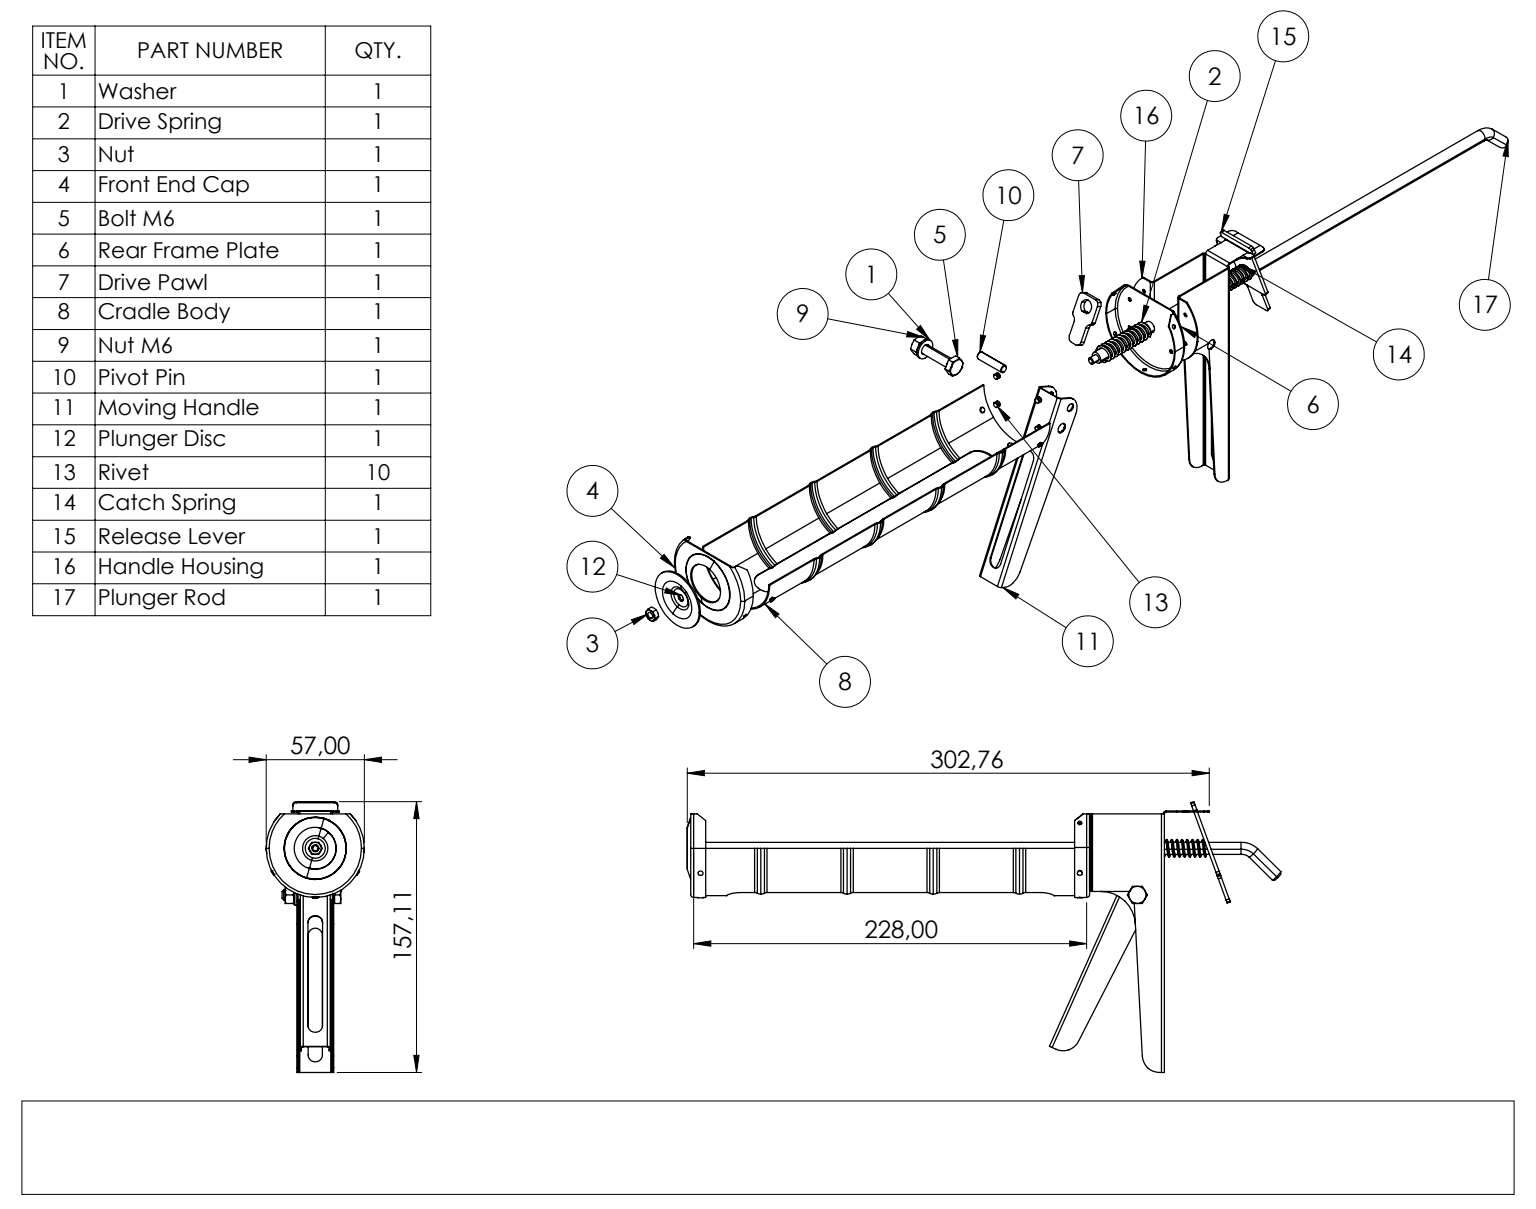
ISO-10303-21;
HEADER;
FILE_DESCRIPTION (('STEP AP214'),
    '1' );
FILE_NAME ('MAS-156',
    '2026-10-06T09:00:30',
    ( '' ),
    ( '' ),
    'SwSTEP 2.0',
    'SolidWorks 2020',
    '' );
FILE_SCHEMA (( 'AUTOMOTIVE_DESIGN' ));
ENDSEC;

DATA;
#1 = CARTESIAN_POINT ( 'NONE',  ( 7.707106781468556100, -5.692566302608600637, -27.29492475672613594 ) ) ;
#2 = DIRECTION ( 'NONE',  ( 0.000000000000000000, 0.9128796883888953273, -0.4082287037029530552 ) ) ;
#3 = CARTESIAN_POINT ( 'NONE',  ( 27.50000000000000000, -6.735334946019999940E-15, 115.0000000000000000 ) ) ;
#4 = EDGE_CURVE ( 'NONE', #19777, #16714, #24382, .T. ) ;
#5 = EDGE_CURVE ( 'NONE', #10372, #13996, #4280, .T. ) ;
#6 = DIRECTION ( 'NONE',  ( -1.000000000000000000, 1.167320209990000089E-13, -2.253435535809999718E-12 ) ) ;
#7 = B_SPLINE_CURVE_WITH_KNOTS ( 'NONE', 5,
 ( #8666, #18262, #27873, #6319, #23164, #13557 ),
 .UNSPECIFIED., .F., .F.,
 ( 6, 6 ),
 ( -2.319814965009999952, 0.000000000000000000 ),
 .UNSPECIFIED. ) ;
#8 = ORIENTED_EDGE ( 'NONE', *, *, #13852, .T. ) ;
#9 = DIRECTION ( 'NONE',  ( -0.7071067811865475727, 0.7071067811865475727, 0.000000000000000000 ) ) ;
#10 = CARTESIAN_POINT ( 'NONE',  ( -15.86372219731129896, -9.538245303637634009, -0.6999999999999785283 ) ) ;
#11 = CARTESIAN_POINT ( 'NONE',  ( 9.499999999614264112, -13.84939817494163350, -36.47165854346829406 ) ) ;
#12 = ORIENTED_EDGE ( 'NONE', *, *, #12651, .T. ) ;
#13 = CARTESIAN_POINT ( 'NONE',  ( 25.25401215818320821, -13.21081861402980273, 4.098596794000014754 ) ) ;
#14 = CARTESIAN_POINT ( 'NONE',  ( 3.314820598666778917, -5.455691467570147779, -47.04669147682499641 ) ) ;
#15 = ORIENTED_EDGE ( 'NONE', *, *, #21844, .F. ) ;
#16 = VERTEX_POINT ( 'NONE', #10421 ) ;
#17 = PRODUCT_DEFINITION ( 'UNKNOWN', '', #18877, #12195 ) ;
#18 = CARTESIAN_POINT ( 'NONE',  ( 0.000000000000000000, 0.000000000000000000, 0.000000000000000000 ) ) ;
#19 = EDGE_LOOP ( 'NONE', ( #14713, #16983, #4133, #2279 ) ) ;
#20 = CARTESIAN_POINT ( 'NONE',  ( -0.8259893079150000261, -28.48844349870000059, 224.2403608809999866 ) ) ;
#21 = ORIENTED_EDGE ( 'NONE', *, *, #30426, .T. ) ;
#22 = CARTESIAN_POINT ( 'NONE',  ( 24.25874038310000103, -14.95904359230000047, 225.7601370010000039 ) ) ;
#23 = CARTESIAN_POINT ( 'NONE',  ( -4.903324624900923467, -10.51181958078580259, -35.69001801787404560 ) ) ;
#24 = FACE_OUTER_BOUND ( 'NONE', #15323, .T. ) ;
#25 = CARTESIAN_POINT ( 'NONE',  ( 0.2753640861538455553, 4.598480474408660257, -35.69999999999998863 ) ) ;
#26 = CARTESIAN_POINT ( 'NONE',  ( 18.18796211431769549, 19.99998853575082336, -0.6839386825886580867 ) ) ;
#27 = EDGE_CURVE ( 'NONE', #20783, #1709, #15444, .T. ) ;
#28 = CARTESIAN_POINT ( 'NONE',  ( -3.876926306394398836, -0.3768009765330506133, -0.6999999999999992895 ) ) ;
#29 = CARTESIAN_POINT ( 'NONE',  ( -6.645959583264284376, -7.251031249533246736, -33.94260493001564782 ) ) ;
#30 = CARTESIAN_POINT ( 'NONE',  ( 1.834951415319072465, -1.057599859260872410, 226.6412452697799438 ) ) ;
#31 = ORIENTED_EDGE ( 'NONE', *, *, #12379, .F. ) ;
#32 = CARTESIAN_POINT ( 'NONE',  ( -5.299969906037439671, -1.662641516789540086, -11.02323088900000769 ) ) ;
#33 = CARTESIAN_POINT ( 'NONE',  ( -4.266767049786682087, -2.157590496602210806, -27.02722909260000961 ) ) ;
#34 = DIRECTION ( 'NONE',  ( 1.000000000000000000, 3.839471067133294241E-11, -1.287095525146219562E-11 ) ) ;
#35 = AXIS2_PLACEMENT_3D ( 'NONE', #27512, #5959, #1254 ) ;
#36 = B_SPLINE_CURVE_WITH_KNOTS ( 'NONE', 3,
 ( #5890, #1034, #22739, #5586, #10623, #27300 ),
 .UNSPECIFIED., .F., .F.,
 ( 4, 2, 4 ),
 ( 0.000000000000000000, 0.5000000000000000000, 1.000000000000000000 ),
 .UNSPECIFIED. ) ;
#37 = CARTESIAN_POINT ( 'NONE',  ( 24.70074545475921823, -14.21822122957610368, 6.002806299999996043 ) ) ;
#38 = CARTESIAN_POINT ( 'NONE',  ( 19.56389002122311638, 19.56882009050699622, 0.5006759800000037952 ) ) ;
#39 = CARTESIAN_POINT ( 'NONE',  ( 5.746322866173966482, -30.90925660337144265, -80.12837891589188644 ) ) ;
#40 = CARTESIAN_POINT ( 'NONE',  ( 3.800013225884302237, -1.579422177728474708, -17.87122516810000405 ) ) ;
#41 = ADVANCED_FACE ( 'NONE', ( #13225 ), #5997, .F. ) ;
#42 = CARTESIAN_POINT ( 'NONE',  ( 17.19192930164915722, 9.890905752024515607, -1.400000000000002132 ) ) ;
#43 = CARTESIAN_POINT ( 'NONE',  ( -24.83401023410189623, -13.98326748962921329, 4.239871886000001311 ) ) ;
#44 = CARTESIAN_POINT ( 'NONE',  ( 1.346291201779999946, -4.118494162357343669, -70.37733883405731206 ) ) ;
#45 = ORIENTED_EDGE ( 'NONE', *, *, #3237, .T. ) ;
#46 = AXIS2_PLACEMENT_3D ( 'NONE', #29369, #26557, #19627 ) ;
#47 = CARTESIAN_POINT ( 'NONE',  ( 0.5184513693225318853, -28.49550581263314086, 3.899998581000013509 ) ) ;
#48 = CARTESIAN_POINT ( 'NONE',  ( -12.32027642597168260, -32.00000000000000711, -27.84664838113162233 ) ) ;
#49 = VERTEX_POINT ( 'NONE', #5842 ) ;
#50 = EDGE_CURVE ( 'NONE', #6418, #21281, #18108, .T. ) ;
#51 = CARTESIAN_POINT ( 'NONE',  ( -20.30403093128963476, 20.00000000003735323, 3.000000106999994642 ) ) ;
#52 = CARTESIAN_POINT ( 'NONE',  ( 1.057488903014505443E-10, -106.9648224075757952, 18.31364292107395642 ) ) ;
#53 = VERTEX_POINT ( 'NONE', #11043 ) ;
#54 = PRODUCT_DEFINITION ( 'UNKNOWN', '', #25430, #25414 ) ;
#55 = VERTEX_POINT ( 'NONE', #6316 ) ;
#56 = ORIENTED_EDGE ( 'NONE', *, *, #13467, .F. ) ;
#57 = EDGE_LOOP ( 'NONE', ( #4561, #8496, #21991, #5977, #22039 ) ) ;
#58 = DIRECTION ( 'NONE',  ( 1.000000000000000000, 0.000000000000000000, 0.000000000000000000 ) ) ;
#59 = DIRECTION ( 'NONE',  ( 0.7071067811865475727, -0.7071067811865475727, 0.000000000000000000 ) ) ;
#60 = CARTESIAN_POINT ( 'NONE',  ( -1.682270644565667439, 2.346032993262427091, -68.02444337080407877 ) ) ;
#61 = VERTEX_POINT ( 'NONE', #24738 ) ;
#62 = CARTESIAN_POINT ( 'NONE',  ( 7.707106781302665688, -60.46534760594231983, -2.801202534548945966 ) ) ;
#63 = CARTESIAN_POINT ( 'NONE',  ( 24.57933163011563238, -12.98840299560160538, 225.3593307347778136 ) ) ;
#64 = EDGE_CURVE ( 'NONE', #9917, #25371, #9300, .T. ) ;
#65 = CARTESIAN_POINT ( 'NONE',  ( 17.83929014045347827, 20.00000000006149392, -1.000005633855494125E-09 ) ) ;
#66 = DIRECTION ( 'NONE',  ( 0.000000000000000000, -0.3420201433259318913, 0.9396926207858126157 ) ) ;
#67 = CARTESIAN_POINT ( 'NONE',  ( 1.127732790480000080, -28.47784299079999926, 225.0000014190000002 ) ) ;
#68 = VERTEX_POINT ( 'NONE', #12776 ) ;
#69 = CARTESIAN_POINT ( 'NONE',  ( -18.27629205756926822, 19.99998488772503080, -0.6746503638753708065 ) ) ;
#70 = EDGE_CURVE ( 'NONE', #662, #13739, #1640, .T. ) ;
#71 = VECTOR ( 'NONE', #9226, 1000.000000000000000 ) ;
#72 = MANIFOLD_SOLID_BREP ( 'PartBody', #5507 ) ;
#73 = CARTESIAN_POINT ( 'NONE',  ( -3.057389860650357338, 5.459897439232808125, -16.07761783620000173 ) ) ;
#74 = CARTESIAN_POINT ( 'NONE',  ( 15.69372571266449512, 10.97998838177520931, -1.972246272986471594 ) ) ;
#75 = CARTESIAN_POINT ( 'NONE',  ( 0.09701118263791908003, -27.50000000070000894, 6.100000000000011191 ) ) ;
#76 = ORIENTED_EDGE ( 'NONE', *, *, #19659, .F. ) ;
#77 = CARTESIAN_POINT ( 'NONE',  ( 16.21564467631812789, 10.42862492216662318, -0.6999999999999785283 ) ) ;
#78 = CARTESIAN_POINT ( 'NONE',  ( 11.39453140432736511, 21.69999999994131912, -70.10000000020002631 ) ) ;
#79 = DIRECTION ( 'NONE',  ( -1.000000000000000000, 0.000000000000000000, -2.253435535809999718E-12 ) ) ;
#80 = EDGE_CURVE ( 'NONE', #20682, #22430, #3324, .T. ) ;
#81 = DIRECTION ( 'NONE',  ( 0.000000000000000000, 0.000000000000000000, 1.000000000000000000 ) ) ;
#82 = CARTESIAN_POINT ( 'NONE',  ( 7.105427357599999217E-15, 3.552713678799999608E-15, 43.21714158840000408 ) ) ;
#83 = CARTESIAN_POINT ( 'NONE',  ( 27.71720220739999974, -1.975806291350000238E-11, 229.4485730569999760 ) ) ;
#84 = CARTESIAN_POINT ( 'NONE',  ( -11.57541201399999942, -14.20905793120000027, 230.6999999999999886 ) ) ;
#85 = EDGE_LOOP ( 'NONE', ( #21526, #26943, #30310, #22481 ) ) ;
#86 = CARTESIAN_POINT ( 'NONE',  ( 25.26810488179999936, 12.77004255139999955, 229.0000000000000000 ) ) ;
#87 = CARTESIAN_POINT ( 'NONE',  ( 27.69999999930000101, -3.392159599989999961E-15, 90.00000000000000000 ) ) ;
#88 = CARTESIAN_POINT ( 'NONE',  ( -27.88265104574380260, 4.289521473631270787, 0.8585786439999909536 ) ) ;
#89 = CARTESIAN_POINT ( 'NONE',  ( -4.778993077004805912, -1.464489131705188019, -68.10000000002500542 ) ) ;
#90 = VERTEX_POINT ( 'NONE', #28021 ) ;
#91 = CARTESIAN_POINT ( 'NONE',  ( 20.67177784749999958, 17.22892977999999786, 230.6999999999999886 ) ) ;
#92 = AXIS2_PLACEMENT_3D ( 'NONE', #8995, #11519, #1614 ) ;
#93 =( LENGTH_UNIT ( ) NAMED_UNIT ( * ) SI_UNIT ( .MILLI., .METRE. ) );
#94 = ORIENTED_EDGE ( 'NONE', *, *, #1377, .F. ) ;
#95 = DIRECTION ( 'NONE',  ( 2.764840495839172918E-12, 0.9128796883888953273, -0.4082287037029530552 ) ) ;
#96 = CARTESIAN_POINT ( 'NONE',  ( 0.2945360517547964130, 4.690762039826936736, -70.15875473022499875 ) ) ;
#97 = VERTEX_POINT ( 'NONE', #25833 ) ;
#98 = CARTESIAN_POINT ( 'NONE',  ( -4.913246905806704312, -2.484498147601009510, -28.96472909259999895 ) ) ;
#99 = CARTESIAN_POINT ( 'NONE',  ( 7.000000000111516130, -60.34578018690756807, -2.533826264242911908 ) ) ;
#100 = CARTESIAN_POINT ( 'NONE',  ( 2.776548632478545553, -3.583402058917904753, -52.50430438132499233 ) ) ;
#101 = ADVANCED_FACE ( 'NONE', ( #28332 ), #9497, .F. ) ;
#102 = CARTESIAN_POINT ( 'NONE',  ( -10.00000000000000000, 21.72305290929948640, -60.97178489257708378 ) ) ;
#103 = CARTESIAN_POINT ( 'NONE',  ( 17.95841148951064525, -9.763538383420391042, -0.6999999999999784173 ) ) ;
#104 = CARTESIAN_POINT ( 'NONE',  ( 24.55806919409999978, -14.46257963250000067, 223.9201486480000085 ) ) ;
#105 = DIRECTION ( 'NONE',  ( -1.000000000000000000, 5.687697937797165957E-16, -6.771501495045624776E-12 ) ) ;
#106 = EDGE_CURVE ( 'NONE', #11838, #4649, #28678, .T. ) ;
#107 = EDGE_CURVE ( 'NONE', #7680, #17625, #27535, .T. ) ;
#108 = CARTESIAN_POINT ( 'NONE',  ( 0.000000000000000000, 0.000000000000000000, 229.2412452700000074 ) ) ;
#109 = ORIENTED_EDGE ( 'NONE', *, *, #22749, .F. ) ;
#110 = CARTESIAN_POINT ( 'NONE',  ( -10.99999999969999998, 20.99999999999999645, -58.51619611000000276 ) ) ;
#111 = CARTESIAN_POINT ( 'NONE',  ( 24.34123158960000310, -14.82477075290000101, 225.9012998019999827 ) ) ;
#112 = CARTESIAN_POINT ( 'NONE',  ( -12.01652311039999965, 1.520041121179999788, 231.9999989789999972 ) ) ;
#113 = CARTESIAN_POINT ( 'NONE',  ( -9.000000000000000000, -130.0000000000000000, -44.10000000000000142 ) ) ;
#114 = AXIS2_PLACEMENT_3D ( 'NONE', #11940, #28625, #12094 ) ;
#115 = CARTESIAN_POINT ( 'NONE',  ( -3.552713678799999608E-15, 0.000000000000000000, 193.2171415880000040 ) ) ;
#116 = CARTESIAN_POINT ( 'NONE',  ( -6.000000000000000000, -30.08462078616447499, -79.82823602431849963 ) ) ;
#117 = CARTESIAN_POINT ( 'NONE',  ( 24.40260331739102639, -13.31784478726558163, 224.1134674150510477 ) ) ;
#118 = CARTESIAN_POINT ( 'NONE',  ( -8.261799387992772026, -15.86465192213916353, -74.65259062561661096 ) ) ;
#119 = CARTESIAN_POINT ( 'NONE',  ( -24.32472894358752313, 13.45989150749028873, 3.899998581000013509 ) ) ;
#120 = CARTESIAN_POINT ( 'NONE',  ( 1.007237960741799165, 1.747572776708515185, 227.6412452700616598 ) ) ;
#121 = MANIFOLD_SOLID_BREP ( 'Stock-MAS-156-1', #21607 ) ;
#122 = CARTESIAN_POINT ( 'NONE',  ( 8.999999999800001760, 21.69999999998272244, -51.75615994398976483 ) ) ;
#123 = CARTESIAN_POINT ( 'NONE',  ( 17.93011078765611543, -8.208160914697428368, -0.6999999999999784173 ) ) ;
#124 = CARTESIAN_POINT ( 'NONE',  ( 7.291979204365766520, -115.1332600680515981, 21.92702704693240179 ) ) ;
#125 = VERTEX_POINT ( 'NONE', #7091 ) ;
#126 = CARTESIAN_POINT ( 'NONE',  ( 19.80526555972147307, 19.50877392102524155, 1.800000000000023803 ) ) ;
#127 = ORIENTED_EDGE ( 'NONE', *, *, #8933, .T. ) ;
#128 = DIRECTION ( 'NONE',  ( -0.000000000000000000, -0.000000000000000000, -1.000000000000000000 ) ) ;
#129 = AXIS2_PLACEMENT_3D ( 'NONE', #21311, #28843, #21003 ) ;
#130 = EDGE_CURVE ( 'NONE', #97, #8033, #30399, .T. ) ;
#131 = CARTESIAN_POINT ( 'NONE',  ( -5.110483438867316153, -2.062468175234513534, -60.18491726642499628 ) ) ;
#132 = ORIENTED_EDGE ( 'NONE', *, *, #23382, .F. ) ;
#133 = EDGE_CURVE ( 'NONE', #7914, #29606, #10076, .T. ) ;
#134 = CONTEXT_DEPENDENT_SHAPE_REPRESENTATION ( #24876, #24989 ) ;
#135 = ORIENTED_EDGE ( 'NONE', *, *, #1841, .T. ) ;
#136 = CARTESIAN_POINT ( 'NONE',  ( -7.000000000050451199, -115.5267901941139144, 21.04701626956108029 ) ) ;
#137 = ORIENTED_EDGE ( 'NONE', *, *, #11511, .F. ) ;
#138 = CARTESIAN_POINT ( 'NONE',  ( 28.49999999979999998, 4.443028818220000176, 229.0000000000000000 ) ) ;
#139 = CARTESIAN_POINT ( 'NONE',  ( 0.000000000000000000, 5.495185456771864096, -69.00660115587162124 ) ) ;
#140 = CARTESIAN_POINT ( 'NONE',  ( 5.010073463369999480, 11.17224087250000153, 232.6627648150000027 ) ) ;
#141 = CYLINDRICAL_SURFACE ( 'NONE', #31028, 3.749999999999999556 ) ;
#142 = CARTESIAN_POINT ( 'NONE',  ( -3.010188847181571870, -5.300177381000955812, -6.685065142700001850 ) ) ;
#143 = CIRCLE ( 'NONE', #28760, 2.000000000000000000 ) ;
#144 = DIRECTION ( 'NONE',  ( -0.6941258031311203780, -0.7198537139083029945, 0.000000000000000000 ) ) ;
#145 = VERTEX_POINT ( 'NONE', #2379 ) ;
#146 = CARTESIAN_POINT ( 'NONE',  ( -0.9130200810698786418, -4.996423850591022564, -44.10000000002499121 ) ) ;
#147 = CARTESIAN_POINT ( 'NONE',  ( -3.665401116828205463, 4.874126016103034864, -20.23064294440001021 ) ) ;
#148 = CARTESIAN_POINT ( 'NONE',  ( 4.000000000000000000, -31.49740633216590524, -81.40662568294101220 ) ) ;
#149 = CARTESIAN_POINT ( 'NONE',  ( 0.4908581387334869928, -27.49541710664063032, 225.9948832293035537 ) ) ;
#150 = AXIS2_PLACEMENT_3D ( 'NONE', #9380, #9854, #2162 ) ;
#151 = CARTESIAN_POINT ( 'NONE',  ( 4.000000000000000000, -29.96004123392021157, -79.78289277550334191 ) ) ;
#152 = DIRECTION ( 'NONE',  ( 0.000000000000000000, 1.000000000000000000, 0.000000000000000000 ) ) ;
#153 = CARTESIAN_POINT ( 'NONE',  ( -18.31085446006445494, 19.88197403644849004, 0.02160863700001458554 ) ) ;
#154 = CARTESIAN_POINT ( 'NONE',  ( 4.638687372181960811, -19.47448025771016233, -31.31863632548023801 ) ) ;
#155 = DIRECTION ( 'NONE',  ( 0.000000000000000000, 0.000000000000000000, -1.000000000000000000 ) ) ;
#156 = DIRECTION ( 'NONE',  ( 1.000000000000000000, -0.000000000000000000, -2.257150022439999944E-12 ) ) ;
#157 = EDGE_CURVE ( 'NONE', #11921, #14079, #9072, .T. ) ;
#158 = CARTESIAN_POINT ( 'NONE',  ( 8.999999999770000869, 20.92262005359999577, -43.64010329495499718 ) ) ;
#159 = B_SPLINE_CURVE_WITH_KNOTS ( 'NONE', 3,
 ( #30867, #2535, #9297, #23951 ),
 .UNSPECIFIED., .F., .F.,
 ( 4, 4 ),
 ( 0.000000000000000000, 1.000000000000000000 ),
 .UNSPECIFIED. ) ;
#160 = ORIENTED_EDGE ( 'NONE', *, *, #26147, .F. ) ;
#161 = CARTESIAN_POINT ( 'NONE',  ( 0.6138679561251692007, 4.311712124478117580, -29.00600711720001357 ) ) ;
#162 = FACE_BOUND ( 'NONE', #6310, .T. ) ;
#163 = ORIENTED_EDGE ( 'NONE', *, *, #204, .F. ) ;
#164 = FACE_OUTER_BOUND ( 'NONE', #30752, .T. ) ;
#165 = CARTESIAN_POINT ( 'NONE',  ( 3.314820598666778917, -5.455691467570147779, -46.56669147682499954 ) ) ;
#166 = ORIENTED_EDGE ( 'NONE', *, *, #29617, .T. ) ;
#167 = EDGE_CURVE ( 'NONE', #31001, #29368, #18432, .T. ) ;
#168 = ORIENTED_EDGE ( 'NONE', *, *, #10296, .F. ) ;
#169 = CARTESIAN_POINT ( 'NONE',  ( 0.000000000000000000, 0.000000000000000000, 0.000000000000000000 ) ) ;
#170 = VERTEX_POINT ( 'NONE', #24397 ) ;
#171 = CARTESIAN_POINT ( 'NONE',  ( -17.59696554489119080, -9.791838634853515799, 0.000000000000000000 ) ) ;
#172 = ADVANCED_BREP_SHAPE_REPRESENTATION ( '', ( #20871, #17722 ), #24361 ) ;
#173 = ORIENTED_EDGE ( 'NONE', *, *, #3047, .T. ) ;
#174 = CARTESIAN_POINT ( 'NONE',  ( 23.47715715134837211, -20.00370206646827498, 1.000000000000000888 ) ) ;
#175 = CARTESIAN_POINT ( 'NONE',  ( -6.661312627754256255, -8.560122214784900763, -36.64192442629084212 ) ) ;
#176 = CARTESIAN_POINT ( 'NONE',  ( 19.80526555972147307, 19.50877392102524155, 8.000000000000007105 ) ) ;
#177 = CARTESIAN_POINT ( 'NONE',  ( 0.4017848704880546684, 4.295537307870551658, -35.69999999999999574 ) ) ;
#178 = CARTESIAN_POINT ( 'NONE',  ( 19.37011161855012986, 20.00004249230521935, -0.3429596948707999693 ) ) ;
#179 = CARTESIAN_POINT ( 'NONE',  ( -24.00289803497245700, 14.02635913871703011, 5.901399683999997592 ) ) ;
#180 = CARTESIAN_POINT ( 'NONE',  ( -4.861312627776431583, -9.716283825163692711, -32.74022090983473987 ) ) ;
#181 = CARTESIAN_POINT ( 'NONE',  ( -10.69999999996051798, -35.47467438098505710, -24.90706660654935689 ) ) ;
#182 = ORIENTED_EDGE ( 'NONE', *, *, #19559, .F. ) ;
#183 = CARTESIAN_POINT ( 'NONE',  ( 3.834994720502944876, -2.823021758520125601, -9.910276792900003073 ) ) ;
#184 = CARTESIAN_POINT ( 'NONE',  ( -5.505691776210679400, -0.009179722898969058451, -27.16856466009999238 ) ) ;
#185 = DIRECTION ( 'NONE',  ( 0.000000000000000000, -2.257145581549999994E-12, -1.000000000000000000 ) ) ;
#186 = EDGE_CURVE ( 'NONE', #24695, #19740, #19204, .T. ) ;
#187 = LINE ( 'NONE', #21734, #27735 ) ;
#188 = LINE ( 'NONE', #19684, #28372 ) ;
#189 = LINE ( 'NONE', #19380, #24692 ) ;
#190 = CARTESIAN_POINT ( 'NONE',  ( 8.566424601805415762, -26.13212873426111216, 23.30748548239859019 ) ) ;
#191 = CARTESIAN_POINT ( 'NONE',  ( 3.486358836775539594, -2.566383416802844319, -8.972776792899997744 ) ) ;
#192 = AXIS2_PLACEMENT_3D ( 'NONE', #23801, #30571, #26003 ) ;
#193 = CIRCLE ( 'NONE', #5696, 0.9999999999999991118 ) ;
#194 = CARTESIAN_POINT ( 'NONE',  ( 9.999999999959999997, -24.87868334570000073, -26.27868334529999927 ) ) ;
#195 = CARTESIAN_POINT ( 'NONE',  ( -0.6197578587862698773, -3.499936541734924411, 230.8124538892490136 ) ) ;
#196 = ORIENTED_EDGE ( 'NONE', *, *, #30807, .F. ) ;
#197 = PLANE ( 'NONE',  #19813 ) ;
#198 = CARTESIAN_POINT ( 'NONE',  ( 16.37473331889771089, 11.76353838340827984, 0.000000000000000000 ) ) ;
#199 = ORIENTED_EDGE ( 'NONE', *, *, #6289, .F. ) ;
#200 = CARTESIAN_POINT ( 'NONE',  ( 25.11738521000000190, -13.46751580659999981, 225.6806823370000075 ) ) ;
#201 = DIRECTION ( 'NONE',  ( 0.000000000000000000, 0.3420201433259318913, -0.9396926207858126157 ) ) ;
#202 = EDGE_LOOP ( 'NONE', ( #3283, #15747, #28522, #14669, #12113 ) ) ;
#203 = ORIENTED_EDGE ( 'NONE', *, *, #5628, .T. ) ;
#204 = EDGE_CURVE ( 'NONE', #15790, #12797, #14647, .T. ) ;
#205 = ORIENTED_EDGE ( 'NONE', *, *, #16530, .T. ) ;
#206 = ORIENTED_EDGE ( 'NONE', *, *, #14101, .F. ) ;
#207 = CARTESIAN_POINT ( 'NONE',  ( 7.099269075060530731, -8.189196033044112255, -36.82283721307814517 ) ) ;
#208 = VECTOR ( 'NONE', #27934, 1000.000000000000114 ) ;
#209 = CARTESIAN_POINT ( 'NONE',  ( -5.361385120510000490, 31.61859227569999931, 222.0000000000000000 ) ) ;
#211 = CARTESIAN_POINT ( 'NONE',  ( -19.29999999990000248, -25.07317073083999759, -28.39999999989999324 ) ) ;
#210 = CIRCLE ( 'NONE', #706, 27.69999999999999929 ) ;
#212 = CIRCLE ( 'NONE', #1212, 2.299999999999999822 ) ;
#213 = ORIENTED_EDGE ( 'NONE', *, *, #13656, .T. ) ;
#214 = CARTESIAN_POINT ( 'NONE',  ( -24.82162973577514364, 12.51998933611906573, 5.310645680000003921 ) ) ;
#215 = CIRCLE ( 'NONE', #4748, 1.500000000000000222 ) ;
#216 = CIRCLE ( 'NONE', #11262, 3.491271820589999741 ) ;
#217 = CARTESIAN_POINT ( 'NONE',  ( 24.50095082274352265, -13.13603084652294051, 225.6822660555842219 ) ) ;
#218 = LINE ( 'NONE', #7132, #8498 ) ;
#219 = CARTESIAN_POINT ( 'NONE',  ( 3.040504021322313122, 1.733590290792417887, 0.000000000000000000 ) ) ;
#220 = ADVANCED_FACE ( 'NONE', ( #19519 ), #21819, .T. ) ;
#221 = CARTESIAN_POINT ( 'NONE',  ( 2.051456227667985299, -4.656424856567735304, -0.7000710907721876541 ) ) ;
#222 = ORIENTED_EDGE ( 'NONE', *, *, #2639, .F. ) ;
#223 = DIRECTION ( 'NONE',  ( 1.000000000000000000, -1.843431230200084908E-12, 2.650498504963248473E-12 ) ) ;
#224 = EDGE_CURVE ( 'NONE', #17932, #4565, #12425, .T. ) ;
#225 = B_SPLINE_CURVE_WITH_KNOTS ( 'NONE', 3,
 ( #19407, #7594, #2874, #4928, #17039, #25916 ),
 .UNSPECIFIED., .F., .F.,
 ( 4, 2, 4 ),
 ( 0.000000000000000000, 0.5000000000000000000, 1.000000000000000000 ),
 .UNSPECIFIED. ) ;
#226 = CARTESIAN_POINT ( 'NONE',  ( -5.990533020055879732, -1.129328118392731950, -16.09949426530000238 ) ) ;
#227 = DIRECTION ( 'NONE',  ( 1.000000000000000000, -1.843431230200084908E-12, 2.650498504963248473E-12 ) ) ;
#228 = CARTESIAN_POINT ( 'NONE',  ( 26.93395403039999891, -3.298349123909999533E-15, 87.75675929330000713 ) ) ;
#229 = DIRECTION ( 'NONE',  ( -0.1090476345695678556, -0.6986477033489640887, -0.7071067811865474617 ) ) ;
#230 = CARTESIAN_POINT ( 'NONE',  ( -10.69999999930000101, -30.00000000000000000, -28.40000000000000213 ) ) ;
#231 = CARTESIAN_POINT ( 'NONE',  ( 22.70032920257776254, -14.24644155109503885, 5.491373161944450132 ) ) ;
#232 = EDGE_CURVE ( 'NONE', #14788, #6922, #2831, .T. ) ;
#233 = LINE ( 'NONE', #19574, #18492 ) ;
#234 = DIRECTION ( 'NONE',  ( -1.000000000000000000, 0.000000000000000000, 0.000000000000000000 ) ) ;
#235 = CARTESIAN_POINT ( 'NONE',  ( 21.99374050320000151, 17.63454380109999775, 229.1414208810000162 ) ) ;
#236 = CARTESIAN_POINT ( 'NONE',  ( -8.000000000474178918, -29.73863906514523947, -27.17531388891475075 ) ) ;
#237 = AXIS2_PLACEMENT_3D ( 'NONE', #28809, #7419, #7570 ) ;
#238 = EDGE_LOOP ( 'NONE', ( #5235, #17859 ) ) ;
#239 = CARTESIAN_POINT ( 'NONE',  ( 22.83443070970000122, 16.43389729289999934, 229.0000000010000178 ) ) ;
#240 = AXIS2_PLACEMENT_3D ( 'NONE', #28736, #7186, #4980 ) ;
#241 = AXIS2_PLACEMENT_3D ( 'NONE', #12449, #26774, #973 ) ;
#242 = AXIS2_PLACEMENT_3D ( 'NONE', #1141, #8056, #25215 ) ;
#243 = AXIS2_PLACEMENT_3D ( 'NONE', #30286, #20689, #17993 ) ;
#244 = DIRECTION ( 'NONE',  ( 0.9880370573969197157, -0.1542166437529880196, 2.958228394580000263E-31 ) ) ;
#245 = ADVANCED_FACE ( 'NONE', ( #491 ), #28838, .T. ) ;
#246 = CARTESIAN_POINT ( 'NONE',  ( -4.889194147463507001, -0.6752612934842897596, -68.10000000002499121 ) ) ;
#247 = ORIENTED_EDGE ( 'NONE', *, *, #6735, .T. ) ;
#248 = CARTESIAN_POINT ( 'NONE',  ( 2.914123423709013228, 2.127246859543532764, -88.52261276242110455 ) ) ;
#249 = ORIENTED_EDGE ( 'NONE', *, *, #27861, .T. ) ;
#250 = LINE ( 'NONE', #26663, #23008 ) ;
#251 = CARTESIAN_POINT ( 'NONE',  ( -4.287590041606510916, 1.413705153860731034, -68.74019511502500279 ) ) ;
#252 = ORIENTED_EDGE ( 'NONE', *, *, #15221, .F. ) ;
#253 = CARTESIAN_POINT ( 'NONE',  ( 4.370697773661016861, 1.580342671372844787, -26.51249766020000109 ) ) ;
#254 = CARTESIAN_POINT ( 'NONE',  ( -18.80686365405603055, 19.99999823163966184, -0.5856999480000069092 ) ) ;
#255 = EDGE_CURVE ( 'NONE', #7386, #15620, #13185, .T. ) ;
#256 = DIRECTION ( 'NONE',  ( -2.764840495839172918E-12, -0.9128796883888953273, 0.4082287037029531107 ) ) ;
#257 = B_SPLINE_SURFACE_WITH_KNOTS ( 'NONE', 5, 1, ( 
 ( #21157, #21469 ),
 ( #23836, #30754 ),
 ( #16430, #9183 ),
 ( #14231, #2282 ),
 ( #11866, #28394 ),
 ( #6831, #11711 ),
 ( #21312, #7144 ),
 ( #26039, #4479 ),
 ( #11245, #28076 ),
 ( #9342, #20853 ),
 ( #18943, #26346 ),
 ( #4794, #7602 ),
 ( #19727, #10128 ),
 ( #21937, #19414 ),
 ( #26800, #17195 ) ),
 .UNSPECIFIED., .F., .F., .F.,
 ( 6, 3, 3, 3, 6 ),
 ( 2, 2 ),
 ( 0.000000000000000000, 0.5239015562240000312, 1.047803112450000018, 1.571704668670000027, 1.746338520749999956 ),
 ( -0.7000000000009999335, 2.556819966299999618E-06 ),
 .UNSPECIFIED. ) ;
#258 = CARTESIAN_POINT ( 'NONE',  ( 4.545032752014871669, -0.3361547907463971474, -49.12442242802499237 ) ) ;
#259 = CARTESIAN_POINT ( 'NONE',  ( 8.000000000495651520, -23.99023929168359714, -28.09088344023833983 ) ) ;
#260 = VECTOR ( 'NONE', #12799, 1000.000000000000000 ) ;
#261 =( LENGTH_UNIT ( ) NAMED_UNIT ( * ) SI_UNIT ( .MILLI., .METRE. ) );
#262 = DIRECTION ( 'NONE',  ( -0.9595496299847263710, 0.2815395311429191305, 0.000000000000000000 ) ) ;
#263 = PRODUCT_DEFINITION_CONTEXT ( 'detailed design', #6356, 'design' ) ;
#264 = DIRECTION ( 'NONE',  ( 0.000000000000000000, 0.000000000000000000, -1.000000000000000000 ) ) ;
#265 = CARTESIAN_POINT ( 'NONE',  ( -17.49268987146206555, -21.99976866032092460, -27.95151664070907316 ) ) ;
#266 = ORIENTED_EDGE ( 'NONE', *, *, #25247, .T. ) ;
#267 = DIRECTION ( 'NONE',  ( -1.000000000000000000, 0.000000000000000000, 0.000000000000000000 ) ) ;
#268 = CARTESIAN_POINT ( 'NONE',  ( 8.700000000289421109, -16.34566964816854195, -38.02266470773063389 ) ) ;
#269 = CARTESIAN_POINT ( 'NONE',  ( -23.23277126416379801, -15.26692729116844482, 5.104183903000020450 ) ) ;
#270 = CARTESIAN_POINT ( 'NONE',  ( -26.95773186790000153, 8.656139628340000058, 223.3999999999999773 ) ) ;
#271 = DIRECTION ( 'NONE',  ( 0.000000000000000000, 0.000000000000000000, 1.000000000000000000 ) ) ;
#272 = STYLED_ITEM ( 'NONE', ( #2224 ), #72 ) ;
#273 = CARTESIAN_POINT ( 'NONE',  ( -8.699999999730765765, -25.41515418226572365, -25.82241997913822473 ) ) ;
#274 = LINE ( 'NONE', #1578, #23781 ) ;
#275 = CARTESIAN_POINT ( 'NONE',  ( -4.583497702006505747, -30.37373325290905868, -0.6577119969999878357 ) ) ;
#276 = CARTESIAN_POINT ( 'NONE',  ( 0.9565336475350260104, -27.48338672371320612, 4.451904520592202097 ) ) ;
#277 = CONICAL_SURFACE ( 'NONE', #23882, 4.987531172069999741, 1.047197551199999799 ) ;
#278 = STYLED_ITEM ( 'NONE', ( #27092 ), #24185 ) ;
#279 = CARTESIAN_POINT ( 'NONE',  ( 28.49528339128749366, 0.5184828350247753237, 8.000000000000007105 ) ) ;
#280 = CARTESIAN_POINT ( 'NONE',  ( 23.65332633301680687, -14.60697862033088512, 225.7326966119605061 ) ) ;
#281 = CARTESIAN_POINT ( 'NONE',  ( 8.903108651239925564, -22.82508830966962421, 140.0000000000000000 ) ) ;
#282 = CARTESIAN_POINT ( 'NONE',  ( -16.81618662976075740, -7.899504219251200610, 0.000000000000000000 ) ) ;
#283 = CARTESIAN_POINT ( 'NONE',  ( 24.86822223037987456, 13.92223202030449691, 5.680679506000013923 ) ) ;
#284 = EDGE_CURVE ( 'NONE', #12548, #25224, #27851, .T. ) ;
#285 = ORIENTED_EDGE ( 'NONE', *, *, #4802, .T. ) ;
#286 = CARTESIAN_POINT ( 'NONE',  ( 20.30396079662882158, 20.00000000004802203, 2.200000000000007283 ) ) ;
#287 = ADVANCED_FACE ( 'NONE', ( #20132 ), #22799, .T. ) ;
#288 = B_SPLINE_CURVE_WITH_KNOTS ( 'NONE', 3,
 ( #27666, #1871, #22960, #8785, #25480, #25320 ),
 .UNSPECIFIED., .F., .F.,
 ( 4, 2, 4 ),
 ( 0.000000000000000000, 0.5000000000000000000, 1.000000000000000000 ),
 .UNSPECIFIED. ) ;
#289 = CARTESIAN_POINT ( 'NONE',  ( -24.87138426050000106, -13.91768300640000078, 223.9574921340000060 ) ) ;
#290 = ORIENTED_EDGE ( 'NONE', *, *, #7961, .T. ) ;
#291 = EDGE_CURVE ( 'NONE', #28488, #24538, #21849, .T. ) ;
#292 = CARTESIAN_POINT ( 'NONE',  ( 24.30716200859999887, -13.49132717699999873, 226.0027513979999867 ) ) ;
#293 = CARTESIAN_POINT ( 'NONE',  ( -0.06606756225350368661, 5.646037861211643083, -57.79818518972499675 ) ) ;
#294 = ORIENTED_EDGE ( 'NONE', *, *, #26070, .F. ) ;
#295 = ORIENTED_EDGE ( 'NONE', *, *, #24858, .F. ) ;
#296 = CARTESIAN_POINT ( 'NONE',  ( -17.49199711315135986, -24.60220466956999985, -24.01086508779000184 ) ) ;
#297 = ORIENTED_EDGE ( 'NONE', *, *, #4833, .F. ) ;
#298 = PRESENTATION_LAYER_ASSIGNMENT (  '', '', ( #23411 ) ) ;
#299 = ORIENTED_EDGE ( 'NONE', *, *, #13486, .T. ) ;
#300 = DIRECTION ( 'NONE',  ( -1.224606353819999829E-16, -1.000000000000000000, 0.000000000000000000 ) ) ;
#301 = CARTESIAN_POINT ( 'NONE',  ( -27.79539923781684507, -0.5057481689249115897, 6.600000000000022737 ) ) ;
#302 = CARTESIAN_POINT ( 'NONE',  ( 8.575788938069999645, 8.809323376420000073, 232.6627648150000027 ) ) ;
#303 = B_SPLINE_CURVE_WITH_KNOTS ( 'NONE', 3,
 ( #7112, #10096, #12136, #9624, #26931, #23962, #26313, #16696, #28976, #19692, #29276, #195, #19386, #5366, #24571, #11984, #24252, #21910, #9939, #19542, #7719, #4759, #14973, #3006, #12599, #31031 ),
 .UNSPECIFIED., .F., .F.,
 ( 4, 2, 2, 1, 1, 2, 2, 2, 2, 2, 1, 1, 2, 2, 4 ),
 ( 0.000000000000000000, 0.1250000000000129896, 0.1875000000000214828, 0.2187500000000258127, 0.2343750000000295874, 0.2421875000000298650, 0.2500000000000301426, 0.5000000000000094369, 0.6249999999999991118, 0.6874999999999938938, 0.7187499999999913403, 0.7343749999999900080, 0.7421874999999908962, 0.7499999999999916733, 1.000000000000000000 ),
 .UNSPECIFIED. ) ;
#304 = DIRECTION ( 'NONE',  ( 0.000000000000000000, 0.000000000000000000, 1.000000000000000000 ) ) ;
#305 = CARTESIAN_POINT ( 'NONE',  ( -0.8919388126321509125, 6.008950160842678301, -10.86772091660000150 ) ) ;
#306 = CARTESIAN_POINT ( 'NONE',  ( 28.49999999970000175, -7.466149220240000162, 229.2404163060000144 ) ) ;
#307 = ORIENTED_EDGE ( 'NONE', *, *, #28551, .T. ) ;
#308 = CARTESIAN_POINT ( 'NONE',  ( 0.7512103448916097603, -4.944508214582001848, -44.10000000002501253 ) ) ;
#309 = CARTESIAN_POINT ( 'NONE',  ( -24.96253706803760153, -13.75225324404262572, 4.689458291000009105 ) ) ;
#310 = CARTESIAN_POINT ( 'NONE',  ( -2.227024806490494946, -3.476280271252722542, -19.20544088820001249 ) ) ;
#311 = CARTESIAN_POINT ( 'NONE',  ( -0.9568679087069641431, 3.499999999999999556, 230.7624477058865295 ) ) ;
#312 = CARTESIAN_POINT ( 'NONE',  ( 1.087768546295719840, -27.47890868157812605, 225.2179249496743978 ) ) ;
#313 = CARTESIAN_POINT ( 'NONE',  ( -9.502613819449999610, 7.533418146720000763, 230.6412452697800006 ) ) ;
#314 = CARTESIAN_POINT ( 'NONE',  ( 8.903108651239925564, -22.82508830966962421, 40.00000000000000000 ) ) ;
#315 = CARTESIAN_POINT ( 'NONE',  ( 2.295476649252899293, -3.592865671589305698, -43.56966640442499994 ) ) ;
#316 = CARTESIAN_POINT ( 'NONE',  ( -10.69999999999999929, -120.5233595621999996, -31.26042064940000387 ) ) ;
#317 = DIRECTION ( 'NONE',  ( 0.9316362575375356503, 0.3633921898465274913, 0.000000000000000000 ) ) ;
#318 = CARTESIAN_POINT ( 'NONE',  ( 10.99289321870000080, -2.500000000000002220, -1.692893218799999877 ) ) ;
#319 = CARTESIAN_POINT ( 'NONE',  ( -24.34385441500000269, 13.50419739129999996, 229.9172023120000006 ) ) ;
#320 = CARTESIAN_POINT ( 'NONE',  ( 8.999999999770000869, 20.38323484520000051, -43.42699808786800020 ) ) ;
#321 = EDGE_LOOP ( 'NONE', ( #8069, #252, #28865, #19891 ) ) ;
#322 = CARTESIAN_POINT ( 'NONE',  ( 3.499930668453409055, 4.992711500635231836, -29.81106724380000372 ) ) ;
#323 = ADVANCED_FACE ( 'NONE', ( #27664 ), #10999, .T. ) ;
#324 = FACE_OUTER_BOUND ( 'NONE', #14055, .T. ) ;
#325 = ORIENTED_EDGE ( 'NONE', *, *, #21114, .F. ) ;
#326 = CARTESIAN_POINT ( 'NONE',  ( 25.05552768372066907, -13.58331698798256504, 3.920132093000017193 ) ) ;
#327 = CARTESIAN_POINT ( 'NONE',  ( -3.250950776947242993, -3.159825117472811140, -47.60083066912499561 ) ) ;
#328 = EDGE_LOOP ( 'NONE', ( #29249, #19391, #9540, #3873 ) ) ;
#329 = EDGE_LOOP ( 'NONE', ( #30586, #15478, #7122, #23473 ) ) ;
#330 = DIRECTION ( 'NONE',  ( 0.000000000000000000, 0.000000000000000000, 1.000000000000000000 ) ) ;
#331 = B_SPLINE_CURVE_WITH_KNOTS ( 'NONE', 4,
 ( #20135, #6279, #8153, #24861, #17748 ),
 .UNSPECIFIED., .F., .F.,
 ( 5, 5 ),
 ( -0.9817477042469999748, 0.9817477042469999748 ),
 .UNSPECIFIED. ) ;
#332 = ORIENTED_EDGE ( 'NONE', *, *, #29953, .F. ) ;
#333 = CARTESIAN_POINT ( 'NONE',  ( -0.07056952541350000607, -28.50017087330000010, 223.9013489249999793 ) ) ;
#334 = EDGE_LOOP ( 'NONE', ( #15122, #20536, #2916, #30946, #21769, #8369 ) ) ;
#335 = CARTESIAN_POINT ( 'NONE',  ( 17.14656078599760392, 12.09981795542235439, -0.6999999999999784173 ) ) ;
#336 =( NAMED_UNIT ( * ) PLANE_ANGLE_UNIT ( ) SI_UNIT ( $, .RADIAN. ) );
#337 = DIRECTION ( 'NONE',  ( -1.000000000000000000, 5.687697913155423197E-16, -6.771501495041734442E-12 ) ) ;
#338 = CARTESIAN_POINT ( 'NONE',  ( 0.6569784070868507353, 4.711013504487742587, -35.69999999999999574 ) ) ;
#339 = SHAPE_REPRESENTATION ( 'Nut', ( #17722 ), #14741 ) ;
#340 = CARTESIAN_POINT ( 'NONE',  ( -12.38103409318611270, -30.48833240864483685, -24.64074601757454630 ) ) ;
#341 = CARTESIAN_POINT ( 'NONE',  ( 9.499999999713729437, -18.10015590263875396, -36.47860036342770229 ) ) ;
#342 = CARTESIAN_POINT ( 'NONE',  ( -23.20948082139999968, -13.40000000000000036, 6.099999999630000502 ) ) ;
#343 = FACE_OUTER_BOUND ( 'NONE', #7511, .T. ) ;
#344 = ORIENTED_EDGE ( 'NONE', *, *, #5154, .T. ) ;
#345 = CARTESIAN_POINT ( 'NONE',  ( -3.630162863991666988, -2.403661707492382060, -7.389929326000004295 ) ) ;
#346 = CARTESIAN_POINT ( 'NONE',  ( 0.8594151385421661127, 6.036396974313712249, -29.00600711719999936 ) ) ;
#347 = CARTESIAN_POINT ( 'NONE',  ( -1.108738578190967550, -3.350312884103880950, 0.000000000000000000 ) ) ;
#348 = LINE ( 'NONE', #2999, #25253 ) ;
#349 = CARTESIAN_POINT ( 'NONE',  ( 23.83639842146205368, 14.30623132797946084, 6.099998581000020792 ) ) ;
#350 = PRESENTATION_STYLE_ASSIGNMENT (( #5052 ) ) ;
#351 = CARTESIAN_POINT ( 'NONE',  ( 8.414407093329970166, -26.18160851622837981, 23.09437632025412412 ) ) ;
#352 = CARTESIAN_POINT ( 'NONE',  ( 3.619519562537643065, 2.908736503316577959, -8.354586408000006514 ) ) ;
#353 = EDGE_CURVE ( 'NONE', #27389, #17896, #14711, .T. ) ;
#354 = B_SPLINE_SURFACE_WITH_KNOTS ( 'NONE', 5, 1, ( 
 ( #10886, #5534 ),
 ( #25047, #15138 ),
 ( #29454, #22387 ),
 ( #22540, #832 ),
 ( #10575, #22684 ),
 ( #7887, #24739 ) ),
 .UNSPECIFIED., .F., .F., .F.,
 ( 6, 6 ),
 ( 2, 2 ),
 ( 0.000000000000000000, 2.000000000000000000 ),
 ( 4.440892098500000003E-16, 0.7000000000030000002 ),
 .UNSPECIFIED. ) ;
#355 = CARTESIAN_POINT ( 'NONE',  ( 12.80098767942999771, -22.00000000000000000, -31.28675134584999640 ) ) ;
#356 =( REPRESENTATION_RELATIONSHIP ('NONE','NONE', #2712, #527 ) REPRESENTATION_RELATIONSHIP_WITH_TRANSFORMATION ( #7357 )SHAPE_REPRESENTATION_RELATIONSHIP( ) );
#357 = LINE ( 'NONE', #17016, #5202 ) ;
#358 = DIRECTION ( 'NONE',  ( 1.000000000000000000, 0.000000000000000000, 0.000000000000000000 ) ) ;
#359 = VERTEX_POINT ( 'NONE', #2030 ) ;
#360 = LINE ( 'NONE', #2855, #2718 ) ;
#361 = CARTESIAN_POINT ( 'NONE',  ( -12.41750254862020952, -32.00000000000000711, -29.79893583387511669 ) ) ;
#362 = ORIENTED_EDGE ( 'NONE', *, *, #25331, .T. ) ;
#363 = FACE_OUTER_BOUND ( 'NONE', #1822, .T. ) ;
#364 = FACE_OUTER_BOUND ( 'NONE', #13195, .T. ) ;
#365 = ORIENTED_EDGE ( 'NONE', *, *, #11993, .F. ) ;
#366 = CARTESIAN_POINT ( 'NONE',  ( -3.642744778375347270, -3.605832648298818111, -44.10000000002499121 ) ) ;
#367 = ORIENTED_EDGE ( 'NONE', *, *, #29552, .F. ) ;
#368 = VERTEX_POINT ( 'NONE', #1564 ) ;
#369 = ORIENTED_EDGE ( 'NONE', *, *, #12352, .F. ) ;
#370 = CARTESIAN_POINT ( 'NONE',  ( 6.438687372225744276, -8.560122214837054599, -36.64192442626541890 ) ) ;
#371 = ADVANCED_FACE ( 'NONE', ( #30354 ), #16338, .F. ) ;
#372 = DIRECTION ( 'NONE',  ( 0.000000000000000000, 0.000000000000000000, -1.000000000000000000 ) ) ;
#373 = FACE_OUTER_BOUND ( 'NONE', #7279, .T. ) ;
#374 = ORIENTED_EDGE ( 'NONE', *, *, #19213, .T. ) ;
#375 = PLANE ( 'NONE',  #27480 ) ;
#376 = LINE ( 'NONE', #19562, #18555 ) ;
#377 = CARTESIAN_POINT ( 'NONE',  ( -17.39952085737849075, -31.99978942475004118, -27.11779176627238641 ) ) ;
#378 = CARTESIAN_POINT ( 'NONE',  ( 10.69999999996367102, -29.15111427914373721, -26.30567555911243360 ) ) ;
#379 = ORIENTED_EDGE ( 'NONE', *, *, #13979, .T. ) ;
#380 = EDGE_CURVE ( 'NONE', #18294, #17040, #28347, .T. ) ;
#381 = AXIS2_PLACEMENT_3D ( 'NONE', #29649, #27284, #22722 ) ;
#382 = CARTESIAN_POINT ( 'NONE',  ( -4.278952157217899455, -0.8066629416743122949, -15.59949426530000238 ) ) ;
#383 = LINE ( 'NONE', #6989, #23905 ) ;
#384 = AXIS2_PLACEMENT_3D ( 'NONE', #23871, #9212, #21346 ) ;
#385 = DIRECTION ( 'NONE',  ( 0.000000000000000000, 0.000000000000000000, 1.000000000000000000 ) ) ;
#386 = CARTESIAN_POINT ( 'NONE',  ( -12.34929264641464464, -28.75102117903383458, -33.16229187319683547 ) ) ;
#387 = CARTESIAN_POINT ( 'NONE',  ( 7.105427357599999217E-15, 3.552713678799999608E-15, 143.6055512749999821 ) ) ;
#388 = LINE ( 'NONE', #26960, #26358 ) ;
#389 = ADVANCED_FACE ( 'NONE', ( #25945 ), #10756, .T. ) ;
#390 = CARTESIAN_POINT ( 'NONE',  ( 10.35667741062603397, -26.55163333981976592, 190.0000000000000000 ) ) ;
#391 = CARTESIAN_POINT ( 'NONE',  ( -10.69999999999999929, -25.99080750769999781, -31.25597987799999444 ) ) ;
#392 = CARTESIAN_POINT ( 'NONE',  ( 25.84472112319999937, 9.051226241580000220, 230.0000000000000000 ) ) ;
#393 = DIRECTION ( 'NONE',  ( -1.000000000000000000, 0.000000000000000000, 0.000000000000000000 ) ) ;
#394 = ORIENTED_EDGE ( 'NONE', *, *, #19312, .F. ) ;
#395 = CARTESIAN_POINT ( 'NONE',  ( -3.985743628842677300, -2.180176701716181942, -52.94982952342499516 ) ) ;
#396 = CARTESIAN_POINT ( 'NONE',  ( -12.32161713220065735, -24.97215432380749434, -23.79754533132837935 ) ) ;
#397 = AXIS2_PLACEMENT_3D ( 'NONE', #28615, #21537, #4694 ) ;
#398 = CARTESIAN_POINT ( 'NONE',  ( 1.060425485998340633, -4.855416528021975431, -68.10000000002500542 ) ) ;
#399 = DIRECTION ( 'NONE',  ( 0.000000000000000000, 0.000000000000000000, 1.000000000000000000 ) ) ;
#400 = ORIENTED_EDGE ( 'NONE', *, *, #20390, .F. ) ;
#401 = VECTOR ( 'NONE', #6112, 1000.000000000000000 ) ;
#402 = EDGE_CURVE ( 'NONE', #3946, #1905, #1953, .T. ) ;
#403 = CARTESIAN_POINT ( 'NONE',  ( 0.5564057544863512117, 3.564787113782302619, -88.52261276243972077 ) ) ;
#404 = SURFACE_SIDE_STYLE ('',( #26510 ) ) ;
#405 = CIRCLE ( 'NONE', #17950, 27.23548387080000310 ) ;
#406 = ORIENTED_EDGE ( 'NONE', *, *, #23149, .F. ) ;
#407 = FACE_OUTER_BOUND ( 'NONE', #9123, .T. ) ;
#408 = CARTESIAN_POINT ( 'NONE',  ( -0.8929276208064895748, -4.785132802852544387, -68.65745670422501234 ) ) ;
#409 = VERTEX_POINT ( 'NONE', #30514 ) ;
#410 = CARTESIAN_POINT ( 'NONE',  ( 2.193772516446764076, 5.694542648089183423, -26.09462237480000724 ) ) ;
#411 = CARTESIAN_POINT ( 'NONE',  ( 17.16657240420000008, -9.000000000000001776, -0.8000000000000020428 ) ) ;
#412 = EDGE_CURVE ( 'NONE', #27661, #8534, #216, .T. ) ;
#413 = CARTESIAN_POINT ( 'NONE',  ( -4.543473910928012671, 0.02303893552233621245, -62.57122063472500884 ) ) ;
#414 = CARTESIAN_POINT ( 'NONE',  ( 17.16657240490000191, 11.00000000029999825, -0.6999999999999992895 ) ) ;
#415 = CARTESIAN_POINT ( 'NONE',  ( -23.47637529058820860, -14.89020704899713365, 4.098700198000015504 ) ) ;
#416 = B_SPLINE_SURFACE_WITH_KNOTS ( 'NONE', 5, 1, ( 
 ( #8599, #18199 ),
 ( #6254, #14591 ),
 ( #24030, #21979 ),
 ( #14278, #7033 ),
 ( #4834, #16622 ),
 ( #17088, #24179 ),
 ( #30954, #26082 ),
 ( #19146, #23884 ),
 ( #18832, #2323 ),
 ( #2471, #16469 ),
 ( #21669, #26392 ),
 ( #16775, #28434 ),
 ( #9549, #14431 ),
 ( #2781, #4521 ),
 ( #14119, #119 ) ),
 .UNSPECIFIED., .F., .F., .F.,
 ( 6, 3, 3, 3, 6 ),
 ( 2, 2 ),
 ( 0.000000000000000000, 0.5239049113340000785, 1.047809822670000113, 1.571714733999999947, 1.746349704450000040 ),
 ( -0.7000000000009999335, 2.557518061549999935E-06 ),
 .UNSPECIFIED. ) ;
#417 = CARTESIAN_POINT ( 'NONE',  ( -19.80535397421925481, 19.50875616500616871, 0.9999999989999952543 ) ) ;
#418 = VECTOR ( 'NONE', #18881, 1000.000000000000000 ) ;
#419 = CARTESIAN_POINT ( 'NONE',  ( 8.700000000293144353, -9.427296937348389250, -35.64651715365807405 ) ) ;
#420 = AXIS2_PLACEMENT_3D ( 'NONE', #11851, #7126, #19088 ) ;
#421 = EDGE_CURVE ( 'NONE', #12111, #14873, #20589, .T. ) ;
#422 = CARTESIAN_POINT ( 'NONE',  ( -27.92857142909999979, 3.420150602519999655E-15, 92.06031501479999690 ) ) ;
#423 = ORIENTED_EDGE ( 'NONE', *, *, #232, .T. ) ;
#424 = CARTESIAN_POINT ( 'NONE',  ( 3.370970677400644266, 1.161062029669245321, 227.6835602974635719 ) ) ;
#425 = DIRECTION ( 'NONE',  ( -1.000000000000000000, 0.000000000000000000, 0.000000000000000000 ) ) ;
#426 = CARTESIAN_POINT ( 'NONE',  ( -7.523368333400000552, -9.723541495030000092, 232.6627643349999914 ) ) ;
#427 = CIRCLE ( 'NONE', #27022, 27.23548387080000310 ) ;
#428 = DIRECTION ( 'NONE',  ( 0.3633921898465272138, -0.9316362575375356503, 0.000000000000000000 ) ) ;
#429 = CARTESIAN_POINT ( 'NONE',  ( -6.304462755850305911, -10.33059293845434645, 232.0000000000046043 ) ) ;
#430 = CARTESIAN_POINT ( 'NONE',  ( -6.000000000000000000, -29.96004123392021157, -79.78289277550334191 ) ) ;
#431 = CARTESIAN_POINT ( 'NONE',  ( 2.919161196683367709, -2.910013007151718956, -0.6999999999999992895 ) ) ;
#432 = AXIS2_PLACEMENT_3D ( 'NONE', #11352, #25679, #6931 ) ;
#433 = B_SPLINE_CURVE_WITH_KNOTS ( 'NONE', 5,
 ( #4051, #25135, #25459, #5930, #17879, #25619 ),
 .UNSPECIFIED., .F., .F.,
 ( 6, 6 ),
 ( -7.000000000120000010, -4.999999893120000038 ),
 .UNSPECIFIED. ) ;
#434 = CARTESIAN_POINT ( 'NONE',  ( -28.35945636591989683, -7.983396444576476902, 0.7595836940000044724 ) ) ;
#435 = LINE ( 'NONE', #22127, #18791 ) ;
#436 = CARTESIAN_POINT ( 'NONE',  ( -7.999999999681902452, -14.92844969907143771, -33.25053330396754347 ) ) ;
#437 = EDGE_CURVE ( 'NONE', #12797, #28640, #22954, .T. ) ;
#438 = MANIFOLD_SOLID_BREP ( 'Stock-MAS-156-1', #10548 ) ;
#439 = CARTESIAN_POINT ( 'NONE',  ( -24.33346004068414459, -12.81155130651161045, 5.286751411345756324 ) ) ;
#440 = CARTESIAN_POINT ( 'NONE',  ( 7.665314379936610578, -115.2210683807244038, 21.73067038611315382 ) ) ;
#441 = ORIENTED_EDGE ( 'NONE', *, *, #29887, .F. ) ;
#442 = VECTOR ( 'NONE', #12389, 1000.000000000000000 ) ;
#443 = CARTESIAN_POINT ( 'NONE',  ( 19.80526555962148549, 19.50877392102342256, 1.000000000000000888 ) ) ;
#444 = CARTESIAN_POINT ( 'NONE',  ( -24.26052213770000066, -13.57583965319999919, 223.9574921340000060 ) ) ;
#445 = DIRECTION ( 'NONE',  ( -3.924189347185962345E-12, 0.4082287037029531107, 0.9128796883888953273 ) ) ;
#446 = EDGE_CURVE ( 'NONE', #1677, #8641, #13828, .T. ) ;
#447 = CARTESIAN_POINT ( 'NONE',  ( 4.569612387855602087, -0.08076758077263379576, -58.09793411332499602 ) ) ;
#448 = ORIENTED_EDGE ( 'NONE', *, *, #167, .T. ) ;
#449 = ORIENTED_EDGE ( 'NONE', *, *, #3492, .F. ) ;
#451 = CARTESIAN_POINT ( 'NONE',  ( 18.13191322229999969, 10.47263190749999495, -1.399999999599998990 ) ) ;
#450 = AXIS2_PLACEMENT_3D ( 'NONE', #30643, #26222, #11742 ) ;
#452 = ORIENTED_EDGE ( 'NONE', *, *, #845, .F. ) ;
#453 = VERTEX_POINT ( 'NONE', #9877 ) ;
#454 = SURFACE_STYLE_FILL_AREA ( #9717 ) ;
#455 = CARTESIAN_POINT ( 'NONE',  ( -16.66884554142874464, -10.09718743908464234, -0.6999999999999783062 ) ) ;
#456 = CARTESIAN_POINT ( 'NONE',  ( -24.82465127917437542, -14.00098045660550916, 223.9261769685532784 ) ) ;
#457 = CARTESIAN_POINT ( 'NONE',  ( 10.59650700230000098, -5.774382186429999564, 231.9999991140000191 ) ) ;
#458 = EDGE_CURVE ( 'NONE', #11841, #9298, #9464, .T. ) ;
#459 = CARTESIAN_POINT ( 'NONE',  ( 9.799999999872998302, 8.682826176889994585, 14.90608581632256424 ) ) ;
#460 = CARTESIAN_POINT ( 'NONE',  ( 3.619519562537647062, 2.908736503316577515, -7.854586408000003850 ) ) ;
#461 = PLANE ( 'NONE',  #25084 ) ;
#462 = ORIENTED_EDGE ( 'NONE', *, *, #21169, .F. ) ;
#463 = CARTESIAN_POINT ( 'NONE',  ( 2.806119477842475618, -3.711775362531495759, -44.10000000002499121 ) ) ;
#464 = DIRECTION ( 'NONE',  ( -1.667070188605962886E-12, 0.4082287037029531107, 0.9128796883888953273 ) ) ;
#465 = VECTOR ( 'NONE', #12974, 1000.000000000000000 ) ;
#466 = ADVANCED_FACE ( 'NONE', ( #21379 ), #11165, .F. ) ;
#467 = CARTESIAN_POINT ( 'NONE',  ( 4.354753084053718304, 0.1085053810021633369, -21.17661200059999871 ) ) ;
#468 = CARTESIAN_POINT ( 'NONE',  ( 12.63351996701598878, 21.70000000000023377, -55.99837678453474865 ) ) ;
#469 = DIRECTION ( 'NONE',  ( 2.764840495839172918E-12, 0.9128796883888953273, -0.4082287037029531107 ) ) ;
#470 = CARTESIAN_POINT ( 'NONE',  ( -3.907985046680000082E-14, -26.80000000000000071, 6.099999999630000502 ) ) ;
#471 = DIRECTION ( 'NONE',  ( 1.000000000000000000, 0.000000000000000000, 0.000000000000000000 ) ) ;
#472 = CARTESIAN_POINT ( 'NONE',  ( -4.848570193085772750, 0.4842359979205512754, -47.22737393802500350 ) ) ;
#473 = CARTESIAN_POINT ( 'NONE',  ( -27.50000000000000000, 3.367667473009999970E-15, 36.39444872359999295 ) ) ;
#474 = CARTESIAN_POINT ( 'NONE',  ( 0.6479069288420113981, -26.79235980062891542, 224.0901877813894032 ) ) ;
#475 = CARTESIAN_POINT ( 'NONE',  ( 8.699999999949442397, -116.5561065468441626, 18.74526241745003574 ) ) ;
#476 = AXIS2_PLACEMENT_3D ( 'NONE', #10659, #13016, #25296 ) ;
#477 = CARTESIAN_POINT ( 'NONE',  ( -26.13021838950000131, 9.136631768579999147, 229.9751247030000059 ) ) ;
#478 = CARTESIAN_POINT ( 'NONE',  ( 8.999999999770000869, 21.34659487689999935, -44.03581336912210276 ) ) ;
#479 = ORIENTED_EDGE ( 'NONE', *, *, #10437, .F. ) ;
#480 = CARTESIAN_POINT ( 'NONE',  ( 3.166603938121563377, 4.517215167231739770, -30.21106724380000941 ) ) ;
#481 = ORIENTED_EDGE ( 'NONE', *, *, #2473, .T. ) ;
#482 = CARTESIAN_POINT ( 'NONE',  ( -10.00000000039044856, -37.77593666279831552, -25.96758248505484801 ) ) ;
#483 = CARTESIAN_POINT ( 'NONE',  ( 2.137930486642451555, 6.059703978454344941, -45.49079303332499791 ) ) ;
#484 = ORIENTED_EDGE ( 'NONE', *, *, #3647, .F. ) ;
#485 = ORIENTED_EDGE ( 'NONE', *, *, #26372, .T. ) ;
#486 = AXIS2_PLACEMENT_3D ( 'NONE', #21935, #385, #9970 ) ;
#487 = ORIENTED_EDGE ( 'NONE', *, *, #22114, .T. ) ;
#488 = CARTESIAN_POINT ( 'NONE',  ( 18.64708650441101767, 19.99999271436163539, 230.6104614892431073 ) ) ;
#489 = ORIENTED_EDGE ( 'NONE', *, *, #26242, .T. ) ;
#490 = CARTESIAN_POINT ( 'NONE',  ( -16.83342759575507586, 10.99999999997565503, -0.6999999999999784173 ) ) ;
#491 = FACE_OUTER_BOUND ( 'NONE', #749, .T. ) ;
#492 = DIRECTION ( 'NONE',  ( 6.325958275728752229E-12, 0.3568421334038983650, -0.9341647027306021478 ) ) ;
#493 = CARTESIAN_POINT ( 'NONE',  ( 0.5558345775367062869, 4.217921792658845703, -35.70000000000000284 ) ) ;
#494 = AXIS2_PLACEMENT_3D ( 'NONE', #24933, #10926, #20518 ) ;
#495 = CARTESIAN_POINT ( 'NONE',  ( -20.30396347049999761, 20.00000000670000233, 227.0000000000000000 ) ) ;
#496 = EDGE_CURVE ( 'NONE', #28185, #6097, #18826, .T. ) ;
#497 = CARTESIAN_POINT ( 'NONE',  ( -3.505585908281066754, -1.519096937744677245, -0.6999999999999995115 ) ) ;
#498 = DIRECTION ( 'NONE',  ( -0.7071067811865475727, -0.7071067811865475727, 0.000000000000000000 ) ) ;
#499 = CYLINDRICAL_SURFACE ( 'NONE', #6959, 3.000000000000003997 ) ;
#500 = CARTESIAN_POINT ( 'NONE',  ( 0.5074138422395748638, -6.503547975687064664, -9.393384211799999051 ) ) ;
#501 = CARTESIAN_POINT ( 'NONE',  ( -4.702124758411583727, -0.9170245833456597273, -30.15902066320000685 ) ) ;
#502 = CARTESIAN_POINT ( 'NONE',  ( 1.630907767950000142, 5.558498091389999729, 226.6412452697800006 ) ) ;
#503 = EDGE_CURVE ( 'NONE', #26528, #20466, #26706, .T. ) ;
#504 = ADVANCED_FACE ( 'NONE', ( #24355, #2797 ), #16952, .T. ) ;
#505 = CARTESIAN_POINT ( 'NONE',  ( 10.14902473058287491, -26.01926976374856082, 187.9396849849999853 ) ) ;
#506 = CARTESIAN_POINT ( 'NONE',  ( 9.229093439197374238, -15.48814874288954613, -74.51555467526300447 ) ) ;
#507 = CARTESIAN_POINT ( 'NONE',  ( 5.601646981916513113, -31.11278470850464473, -80.20245708799704687 ) ) ;
#508 = CARTESIAN_POINT ( 'NONE',  ( 1.015231355570000105, -28.48218680760000154, 225.5064715119999903 ) ) ;
#509 = CARTESIAN_POINT ( 'NONE',  ( 1.213582369797461258, 4.521795443253901148, -2.053410702900000828 ) ) ;
#510 = CARTESIAN_POINT ( 'NONE',  ( 0.5057536231481192246, -27.79562098839016571, 6.099998581000020792 ) ) ;
#511 = CARTESIAN_POINT ( 'NONE',  ( -23.81866173682177390, -14.33570044646243247, 3.899998581000013509 ) ) ;
#512 = CARTESIAN_POINT ( 'NONE',  ( 16.27478637877570833, 11.65988689034672809, -4.336808689942018722E-16 ) ) ;
#513 = ORIENTED_EDGE ( 'NONE', *, *, #26739, .T. ) ;
#514 = DIRECTION ( 'NONE',  ( -0.7071067811834159667, 0.6355433650310505778, -0.3099752105724544737 ) ) ;
#515 = CARTESIAN_POINT ( 'NONE',  ( -10.35667741062608371, -26.55163333981974816, 190.0000000000000000 ) ) ;
#516 = AXIS2_PLACEMENT_3D ( 'NONE', #27552, #8502, #8343 ) ;
#517 = ORIENTED_EDGE ( 'NONE', *, *, #14756, .F. ) ;
#518 = B_SPLINE_CURVE_WITH_KNOTS ( 'NONE', 3,
 ( #27708, #6155, #1766, #15753, #13874, #1917, #25838, #4277, #13558, #25368, #23481, #21112, #6786, #30708, #3806, #28337, #13394, #9135, #23165, #23005 ),
 .UNSPECIFIED., .F., .F.,
 ( 4, 1, 1, 1, 2, 2, 2, 1, 1, 1, 2, 2, 4 ),
 ( 0.000000000000000000, 0.1249999999999770739, 0.1874999999999654166, 0.2187499999999614197, 0.2343749999999610867, 0.2499999999999607536, 0.4999999999999691358, 0.6249999999999732436, 0.6874999999999761302, 0.7187499999999775735, 0.7343749999999796829, 0.7499999999999819034, 1.000000000000000000 ),
 .UNSPECIFIED. ) ;
#519 = B_SPLINE_CURVE_WITH_KNOTS ( 'NONE', 5,
 ( #763, #19799, #26878, #10508, #7824, #14617, #22156, #5319, #27336, #14923, #24519, #22311, #2956, #20108, #29696 ),
 .UNSPECIFIED., .F., .F.,
 ( 6, 3, 3, 3, 6 ),
 ( 0.000000000000000000, 0.3000000000005726419, 0.6000000000000000888, 0.9000000000028631764, 1.000000000000000000 ),
 .UNSPECIFIED. ) ;
#520 = DIRECTION ( 'NONE',  ( 1.000000000000000000, -0.000000000000000000, -2.257150022439999944E-12 ) ) ;
#521 = DIRECTION ( 'NONE',  ( 1.000000000000000000, 0.000000000000000000, 0.000000000000000000 ) ) ;
#522 = ORIENTED_EDGE ( 'NONE', *, *, #12199, .T. ) ;
#523 = CARTESIAN_POINT ( 'NONE',  ( -2.744417411265728912, -4.298957096598221561, -44.10000000002499121 ) ) ;
#524 = ORIENTED_EDGE ( 'NONE', *, *, #26123, .T. ) ;
#525 = ORIENTED_EDGE ( 'NONE', *, *, #2715, .F. ) ;
#526 = FILL_AREA_STYLE_COLOUR ( '', #18851 ) ;
#527 = SHAPE_REPRESENTATION ( 'Rivet', ( #17722 ), #2272 ) ;
#528 = VERTEX_POINT ( 'NONE', #14451 ) ;
#529 = FACE_OUTER_BOUND ( 'NONE', #18862, .T. ) ;
#530 = FACE_OUTER_BOUND ( 'NONE', #26990, .T. ) ;
#531 = CARTESIAN_POINT ( 'NONE',  ( -7.999999999670753148, -18.01685129643773564, -34.09892490238275542 ) ) ;
#532 = EDGE_CURVE ( 'NONE', #10448, #2003, #10192, .T. ) ;
#533 = ORIENTED_EDGE ( 'NONE', *, *, #12374, .F. ) ;
#534 = CARTESIAN_POINT ( 'NONE',  ( -24.78870452935070290, 12.58522324297991268, 5.507123707999994622 ) ) ;
#535 = FACE_BOUND ( 'NONE', #29200, .T. ) ;
#536 = CARTESIAN_POINT ( 'NONE',  ( -17.19097361925006595, -31.99975500943657281, -30.75789318072767742 ) ) ;
#537 = CARTESIAN_POINT ( 'NONE',  ( 10.69999999989999928, -25.00000000000000000, -7.274962170899998526 ) ) ;
#538 = ORIENTED_EDGE ( 'NONE', *, *, #20624, .T. ) ;
#539 = AXIS2_PLACEMENT_3D ( 'NONE', #23049, #13598, #18623 ) ;
#540 = MANIFOLD_SOLID_BREP ( 'PartBody', #13552 ) ;
#541 = CARTESIAN_POINT ( 'NONE',  ( 1.776356839399999804E-15, -5.329070518200000398E-15, 224.6412452697800290 ) ) ;
#542 = CARTESIAN_POINT ( 'NONE',  ( -2.820898088245517688, -4.403288343584588205, -17.70544088820000539 ) ) ;
#543 = CARTESIAN_POINT ( 'NONE',  ( -0.9721910944845530977, -28.48371442619422567, 224.4394323450521540 ) ) ;
#544 = APPLICATION_CONTEXT ( 'automotive_design' ) ;
#545 = CARTESIAN_POINT ( 'NONE',  ( -8.699999999716542476, -29.98791884354844939, -27.92359244214648228 ) ) ;
#546 = LINE ( 'NONE', #17194, #5634 ) ;
#547 = DIRECTION ( 'NONE',  ( 0.000000000000000000, 0.000000000000000000, -1.000000000000000000 ) ) ;
#548 = FACE_OUTER_BOUND ( 'NONE', #11882, .T. ) ;
#549 = CYLINDRICAL_SURFACE ( 'NONE', #29045, 20.00000000000000355 ) ;
#550 = DIRECTION ( 'NONE',  ( -1.000000000000000000, 5.063197467948052462E-16, -2.257212216284997029E-12 ) ) ;
#551 = CARTESIAN_POINT ( 'NONE',  ( 26.78508784419999955, 9.380747199480000020, 229.2930777859999978 ) ) ;
#552 = CARTESIAN_POINT ( 'NONE',  ( -10.87631678760000042, 14.78838196149999895, 230.6999999999999886 ) ) ;
#553 = VERTEX_POINT ( 'NONE', #15670 ) ;
#554 = CARTESIAN_POINT ( 'NONE',  ( 4.692739937114380311, 0.5303478879429834869, -55.01771407622499765 ) ) ;
#555 = CARTESIAN_POINT ( 'NONE',  ( -8.699999999672870743, -17.90468864316765973, -33.94136269864641520 ) ) ;
#556 = CARTESIAN_POINT ( 'NONE',  ( -26.39324905318550307, 9.701294701415816846, 8.000000000000007105 ) ) ;
#557 = CARTESIAN_POINT ( 'NONE',  ( -4.646218698937943259, 0.8004880362142797745, -68.10000000002497700 ) ) ;
#558 = ADVANCED_FACE ( 'NONE', ( #1056 ), #28917, .F. ) ;
#559 = ORIENTED_EDGE ( 'NONE', *, *, #5058, .T. ) ;
#560 = ADVANCED_FACE ( 'NONE', ( #602, #27628 ), #17709, .F. ) ;
#561 = CARTESIAN_POINT ( 'NONE',  ( 3.371793442757397230, -0.3929169320064240245, -94.29636648343951322 ) ) ;
#562 = ORIENTED_EDGE ( 'NONE', *, *, #8040, .F. ) ;
#563 = CARTESIAN_POINT ( 'NONE',  ( -10.99289321870000080, 19.99999999999999645, -1.692893218799999877 ) ) ;
#564 = DIRECTION ( 'NONE',  ( 1.000000000000000000, 0.000000000000000000, 0.000000000000000000 ) ) ;
#565 = VERTEX_POINT ( 'NONE', #8271 ) ;
#566 = CARTESIAN_POINT ( 'NONE',  ( 2.695668638436317543, -3.937035225248731951, -28.07042313650000409 ) ) ;
#567 = EDGE_CURVE ( 'NONE', #6895, #23236, #6073, .T. ) ;
#568 = DIRECTION ( 'NONE',  ( 1.000000000000000000, -1.224606353819999582E-16, 0.000000000000000000 ) ) ;
#569 = AXIS2_PLACEMENT_3D ( 'NONE', #17547, #27158, #15193 ) ;
#570 = CARTESIAN_POINT ( 'NONE',  ( -3.552713678799999608E-15, -26.80000000000000071, 0.000000000000000000 ) ) ;
#571 = CARTESIAN_POINT ( 'NONE',  ( -23.92402432625451070, -13.56054118811422882, 3.912293197164086855 ) ) ;
#572 =( LENGTH_UNIT ( ) NAMED_UNIT ( * ) SI_UNIT ( .MILLI., .METRE. ) );
#573 = CARTESIAN_POINT ( 'NONE',  ( -25.38146355678814814, 12.59839640969361696, 1.000000000000000888 ) ) ;
#574 = UNCERTAINTY_MEASURE_WITH_UNIT (LENGTH_MEASURE( 1.000000000000000082E-05 ), #26475, 'distance_accuracy_value', 'NONE');
#575 = CARTESIAN_POINT ( 'NONE',  ( -7.999999999684056284, -16.63651352361650382, -33.12749869627004529 ) ) ;
#576 = LINE ( 'NONE', #10157, #14540 ) ;
#577 = ORIENTED_EDGE ( 'NONE', *, *, #30008, .F. ) ;
#578 = CARTESIAN_POINT ( 'NONE',  ( 1.850829058368554492, -3.930924299794261056, -38.89973510835294235 ) ) ;
#579 = EDGE_CURVE ( 'NONE', #21911, #7653, #7180, .T. ) ;
#580 = CARTESIAN_POINT ( 'NONE',  ( 24.49999999589999788, -3.000285566359999846E-15, 90.00000000000000000 ) ) ;
#581 = CARTESIAN_POINT ( 'NONE',  ( -23.25311087912443853, -15.23597700045676895, 5.310552105000033052 ) ) ;
#582 = DIRECTION ( 'NONE',  ( 0.000000000000000000, 0.000000000000000000, 1.000000000000000000 ) ) ;
#583 = CARTESIAN_POINT ( 'NONE',  ( 26.93395386830000149, -3.298349104060000254E-15, 142.2432411360000231 ) ) ;
#584 = CARTESIAN_POINT ( 'NONE',  ( 2.423529086371690511, -21.74707102514618740, -30.21021974772776986 ) ) ;
#585 = CARTESIAN_POINT ( 'NONE',  ( 3.633532083198900864, -2.434228036718701027, -0.6999999999999992895 ) ) ;
#586 = CARTESIAN_POINT ( 'NONE',  ( -4.785279987089964493, -31.71089578132167119, 1.000000000000000888 ) ) ;
#587 = LINE ( 'NONE', #26687, #5223 ) ;
#588 = DIRECTION ( 'NONE',  ( 0.000000000000000000, 0.000000000000000000, 1.000000000000000000 ) ) ;
#589 = FACE_OUTER_BOUND ( 'NONE', #26163, .T. ) ;
#590 = COLOUR_RGB ( '', 0.09019608, 0.27058824, 0.51372549) ;
#591 = CARTESIAN_POINT ( 'NONE',  ( -22.29514036694591184, -14.89751301532327155, 93.21714158846667431 ) ) ;
#592 = CARTESIAN_POINT ( 'NONE',  ( 1.128437890537931976, -3.898078178863690901, -68.10000000002501963 ) ) ;
#593 = ORIENTED_EDGE ( 'NONE', *, *, #25979, .T. ) ;
#594 = CARTESIAN_POINT ( 'NONE',  ( 11.59065746419999954, -24.20066399999999973, -1.404983722799999057 ) ) ;
#595 = CARTESIAN_POINT ( 'NONE',  ( 24.19477113890000197, -13.69187437440000110, 226.0798554400000171 ) ) ;
#596 = CARTESIAN_POINT ( 'NONE',  ( -0.8249440165340218289, 4.504533947698903695, -60.65324387862499833 ) ) ;
#597 = ORIENTED_EDGE ( 'NONE', *, *, #20203, .T. ) ;
#598 = EDGE_CURVE ( 'NONE', #11580, #19721, #22614, .T. ) ;
#599 = ORIENTED_EDGE ( 'NONE', *, *, #18165, .T. ) ;
#600 = DIRECTION ( 'NONE',  ( -4.656612873080000265E-10, 2.255973186040000320E-12, 1.000000000000000000 ) ) ;
#601 = ORIENTED_EDGE ( 'NONE', *, *, #21982, .T. ) ;
#602 = FACE_BOUND ( 'NONE', #30223, .T. ) ;
#603 = CARTESIAN_POINT ( 'NONE',  ( -24.29138540600951046, 13.52003710149997140, 3.901342110999989288 ) ) ;
#604 = DIRECTION ( 'NONE',  ( 0.2815395311429191860, 0.9595496299847263710, 0.000000000000000000 ) ) ;
#605 = VECTOR ( 'NONE', #18518, 1000.000000000000000 ) ;
#606 = CARTESIAN_POINT ( 'NONE',  ( 11.05434102880000147, 5.380509146490000560, 232.6627648150000027 ) ) ;
#607 = DIRECTION ( 'NONE',  ( 1.224606353819999829E-16, 1.000000000000000000, 0.000000000000000000 ) ) ;
#608 = CARTESIAN_POINT ( 'NONE',  ( 0.3624384587677549341, -4.645391411234346180, -8.893384211800004380 ) ) ;
#609 = AXIS2_PLACEMENT_3D ( 'NONE', #4921, #21294, #28527 ) ;
#610 = CARTESIAN_POINT ( 'NONE',  ( 14.40197535836999876, -27.00000000000014566, -22.62649730800000114 ) ) ;
#611 = EDGE_LOOP ( 'NONE', ( #22896, #7545, #4645, #11032, #905, #16835, #7239, #10300 ) ) ;
#612 = CARTESIAN_POINT ( 'NONE',  ( 2.873326072151168642, -3.563018121669343063, -44.10000000002499831 ) ) ;
#613 = ADVANCED_FACE ( 'NONE', ( #29527 ), #24814, .T. ) ;
#614 = CARTESIAN_POINT ( 'NONE',  ( -7.861312627709999390, 2.450513428968473129, -42.01217025057427179 ) ) ;
#615 = ADVANCED_FACE ( 'NONE', ( #10188, #8422, #29835 ), #7814, .F. ) ;
#616 = CARTESIAN_POINT ( 'NONE',  ( 5.403695180783418373, -1.168003237233325553, -24.79036215650000585 ) ) ;
#617 = CARTESIAN_POINT ( 'NONE',  ( 8.349999999579441834, -116.5561065468438215, 18.74526241744838373 ) ) ;
#618 = FACE_OUTER_BOUND ( 'NONE', #29092, .T. ) ;
#619 = EDGE_CURVE ( 'NONE', #11656, #7142, #9529, .T. ) ;
#620 =( LENGTH_UNIT ( ) NAMED_UNIT ( * ) SI_UNIT ( .MILLI., .METRE. ) );
#621 = DIRECTION ( 'NONE',  ( -1.000000000000000000, -0.000000000000000000, -6.771000000000000128E-12 ) ) ;
#622 = CARTESIAN_POINT ( 'NONE',  ( -0.5163256777700186984, 4.538631023554793309, -47.86410749632499773 ) ) ;
#623 = EDGE_CURVE ( 'NONE', #12633, #11464, #6060, .T. ) ;
#624 = CARTESIAN_POINT ( 'NONE',  ( -7.999999999945726081, -112.1477080532550445, 5.846459785100098117 ) ) ;
#625 = CARTESIAN_POINT ( 'NONE',  ( -26.84464183999999776, 3.287411896330000120E-15, 142.5624961750000068 ) ) ;
#626 = FACE_BOUND ( 'NONE', #15131, .T. ) ;
#627 = CARTESIAN_POINT ( 'NONE',  ( -18.03440174900000059, 20.21871556809999859, 229.9751246760000072 ) ) ;
#628 = CARTESIAN_POINT ( 'NONE',  ( 8.999999999770000869, 20.56980753179999510, -43.48101130890499633 ) ) ;
#629 = ORIENTED_EDGE ( 'NONE', *, *, #30807, .T. ) ;
#630 = B_SPLINE_CURVE_WITH_KNOTS ( 'NONE', 1,
 ( #19801, #8283 ),
 .UNSPECIFIED., .F., .F.,
 ( 2, 2 ),
 ( -2.557291473029999731E-06, 0.7000000000009999335 ),
 .UNSPECIFIED. ) ;
#631 = B_SPLINE_CURVE_WITH_KNOTS ( 'NONE', 5,
 ( #31112, #6871, #7037, #18836, #26396, #16473, #11758, #23732, #2168 ),
 .UNSPECIFIED., .F., .F.,
 ( 6, 3, 6 ),
 ( 8.011061266649999624, 8.811732102769999742, 9.612402938880000747 ),
 .UNSPECIFIED. ) ;
#632 = CARTESIAN_POINT ( 'NONE',  ( -2.539202180960155264, -4.449342792696782567, -31.61392233980000199 ) ) ;
#633 = EDGE_CURVE ( 'NONE', #28095, #17368, #24462, .T. ) ;
#634 = ORIENTED_EDGE ( 'NONE', *, *, #28989, .F. ) ;
#635 = CARTESIAN_POINT ( 'NONE',  ( 9.999999999971985076, -26.60730091853679369, -31.40000000000158664 ) ) ;
#636 = CARTESIAN_POINT ( 'NONE',  ( -2.393684743089937061, 3.904820337558664978, -45.05531229042499319 ) ) ;
#637 = ORIENTED_EDGE ( 'NONE', *, *, #4986, .T. ) ;
#638 = ORIENTED_EDGE ( 'NONE', *, *, #24063, .F. ) ;
#639 = PRODUCT_CONTEXT ( 'NONE', #19223, 'mechanical' ) ;
#640 = ORIENTED_EDGE ( 'NONE', *, *, #8309, .F. ) ;
#641 = ORIENTED_EDGE ( 'NONE', *, *, #7365, .F. ) ;
#642 = DIRECTION ( 'NONE',  ( -1.181300906760215537E-13, 0.9986295347541825906, 0.05233595625040957794 ) ) ;
#643 = EDGE_CURVE ( 'NONE', #22250, #22666, #3841, .T. ) ;
#644 = LINE ( 'NONE', #10231, #6918 ) ;
#645 = CARTESIAN_POINT ( 'NONE',  ( -6.585786437629999490, -15.73107082825028336, -76.73232662853232000 ) ) ;
#646 = CARTESIAN_POINT ( 'NONE',  ( -12.39443769393950845, -30.57364707460137510, -24.68998539662501557 ) ) ;
#647 = CARTESIAN_POINT ( 'NONE',  ( -3.745818880286417851, 2.145659048795447443, -0.6999999999999994005 ) ) ;
#648 = DIRECTION ( 'NONE',  ( 1.000000000000000000, 0.000000000000000000, 0.000000000000000000 ) ) ;
#649 = CIRCLE ( 'NONE', #8157, 1.472846691535505848 ) ;
#650 = DIRECTION ( 'NONE',  ( 0.000000000000000000, -1.000000000000000000, 2.257145581549999994E-12 ) ) ;
#651 = CARTESIAN_POINT ( 'NONE',  ( -0.8919388126321509125, 6.008950160842678301, -11.46772091660000470 ) ) ;
#652 = CARTESIAN_POINT ( 'NONE',  ( 6.379535387291454640, -1.442012952481606991, -32.78377053309999667 ) ) ;
#653 = CARTESIAN_POINT ( 'NONE',  ( 3.686970300939999667, -0.1862064327014488485, -68.94610314789109395 ) ) ;
#654 = CARTESIAN_POINT ( 'NONE',  ( 24.92013865993870425, -13.82966158318416738, 6.099998581000020792 ) ) ;
#655 = CARTESIAN_POINT ( 'NONE',  ( 24.66346747934004568, 14.28208995973567141, 6.002748562000004284 ) ) ;
#656 =( NAMED_UNIT ( * ) PLANE_ANGLE_UNIT ( ) SI_UNIT ( $, .RADIAN. ) );
#657 = CARTESIAN_POINT ( 'NONE',  ( 8.000000000883357387, -67.40749995174687115, -17.04319545456667484 ) ) ;
#658 = CARTESIAN_POINT ( 'NONE',  ( -2.308365619037855421, -4.044857084274065429, -30.67642233980000199 ) ) ;
#659 = CARTESIAN_POINT ( 'NONE',  ( 9.999999999969999109, -24.00000000000000000, -28.40000000000000213 ) ) ;
#660 = CARTESIAN_POINT ( 'NONE',  ( 24.34663841809999951, -12.78636765230000094, 5.000000000000000000 ) ) ;
#661 = LINE ( 'NONE', #3612, #30395 ) ;
#662 = VERTEX_POINT ( 'NONE', #3400 ) ;
#663 = DIRECTION ( 'NONE',  ( 4.901511854548699870E-24, -1.000000000000000000, 2.257145581550420047E-12 ) ) ;
#664 = CARTESIAN_POINT ( 'NONE',  ( -12.44217317844253756, -31.99999999999999289, -29.95172824868416583 ) ) ;
#665 = EDGE_LOOP ( 'NONE', ( #12496, #18069, #19743, #15909 ) ) ;
#666 = CARTESIAN_POINT ( 'NONE',  ( -14.89999999969999855, -27.00000000000000000, -28.40000000020000215 ) ) ;
#667 = DIRECTION ( 'NONE',  ( 0.3090169943750400994, -0.9510565162951234441, 0.000000000000000000 ) ) ;
#668 = EDGE_CURVE ( 'NONE', #10071, #13694, #28108, .T. ) ;
#669 = VERTEX_POINT ( 'NONE', #6546 ) ;
#670 = CARTESIAN_POINT ( 'NONE',  ( 9.947945353310727157, -14.47719179179285476, -74.14759643693901126 ) ) ;
#671 = ORIENTED_EDGE ( 'NONE', *, *, #17096, .T. ) ;
#672 = ORIENTED_EDGE ( 'NONE', *, *, #1632, .F. ) ;
#673 = EDGE_CURVE ( 'NONE', #7295, #15790, #18185, .T. ) ;
#674 = ORIENTED_EDGE ( 'NONE', *, *, #8406, .F. ) ;
#675 = CARTESIAN_POINT ( 'NONE',  ( 27.50000000000000000, -1.044349611129999949E-13, 0.000000000000000000 ) ) ;
#676 = ADVANCED_FACE ( 'NONE', ( #8584 ), #13788, .T. ) ;
#677 = EDGE_CURVE ( 'NONE', #10071, #14251, #16593, .T. ) ;
#678 = CARTESIAN_POINT ( 'NONE',  ( -16.06988921231594603, 11.79183908526949054, -0.6999999999999784173 ) ) ;
#679 = DIRECTION ( 'NONE',  ( 0.9316362575375356503, 0.3633921898465274913, 0.000000000000000000 ) ) ;
#680 = ORIENTED_EDGE ( 'NONE', *, *, #23014, .F. ) ;
#681 = CARTESIAN_POINT ( 'NONE',  ( -24.83827471527357744, 12.48687850854618198, 4.999998581000003384 ) ) ;
#682 = DIRECTION ( 'NONE',  ( 0.9316362575375356503, 0.3633921898465274913, 0.000000000000000000 ) ) ;
#683 = CARTESIAN_POINT ( 'NONE',  ( -17.12355120911804462, -32.00000000000027001, -31.01886516981582886 ) ) ;
#684 = CARTESIAN_POINT ( 'NONE',  ( 0.000000000000000000, 0.000000000000000000, 92.06031501460000754 ) ) ;
#685 = CIRCLE ( 'NONE', #15728, 3.200000000000000178 ) ;
#686 = ORIENTED_EDGE ( 'NONE', *, *, #13583, .T. ) ;
#687 = TOROIDAL_SURFACE ( 'NONE', #1239, 12.03781779390000040, 5.000000000000000000 ) ;
#688 = MANIFOLD_SOLID_BREP ( 'Stock-MAS-156-1', #17562 ) ;
#689 = CARTESIAN_POINT ( 'NONE',  ( 16.20123158609999692, -8.472631907500000281, -1.399999999599998990 ) ) ;
#690 = CARTESIAN_POINT ( 'NONE',  ( -5.151963982244392781, -3.152247574024123811, -21.30799200640000279 ) ) ;
#691 = TOROIDAL_SURFACE ( 'NONE', #8176, 29.80000000000000071, 3.000000000000000000 ) ;
#692 = CARTESIAN_POINT ( 'NONE',  ( -0.8418772534729759283, -28.48787735128006560, 224.2649303555695326 ) ) ;
#693 = B_SPLINE_CURVE_WITH_KNOTS ( 'NONE', 1,
 ( #19992, #29587 ),
 .UNSPECIFIED., .F., .F.,
 ( 2, 2 ),
 ( -3.500000000000000000, -1.499999893000000029 ),
 .UNSPECIFIED. ) ;
#694 = CARTESIAN_POINT ( 'NONE',  ( -0.2897532859572976571, -27.49881094958763939, 6.071390044457605661 ) ) ;
#695 = CARTESIAN_POINT ( 'NONE',  ( 23.26185891380331583, -14.66761890373620503, 225.2867514118632357 ) ) ;
#696 = DIRECTION ( 'NONE',  ( -0.8660254037843290176, 0.5000000000001900702, 0.000000000000000000 ) ) ;
#697 = CARTESIAN_POINT ( 'NONE',  ( 8.999999999770000869, 20.70710678120000381, -44.39289321881399530 ) ) ;
#698 = CARTESIAN_POINT ( 'NONE',  ( -3.415131430766694010, -0.8926240818011570433, -0.6999999999999785283 ) ) ;
#699 = CARTESIAN_POINT ( 'NONE',  ( 18.26639035964474900, 11.02001161816309072, -0.6999999989999727834 ) ) ;
#700 = FACE_OUTER_BOUND ( 'NONE', #10031, .T. ) ;
#701 = ORIENTED_EDGE ( 'NONE', *, *, #14521, .F. ) ;
#702 = CARTESIAN_POINT ( 'NONE',  ( 3.599561039400463347, 4.779710538180673041, -54.62619010302499589 ) ) ;
#703 = DIRECTION ( 'NONE',  ( -1.000000000000000000, 0.000000000000000000, 0.000000000000000000 ) ) ;
#704 = CARTESIAN_POINT ( 'NONE',  ( -18.48840142452550594, 20.72769736509012262, 0.7069223289999926330 ) ) ;
#705 = CARTESIAN_POINT ( 'NONE',  ( -4.145494824737311568, 0.03818007883295551630, -68.10000000002501963 ) ) ;
#706 = AXIS2_PLACEMENT_3D ( 'NONE', #14476, #7537, #17129 ) ;
#707 = ORIENTED_EDGE ( 'NONE', *, *, #25056, .T. ) ;
#708 = CIRCLE ( 'NONE', #23295, 3.000000000000001332 ) ;
#709 = CARTESIAN_POINT ( 'NONE',  ( 23.81569860410000317, -13.75000000000000000, 6.099999999630000502 ) ) ;
#710 = VECTOR ( 'NONE', #27940, 1000.000000000000000 ) ;
#711 = ORIENTED_EDGE ( 'NONE', *, *, #9275, .F. ) ;
#712 = FACE_OUTER_BOUND ( 'NONE', #24045, .T. ) ;
#713 = EDGE_CURVE ( 'NONE', #20972, #5752, #15843, .T. ) ;
#714 = CARTESIAN_POINT ( 'NONE',  ( -8.000000000001699973, -117.5009442568067755, 14.55791348096084192 ) ) ;
#715 = ORIENTED_EDGE ( 'NONE', *, *, #21453, .F. ) ;
#716 = CARTESIAN_POINT ( 'NONE',  ( 1.415268835064556363, -5.780081730213937341, -64.22397119102500085 ) ) ;
#717 = LINE ( 'NONE', #17373, #10923 ) ;
#718 = CARTESIAN_POINT ( 'NONE',  ( -28.49528339128749366, -0.5184828350247461248, 0.7595836940000044724 ) ) ;
#719 = DIRECTION ( 'NONE',  ( 0.000000000000000000, -1.000000000000000000, 0.000000000000000000 ) ) ;
#720 = SURFACE_STYLE_USAGE ( .BOTH. , #26983 ) ;
#721 = CARTESIAN_POINT ( 'NONE',  ( -15.88645657644312337, 11.57790908595850965, -1.400000000000001910 ) ) ;
#722 = ORIENTED_EDGE ( 'NONE', *, *, #2189, .T. ) ;
#723 = CARTESIAN_POINT ( 'NONE',  ( 13.99999999979999821, 21.69999999929999390, -58.51619795559999915 ) ) ;
#724 = DIRECTION ( 'NONE',  ( 0.000000000000000000, -0.3420201433259318358, 0.9396926207858125046 ) ) ;
#725 = VERTEX_POINT ( 'NONE', #10962 ) ;
#726 = CARTESIAN_POINT ( 'NONE',  ( 3.221703195401058650, 1.419518900322475741, 227.6563758784883191 ) ) ;
#727 = ADVANCED_FACE ( 'NONE', ( #13470 ), #28257, .F. ) ;
#728 = DIRECTION ( 'NONE',  ( 0.000000000000000000, -2.256683728769999802E-12, -1.000000000000000000 ) ) ;
#729 = CIRCLE ( 'NONE', #20825, 27.50000000000000000 ) ;
#730 = CARTESIAN_POINT ( 'NONE',  ( 7.000000000276031642, -5.430118837459354530, -26.70804059584096635 ) ) ;
#731 = VECTOR ( 'NONE', #13088, 1000.000000000000114 ) ;
#732 = CARTESIAN_POINT ( 'NONE',  ( 28.49528339128749366, 0.5184828350247212558, 1.000000000000000888 ) ) ;
#733 = CARTESIAN_POINT ( 'NONE',  ( 26.80000000069999899, -3.281945028320000125E-15, 142.8898184869999852 ) ) ;
#734 = CARTESIAN_POINT ( 'NONE',  ( -5.851800771450323957, -26.15706768910720825, 208.9785434308453489 ) ) ;
#735 = CARTESIAN_POINT ( 'NONE',  ( 2.380832905875084116, -3.235963252731846485, -0.6999999999999991784 ) ) ;
#736 = CARTESIAN_POINT ( 'NONE',  ( -27.29371452669260734, -0.4966198192113812637, -0.6577119969999878357 ) ) ;
#737 = DIRECTION ( 'NONE',  ( 0.000000000000000000, -0.9624904629342537765, 0.2713155151490711514 ) ) ;
#738 = SURFACE_STYLE_USAGE ( .BOTH. , #10017 ) ;
#739 = CARTESIAN_POINT ( 'NONE',  ( -7.999999999681398855, -14.76903124974032977, -33.32608274503188994 ) ) ;
#740 = EDGE_CURVE ( 'NONE', #4043, #4187, #12790, .T. ) ;
#741 = CARTESIAN_POINT ( 'NONE',  ( -7.833397470852288436, -25.63019328476619307, 22.68384840406914549 ) ) ;
#742 = LINE ( 'NONE', #24800, #23892 ) ;
#743 = ORIENTED_EDGE ( 'NONE', *, *, #1777, .T. ) ;
#744 = CYLINDRICAL_SURFACE ( 'NONE', #29818, 3.000000000000002220 ) ;
#745 = CARTESIAN_POINT ( 'NONE',  ( 13.99999999979999821, 21.34999999960000139, -58.51619795559999915 ) ) ;
#746 = VECTOR ( 'NONE', #11944, 1000.000000000000114 ) ;
#747 = CARTESIAN_POINT ( 'NONE',  ( 1.008954696561116027, 5.412080152108726949, -64.22744533512499743 ) ) ;
#748 = EDGE_LOOP ( 'NONE', ( #15033, #19487, #856, #4347 ) ) ;
#749 = EDGE_LOOP ( 'NONE', ( #24404, #672, #17249, #8267 ) ) ;
#750 = CARTESIAN_POINT ( 'NONE',  ( -20.06986697712849121, -20.94709743681733727, 0.2686753820000109538 ) ) ;
#751 = EDGE_LOOP ( 'NONE', ( #2180, #29405, #19550, #13095 ) ) ;
#752 = EDGE_CURVE ( 'NONE', #26248, #11846, #25282, .T. ) ;
#753 = ORIENTED_EDGE ( 'NONE', *, *, #18876, .T. ) ;
#754 = CARTESIAN_POINT ( 'NONE',  ( -7.999999999888485647, -60.34578018689373380, -2.533826264313577603 ) ) ;
#755 = CARTESIAN_POINT ( 'NONE',  ( -23.69119896560000171, -20.94188573509999785, 229.0000000000000000 ) ) ;
#756 = CARTESIAN_POINT ( 'NONE',  ( -19.80535357367646654, 19.50875577052770993, 5.200000000000009948 ) ) ;
#757 = CARTESIAN_POINT ( 'NONE',  ( 8.700000000279958456, -18.28438020625039329, -36.42481760783426381 ) ) ;
#758 = DIRECTION ( 'NONE',  ( 1.224606353819999829E-16, 1.000000000000000000, 0.000000000000000000 ) ) ;
#759 = AXIS2_PLACEMENT_3D ( 'NONE', #15036, #8234, #5426 ) ;
#760 = CARTESIAN_POINT ( 'NONE',  ( 26.57440914490000239, -3.469982507400000582, -0.6999999999999992895 ) ) ;
#761 = ORIENTED_EDGE ( 'NONE', *, *, #22188, .T. ) ;
#762 = CARTESIAN_POINT ( 'NONE',  ( 2.591254417889934825, -3.476099799987327987, -44.10000000002499121 ) ) ;
#763 = CARTESIAN_POINT ( 'NONE',  ( 24.98081130624543889, 13.71897605842228529, 4.999998581000003384 ) ) ;
#764 = CARTESIAN_POINT ( 'NONE',  ( -2.496099253731141943, 5.577352528212363048, -22.73780126169999605 ) ) ;
#765 = CARTESIAN_POINT ( 'NONE',  ( -12.41345480022557446, -25.68646278880473233, -33.41489075299887901 ) ) ;
#766 = CARTESIAN_POINT ( 'NONE',  ( 11.20000000009999930, -22.00000000000000000, -31.28675134584999640 ) ) ;
#767 = B_SPLINE_CURVE_WITH_KNOTS ( 'NONE', 3,
 ( #13205, #8639, #22518, #965, #1269, #18235 ),
 .UNSPECIFIED., .F., .F.,
 ( 4, 2, 4 ),
 ( 0.000000000000000000, 0.5000000000000000000, 1.000000000000000000 ),
 .UNSPECIFIED. ) ;
#768 = CARTESIAN_POINT ( 'NONE',  ( 20.19076655603537418, -17.71015691556361205, 86.78285841154168168 ) ) ;
#769 = VECTOR ( 'NONE', #17966, 1000.000000000000114 ) ;
#770 = DIRECTION ( 'NONE',  ( 0.000000000000000000, 0.000000000000000000, 1.000000000000000000 ) ) ;
#771 = CARTESIAN_POINT ( 'NONE',  ( 4.647199600633202365, 1.656603404052558348, -45.17627377572499370 ) ) ;
#772 = ADVANCED_FACE ( 'NONE', ( #6236 ), #4729, .F. ) ;
#773 = CARTESIAN_POINT ( 'NONE',  ( -7.999999999947260854, -112.5823803020635125, 6.087179798330493163 ) ) ;
#774 = CARTESIAN_POINT ( 'NONE',  ( 9.339631244007776445, -25.12005762863061165, 204.5931320852415354 ) ) ;
#775 = DIRECTION ( 'NONE',  ( -1.000000000000000000, 5.687697999151106851E-16, -6.771501495036750356E-12 ) ) ;
#776 = CARTESIAN_POINT ( 'NONE',  ( -27.79999999999999716, -2.358414161360000020E-11, 229.1414213560000235 ) ) ;
#777 = CARTESIAN_POINT ( 'NONE',  ( -16.95738181130097288, -10.10243747011873872, -0.6999999999999783062 ) ) ;
#778 = ORIENTED_EDGE ( 'NONE', *, *, #1992, .T. ) ;
#779 = CARTESIAN_POINT ( 'NONE',  ( -2.448179507319817816, 5.395419651867324973, -32.72635571290000911 ) ) ;
#780 = CIRCLE ( 'NONE', #14848, 17.84349269770000035 ) ;
#781 = EDGE_LOOP ( 'NONE', ( #13468, #9312, #24772, #16453 ) ) ;
#782 = EDGE_CURVE ( 'NONE', #19357, #7295, #2457, .T. ) ;
#783 = DIRECTION ( 'NONE',  ( 0.7071067811865475727, 0.7071067811865475727, 0.000000000000000000 ) ) ;
#784 = CARTESIAN_POINT ( 'NONE',  ( 3.346097069915054512, -4.318458891539398437, -53.30430438132499660 ) ) ;
#785 = ORIENTED_EDGE ( 'NONE', *, *, #9500, .F. ) ;
#786 = ORIENTED_EDGE ( 'NONE', *, *, #29103, .T. ) ;
#787 = ADVANCED_FACE ( 'NONE', ( #14575 ), #4508, .F. ) ;
#788 = DIRECTION ( 'NONE',  ( 0.8660254037843287955, -0.5000000000001901812, 4.086617732256023781E-17 ) ) ;
#789 = ORIENTED_EDGE ( 'NONE', *, *, #21453, .T. ) ;
#790 = VERTEX_POINT ( 'NONE', #19287 ) ;
#791 = CARTESIAN_POINT ( 'NONE',  ( -10.58956532309999865, -24.61949706369999902, -1.102843534499998945 ) ) ;
#792 = CARTESIAN_POINT ( 'NONE',  ( 24.66346747934186112, 14.28208995963568739, 3.997248600000002927 ) ) ;
#793 = CARTESIAN_POINT ( 'NONE',  ( -9.700000000002093614, -15.94902145826220696, -35.53273252502236090 ) ) ;
#794 = CARTESIAN_POINT ( 'NONE',  ( 2.543356874222871156, 4.353805031640042067, -35.69999999999999574 ) ) ;
#795 = EDGE_CURVE ( 'NONE', #974, #18728, #25586, .T. ) ;
#796 = CARTESIAN_POINT ( 'NONE',  ( -12.41832131460176392, -28.28617032314356905, -23.36932019586331677 ) ) ;
#797 = CARTESIAN_POINT ( 'NONE',  ( -3.831450486774387265, 1.635689702191160944, -0.6999999999999992895 ) ) ;
#798 = CYLINDRICAL_SURFACE ( 'NONE', #20779, 26.80000000000002203 ) ;
#799 = CARTESIAN_POINT ( 'NONE',  ( -27.50000000000000000, 1.776356839399999804E-15, 43.60555127550000520 ) ) ;
#800 = DIRECTION ( 'NONE',  ( 0.000000000000000000, 0.000000000000000000, 1.000000000000000000 ) ) ;
#801 = CARTESIAN_POINT ( 'NONE',  ( 1.086829820489895848, 5.988658659452708477, -14.62400681849999806 ) ) ;
#802 = CARTESIAN_POINT ( 'NONE',  ( -2.448179507325345838, 5.395419651858992971, -30.72635571289999845 ) ) ;
#803 = DIRECTION ( 'NONE',  ( 0.4353787270609792981, 0.9002473904559574747, 0.000000000000000000 ) ) ;
#804 = B_SPLINE_CURVE_WITH_KNOTS ( 'NONE', 5,
 ( #6023, #8370, #8687, #25708, #20976, #25393 ),
 .UNSPECIFIED., .F., .F.,
 ( 6, 6 ),
 ( -7.118285296629999870, 0.000000000000000000 ),
 .UNSPECIFIED. ) ;
#805 = EDGE_CURVE ( 'NONE', #28870, #3434, #12807, .T. ) ;
#806 = CARTESIAN_POINT ( 'NONE',  ( 10.69999999999999929, -27.00000000000000000, -28.40000000000000213 ) ) ;
#807 = CARTESIAN_POINT ( 'NONE',  ( 11.08346179031908640, -28.41490585489484033, 193.6055512750000105 ) ) ;
#808 = SURFACE_SIDE_STYLE ('',( #24564 ) ) ;
#809 = CARTESIAN_POINT ( 'NONE',  ( -28.50000000000000000, -4.181985830669999980E-14, 229.2404163060000144 ) ) ;
#810 = DIRECTION ( 'NONE',  ( 0.000000000000000000, 1.000000000000000000, 0.000000000000000000 ) ) ;
#811 = CARTESIAN_POINT ( 'NONE',  ( 6.915128059151116610E-14, -5.777949443891209499E-13, 232.1412452697749984 ) ) ;
#812 = CARTESIAN_POINT ( 'NONE',  ( -8.699999999655181782, -13.66682223737418944, -36.55330428419230060 ) ) ;
#813 = CARTESIAN_POINT ( 'NONE',  ( -27.54391552379999908, 3.373045395949999841E-15, 92.95625301640001226 ) ) ;
#814 = ORIENTED_EDGE ( 'NONE', *, *, #9548, .T. ) ;
#815 = EDGE_CURVE ( 'NONE', #10804, #9494, #21654, .T. ) ;
#816 = CARTESIAN_POINT ( 'NONE',  ( -8.000000000000000000, -17.05999687705277879, -77.21601615383784178 ) ) ;
#817 = CARTESIAN_POINT ( 'NONE',  ( 9.000000000000000000, 20.99999999990000887, -67.10000000019999788 ) ) ;
#818 = ORIENTED_EDGE ( 'NONE', *, *, #11201, .T. ) ;
#819 = CARTESIAN_POINT ( 'NONE',  ( 0.000000000000000000, 0.000000000000000000, 90.00000000000000000 ) ) ;
#820 = CARTESIAN_POINT ( 'NONE',  ( 7.785475348737113777, -115.2733928504967764, 21.61366257841296701 ) ) ;
#821 = ORIENTED_EDGE ( 'NONE', *, *, #27749, .F. ) ;
#822 = CARTESIAN_POINT ( 'NONE',  ( -0.8355101799141004815, -26.78702284090145014, 4.280685865825344827 ) ) ;
#823 = ORIENTED_EDGE ( 'NONE', *, *, #1132, .F. ) ;
#824 = ORIENTED_EDGE ( 'NONE', *, *, #27429, .T. ) ;
#825 = FILL_AREA_STYLE_COLOUR ( '', #13827 ) ;
#826 = ORIENTED_EDGE ( 'NONE', *, *, #17759, .F. ) ;
#827 = CARTESIAN_POINT ( 'NONE',  ( 133283.2432719999924, 454259.0741890000063, -160669.1380380000046 ) ) ;
#828 = B_SPLINE_CURVE_WITH_KNOTS ( 'NONE', 3,
 ( #13806, #6715, #27644, #25299, #3733, #13332 ),
 .UNSPECIFIED., .F., .F.,
 ( 4, 2, 4 ),
 ( 0.000000000000000000, 0.5000000000000000000, 1.000000000000000000 ),
 .UNSPECIFIED. ) ;
#829 = DIRECTION ( 'NONE',  ( 6.181308505765962611E-12, -0.4082287037029531107, -0.9128796883888953273 ) ) ;
#830 = LINE ( 'NONE', #18100, #19769 ) ;
#831 = ORIENTED_EDGE ( 'NONE', *, *, #20654, .T. ) ;
#832 = CARTESIAN_POINT ( 'NONE',  ( -19.80526803560000104, 19.50877411510000314, 227.8000000000000114 ) ) ;
#833 = CARTESIAN_POINT ( 'NONE',  ( 0.5184513693225726305, -28.49550581263314086, 6.099998581000020792 ) ) ;
#834 = CARTESIAN_POINT ( 'NONE',  ( 19.76603533419210734, 19.51852340513930173, 0.7754612589999931860 ) ) ;
#835 = CARTESIAN_POINT ( 'NONE',  ( -7.999999999655180716, -13.66682223735657864, -36.55330428419717492 ) ) ;
#836 = MANIFOLD_SOLID_BREP ( 'PartBody', #31118 ) ;
#837 = CARTESIAN_POINT ( 'NONE',  ( 0.8228371056950706253, -6.016286819831330845, -0.9731240479999986315 ) ) ;
#838 = CARTESIAN_POINT ( 'NONE',  ( -1.058439502263211374, 6.005994971325610443, -19.83583244400000112 ) ) ;
#839 = CARTESIAN_POINT ( 'NONE',  ( 0.000000000000000000, -17.25771824150000100, 5.000000000000000000 ) ) ;
#840 = EDGE_CURVE ( 'NONE', #23934, #21744, #20728, .T. ) ;
#841 = FACE_OUTER_BOUND ( 'NONE', #10613, .T. ) ;
#842 = CARTESIAN_POINT ( 'NONE',  ( 23.74292845531203966, -13.87604159492686939, 226.1000000000000512 ) ) ;
#843 = CARTESIAN_POINT ( 'NONE',  ( -28.49999999979999998, 4.805538726630000923, 229.2404163060000144 ) ) ;
#844 = DIRECTION ( 'NONE',  ( 1.000000000000000000, 0.000000000000000000, 0.000000000000000000 ) ) ;
#845 = EDGE_CURVE ( 'NONE', #4569, #29453, #19752, .T. ) ;
#846 = EDGE_CURVE ( 'NONE', #15698, #27653, #3362, .T. ) ;
#847 = CARTESIAN_POINT ( 'NONE',  ( -3.046043134630462390, 1.783682052046422939, -0.6999999999999784173 ) ) ;
#848 = CARTESIAN_POINT ( 'NONE',  ( -11.66358246699999945, -24.14124255240000139, -1.399999999999998579 ) ) ;
#849 = DIRECTION ( 'NONE',  ( -0.9880370573969196046, 0.1542166437529879086, -5.551115123125782071E-14 ) ) ;
#850 = ORIENTED_EDGE ( 'NONE', *, *, #20772, .T. ) ;
#851 = CARTESIAN_POINT ( 'NONE',  ( -5.035266659556940638, -1.323295706752037670, -55.65102360502499579 ) ) ;
#852 = CARTESIAN_POINT ( 'NONE',  ( 26.71513120331084679, 4.908099852734520319, 0.000000000000000000 ) ) ;
#853 = CARTESIAN_POINT ( 'NONE',  ( -1.102325287918849650, -5.983340188646091740, -3.525234013000005717 ) ) ;
#854 = CARTESIAN_POINT ( 'NONE',  ( -3.916350486798555242, 2.029077553960367819, -38.46881641891648940 ) ) ;
#855 = CARTESIAN_POINT ( 'NONE',  ( -4.557930684098742802, 0.9655407268836344592, -68.10000000002501963 ) ) ;
#856 = ORIENTED_EDGE ( 'NONE', *, *, #2374, .F. ) ;
#857 = ORIENTED_EDGE ( 'NONE', *, *, #6995, .T. ) ;
#858 = CARTESIAN_POINT ( 'NONE',  ( -2.888061030901512893, 2.091444806125899891, -88.52261276243450538 ) ) ;
#859 = SHAPE_REPRESENTATION_RELATIONSHIP ( 'NONE' , 'NONE' ,  #19621, #20057 ) ;
#860 = EDGE_LOOP ( 'NONE', ( #6960, #16558, #28447, #28985 ) ) ;
#861 = DIRECTION ( 'NONE',  ( 0.2815395311429196301, 0.9595496299847262600, 0.000000000000000000 ) ) ;
#862 = CARTESIAN_POINT ( 'NONE',  ( 17.18658402241074867, -10.09981795543446736, -0.6999999989999727834 ) ) ;
#863 = ORIENTED_EDGE ( 'NONE', *, *, #7156, .T. ) ;
#864 = CARTESIAN_POINT ( 'NONE',  ( 1.008954696561116027, 5.412080152108726949, -62.62744533512499601 ) ) ;
#865 = CARTESIAN_POINT ( 'NONE',  ( 0.8057560762813021915, -28.48917411425644275, 6.073787920303829857 ) ) ;
#866 = AXIS2_PLACEMENT_3D ( 'NONE', #19748, #7622, #5419 ) ;
#867 = CARTESIAN_POINT ( 'NONE',  ( -27.61404081990094994, 9.332834367751024374, 0.7595836940000044724 ) ) ;
#868 = CARTESIAN_POINT ( 'NONE',  ( 12.12499559729999810, 20.99999999999999645, -55.73512174120000395 ) ) ;
#869 = STYLED_ITEM ( 'NONE', ( #24313 ), #836 ) ;
#870 = DIRECTION ( 'NONE',  ( 0.000000000000000000, 1.000000000000000000, 0.000000000000000000 ) ) ;
#871 = ORIENTED_EDGE ( 'NONE', *, *, #27753, .F. ) ;
#872 = UNCERTAINTY_MEASURE_WITH_UNIT (LENGTH_MEASURE( 1.000000000000000082E-05 ), #5198, 'distance_accuracy_value', 'NONE');
#873 = CARTESIAN_POINT ( 'NONE',  ( 1.100000000000000089, -26.77741585740000119, 5.000000000000000000 ) ) ;
#874 = CARTESIAN_POINT ( 'NONE',  ( 11.20000000009999930, -27.00000000000000355, -22.62649730800000114 ) ) ;
#875 = ORIENTED_EDGE ( 'NONE', *, *, #15893, .F. ) ;
#876 = CARTESIAN_POINT ( 'NONE',  ( 11.45957740435851235, -24.29669185712473478, 36.78285841129288514 ) ) ;
#877 = DIRECTION ( 'NONE',  ( -0.000000000000000000, -0.9396926207858126157, -0.3420201433259318913 ) ) ;
#878 = CARTESIAN_POINT ( 'NONE',  ( 6.760007715859398303, 5.672256964398498802, -40.24571374337934770 ) ) ;
#879 = EDGE_CURVE ( 'NONE', #15714, #12853, #23989, .T. ) ;
#880 = CARTESIAN_POINT ( 'NONE',  ( -7.131609927916050751, 9.777910867662733096, 232.0000000000051159 ) ) ;
#881 = DIRECTION ( 'NONE',  ( -0.000000000000000000, -0.000000000000000000, -1.000000000000000000 ) ) ;
#882 = PRODUCT_DEFINITION_SHAPE ( 'NONE', 'NONE',  #31119 ) ;
#883 = CARTESIAN_POINT ( 'NONE',  ( 3.509739097420207621, -2.501532857717466474, -0.6999999999999992895 ) ) ;
#884 = CARTESIAN_POINT ( 'NONE',  ( 14.58748419594687817, -28.00135611681330516, 0.5017677510000262409 ) ) ;
#886 = EDGE_CURVE ( 'NONE', #22309, #15300, #28972, .T. ) ;
#885 = CARTESIAN_POINT ( 'NONE',  ( 27.76135144349999706, -3.399672736829999707E-15, 142.3385858900000187 ) ) ;
#887 = ORIENTED_EDGE ( 'NONE', *, *, #20994, .F. ) ;
#888 = CARTESIAN_POINT ( 'NONE',  ( -10.69999999999999929, -27.00000000000000000, -31.39999999999999858 ) ) ;
#889 = CARTESIAN_POINT ( 'NONE',  ( 23.69119887989999995, 20.94188554249999967, 222.0000000000000000 ) ) ;
#890 = MANIFOLD_SOLID_BREP ( 'PartBody', #23115 ) ;
#891 = AXIS2_PLACEMENT_3D ( 'NONE', #15373, #6397, #3885 ) ;
#892 = CARTESIAN_POINT ( 'NONE',  ( -19.36389667587701524, -18.53702679572193546, 93.21714158842225117 ) ) ;
#893 = CARTESIAN_POINT ( 'NONE',  ( -0.6145358956450698296, -3.890912529351672422, -68.10000000002501963 ) ) ;
#894 = ORIENTED_EDGE ( 'NONE', *, *, #4532, .F. ) ;
#895 = CARTESIAN_POINT ( 'NONE',  ( 10.58956533789999988, -24.61949705740000027, -1.102843518299999381 ) ) ;
#896 = B_SPLINE_CURVE_WITH_KNOTS ( 'NONE', 3,
 ( #3635, #22846, #20952, #8825, #16225, #8506 ),
 .UNSPECIFIED., .F., .F.,
 ( 4, 2, 4 ),
 ( 0.000000000000000000, 0.5000000000000000000, 1.000000000000000000 ),
 .UNSPECIFIED. ) ;
#897 = CARTESIAN_POINT ( 'NONE',  ( 14.40197535836999876, -22.00000000000000000, -31.28675134584999640 ) ) ;
#898 = CARTESIAN_POINT ( 'NONE',  ( 3.861721477338983632, 0.2146938847481238977, -40.92168819670553148 ) ) ;
#899 = CARTESIAN_POINT ( 'NONE',  ( 2.840551633548176191, -3.955783487875848881, -62.27197827312499356 ) ) ;
#900 = EDGE_LOOP ( 'NONE', ( #20816, #30735 ) ) ;
#901 = CONTEXT_DEPENDENT_SHAPE_REPRESENTATION ( #28088, #19010 ) ;
#902 = VERTEX_POINT ( 'NONE', #27140 ) ;
#903 = CIRCLE ( 'NONE', #21011, 2.999999999999999556 ) ;
#904 = CARTESIAN_POINT ( 'NONE',  ( 14.23756994129695030, -27.32973605077160073, 0.7069240339999949274 ) ) ;
#905 = ORIENTED_EDGE ( 'NONE', *, *, #2120, .T. ) ;
#906 = ORIENTED_EDGE ( 'NONE', *, *, #846, .F. ) ;
#907 = CARTESIAN_POINT ( 'NONE',  ( 16.59368952141597831, 11.95034963011661944, -0.6999999999999784173 ) ) ;
#908 = EDGE_CURVE ( 'NONE', #7204, #15025, #26492, .T. ) ;
#909 = CARTESIAN_POINT ( 'NONE',  ( 24.95427444975690889, -13.76797447160702070, 3.899998581000013509 ) ) ;
#910 = CARTESIAN_POINT ( 'NONE',  ( -24.75565187725877081, -14.12271910255536689, 223.9000014190000059 ) ) ;
#911 = CIRCLE ( 'NONE', #3909, 4.000000000000001776 ) ;
#912 = CARTESIAN_POINT ( 'NONE',  ( 8.700000000283074186, -17.54022835462044227, -37.48857263400110895 ) ) ;
#913 = AXIS2_PLACEMENT_3D ( 'NONE', #1973, #13609, #2285 ) ;
#914 = CYLINDRICAL_SURFACE ( 'NONE', #15454, 3.000000000000002220 ) ;
#915 = CARTESIAN_POINT ( 'NONE',  ( 10.69999999999999929, -27.00000000000000000, -28.40000000000000213 ) ) ;
#916 = ORIENTED_EDGE ( 'NONE', *, *, #7146, .F. ) ;
#917 = CARTESIAN_POINT ( 'NONE',  ( 1.979015836267390194, -4.452375488360101663, -44.10000000002499121 ) ) ;
#918 = CARTESIAN_POINT ( 'NONE',  ( 10.69999999999999929, -82.23832021929999314, -29.25398675779999991 ) ) ;
#919 = CARTESIAN_POINT ( 'NONE',  ( -2.322678811625146444, -3.635533071076381795, -22.20891267860000795 ) ) ;
#920 = CARTESIAN_POINT ( 'NONE',  ( 12.55799324160000019, 21.70000000000000284, -55.95247857500000066 ) ) ;
#921 = CARTESIAN_POINT ( 'NONE',  ( 20.30396079652883756, 20.00000000004620304, 1.000000000000000888 ) ) ;
#922 = CARTESIAN_POINT ( 'NONE',  ( -27.92857142820000149, 1.776356839399999804E-15, 187.9396849849999853 ) ) ;
#923 = CARTESIAN_POINT ( 'NONE',  ( -12.29999999970000069, -27.00000000000000000, -28.40000000001083791 ) ) ;
#924 = CARTESIAN_POINT ( 'NONE',  ( -1.909971040720825908, -5.612411004515823088, -46.51520033292499789 ) ) ;
#925 = AXIS2_PLACEMENT_3D ( 'NONE', #19192, #16825, #15877 ) ;
#926 = CARTESIAN_POINT ( 'NONE',  ( -16.17969668575259590, 11.89630849621310738, -1.400000000000001910 ) ) ;
#927 = CARTESIAN_POINT ( 'NONE',  ( 8.158046243928268382, -25.52871334855630536, 206.9076631228209635 ) ) ;
#928 = CARTESIAN_POINT ( 'NONE',  ( -10.69999999999829932, -27.75984822496048920, -25.47305230109693142 ) ) ;
#929 = DIRECTION ( 'NONE',  ( 1.000000000000000000, 0.000000000000000000, 0.000000000000000000 ) ) ;
#930 = CARTESIAN_POINT ( 'NONE',  ( 24.05715877135684622, -13.32261293554750914, 225.9948832293248415 ) ) ;
#931 = VERTEX_POINT ( 'NONE', #12655 ) ;
#932 = CARTESIAN_POINT ( 'NONE',  ( 3.853781668577745734, 2.900580182411895080, -33.29782172560000220 ) ) ;
#933 = AXIS2_PLACEMENT_3D ( 'NONE', #27960, #6400, #18514 ) ;
#934 = ORIENTED_EDGE ( 'NONE', *, *, #11925, .F. ) ;
#935 = CARTESIAN_POINT ( 'NONE',  ( -10.32522729140000095, -25.00000000000000000, -1.399999999999998579 ) ) ;
#936 = CARTESIAN_POINT ( 'NONE',  ( -5.473571180597741836, 3.247285761689575168, -51.31267869292499739 ) ) ;
#937 = ORIENTED_EDGE ( 'NONE', *, *, #11074, .T. ) ;
#938 = EDGE_LOOP ( 'NONE', ( #7881, #1510, #28414, #15809 ) ) ;
#939 = EDGE_CURVE ( 'NONE', #11197, #5944, #10463, .T. ) ;
#940 = DIRECTION ( 'NONE',  ( 0.000000000000000000, 0.000000000000000000, 1.000000000000000000 ) ) ;
#941 = MANIFOLD_SOLID_BREP ( 'PartBody', #9536 ) ;
#942 = ORIENTED_EDGE ( 'NONE', *, *, #4712, .F. ) ;
#943 = APPLICATION_CONTEXT ( 'automotive_design' ) ;
#944 = ORIENTED_EDGE ( 'NONE', *, *, #20701, .T. ) ;
#945 = CARTESIAN_POINT ( 'NONE',  ( 8.000000000289732682, -15.05691661385925961, -37.86814300156539304 ) ) ;
#946 = CARTESIAN_POINT ( 'NONE',  ( 24.96253706050071131, 13.75225324050492581, 4.689458287000014991 ) ) ;
#947 = EDGE_CURVE ( 'NONE', #18243, #19781, #29652, .T. ) ;
#948 = CARTESIAN_POINT ( 'NONE',  ( 0.5057536231481192246, -27.79562098839016571, 6.099998581000020792 ) ) ;
#949 = CARTESIAN_POINT ( 'NONE',  ( 8.000000000050000892, -13.98526668056139144, -73.96855033896248699 ) ) ;
#950 = DIRECTION ( 'NONE',  ( 3.924189347185962345E-12, -0.4082287037029530552, -0.9128796883888953273 ) ) ;
#951 = CARTESIAN_POINT ( 'NONE',  ( -22.97554861169999896, 15.65134970780000145, 222.0000000000000000 ) ) ;
#952 = CARTESIAN_POINT ( 'NONE',  ( -4.383977851963892114, 1.985334855346547966, -0.6999999999999992895 ) ) ;
#953 = CARTESIAN_POINT ( 'NONE',  ( 2.910738317039999947E-11, 21.69999999990000106, -70.09999999999999432 ) ) ;
#954 = DIRECTION ( 'NONE',  ( -1.000000000000000000, 5.687697999151106851E-16, -6.771501495036750356E-12 ) ) ;
#955 = CARTESIAN_POINT ( 'NONE',  ( 11.69999999989999928, -2.500000000000002220, -2.399999999999999467 ) ) ;
#956 = CARTESIAN_POINT ( 'NONE',  ( 3.550610403408205329, -5.007233058897099021, -12.12388893670000201 ) ) ;
#957 = CARTESIAN_POINT ( 'NONE',  ( -5.305719984766040120, 1.510612064730647131, -30.30158078970000091 ) ) ;
#958 = VECTOR ( 'NONE', #5157, 1000.000000000000114 ) ;
#959 = CARTESIAN_POINT ( 'NONE',  ( 0.000000000000000000, 0.000000000000000000, 115.0000000000000000 ) ) ;
#960 = ADVANCED_FACE ( 'NONE', ( #23523 ), #10927, .F. ) ;
#961 = CARTESIAN_POINT ( 'NONE',  ( 18.92356420714367360, 19.72862907665551546, 0.1494310229999962214 ) ) ;
#962 = CARTESIAN_POINT ( 'NONE',  ( 9.499999999998065547, -18.19953924290990344, -36.00725302081955448 ) ) ;
#963 = DIRECTION ( 'NONE',  ( 0.000000000000000000, 2.257145581549999994E-12, 1.000000000000000000 ) ) ;
#964 = CARTESIAN_POINT ( 'NONE',  ( 19.80538173989999962, 19.50875420239999869, 229.0000000000000000 ) ) ;
#965 = CARTESIAN_POINT ( 'NONE',  ( -9.947945353463017781, -14.47719179108256782, -74.14759643668045896 ) ) ;
#966 = CARTESIAN_POINT ( 'NONE',  ( 25.80996960090668679, 10.85703805089278617, 1.000000000000000888 ) ) ;
#967 = EDGE_LOOP ( 'NONE', ( #12615, #17366 ) ) ;
#968 = AXIS2_PLACEMENT_3D ( 'NONE', #3100, #14920, #144 ) ;
#969 = DIRECTION ( 'NONE',  ( 1.000000000000000000, 0.000000000000000000, 0.000000000000000000 ) ) ;
#970 = LINE ( 'NONE', #17624, #2207 ) ;
#971 = ORIENTED_EDGE ( 'NONE', *, *, #25154, .T. ) ;
#972 = CARTESIAN_POINT ( 'NONE',  ( -7.999999999697742226, -24.65319937755806379, -30.30964379067835424 ) ) ;
#973 = DIRECTION ( 'NONE',  ( -0.5000000000001898481, -0.8660254037843291286, 0.000000000000000000 ) ) ;
#974 = VERTEX_POINT ( 'NONE', #13912 ) ;
#975 = CARTESIAN_POINT ( 'NONE',  ( -4.182178350032519809, -27.18131967880235322, 20.25455995680620447 ) ) ;
#976 = ORIENTED_EDGE ( 'NONE', *, *, #14186, .T. ) ;
#977 = ORIENTED_EDGE ( 'NONE', *, *, #11138, .T. ) ;
#978 = AXIS2_PLACEMENT_3D ( 'NONE', #18506, #25756, #719 ) ;
#979 = VERTEX_POINT ( 'NONE', #23204 ) ;
#980 = CARTESIAN_POINT ( 'NONE',  ( -17.49331448440255343, 10.10821397335649152, -0.6999999999999784173 ) ) ;
#981 = EDGE_CURVE ( 'NONE', #18243, #12035, #20262, .T. ) ;
#982 = DIRECTION ( 'NONE',  ( 1.000000000000000000, 0.000000000000000000, 0.000000000000000000 ) ) ;
#983 = CARTESIAN_POINT ( 'NONE',  ( -7.999999999652784410, -17.12901166691730737, -37.73938230484767331 ) ) ;
#984 = FILL_AREA_STYLE_COLOUR ( '', #18846 ) ;
#985 = EDGE_CURVE ( 'NONE', #14751, #26486, #21786, .T. ) ;
#986 = CARTESIAN_POINT ( 'NONE',  ( -24.70450124751183552, 12.74984379616985386, 5.760266710000017554 ) ) ;
#987 = CARTESIAN_POINT ( 'NONE',  ( 4.785280386522178020, 31.71089591180988876, 1.000000000000000888 ) ) ;
#988 = CARTESIAN_POINT ( 'NONE',  ( -27.50000000000000000, 3.367667473009999970E-15, 186.3944487260000074 ) ) ;
#989 = CARTESIAN_POINT ( 'NONE',  ( -7.999999999658122363, -13.45788390610263541, -35.88763790175109136 ) ) ;
#990 = CARTESIAN_POINT ( 'NONE',  ( 4.345117593642236820, 2.039387521354418809, -3.416670051700001931 ) ) ;
#991 = CARTESIAN_POINT ( 'NONE',  ( 1.391539067366913018, -4.898323207587138128, -20.35785708919999948 ) ) ;
#992 = FACE_OUTER_BOUND ( 'NONE', #10653, .T. ) ;
#993 = CARTESIAN_POINT ( 'NONE',  ( 10.69999999999999929, -24.97510463969999961, -26.18619911029999869 ) ) ;
#994 = CARTESIAN_POINT ( 'NONE',  ( 25.22036945370000183, -13.27344566769999901, 224.7916409239999780 ) ) ;
#995 = ADVANCED_FACE ( 'NONE', ( #23367 ), #9025, .T. ) ;
#996 = CARTESIAN_POINT ( 'NONE',  ( -18.97091445539999910, 21.26865671750000075, 229.0000000000000000 ) ) ;
#997 = CARTESIAN_POINT ( 'NONE',  ( 10.69999999996385576, -38.97238336744932496, -26.38768795973993520 ) ) ;
#998 = VECTOR ( 'NONE', #23561, 1000.000000000000000 ) ;
#999 = AXIS2_PLACEMENT_3D ( 'NONE', #22838, #679, #10268 ) ;
#1000 = CARTESIAN_POINT ( 'NONE',  ( 24.34660549313293032, -12.78643034496977116, 224.8543268302984188 ) ) ;
#1001 = EDGE_CURVE ( 'NONE', #23549, #20463, #10068, .T. ) ;
#1002 = CARTESIAN_POINT ( 'NONE',  ( 3.184793790070000075, -18.07879718899999943, 230.6999999999999886 ) ) ;
#1003 = CARTESIAN_POINT ( 'NONE',  ( 23.76736455380283530, -13.83371703085023086, 223.8999999999988688 ) ) ;
#1004 = ORIENTED_EDGE ( 'NONE', *, *, #677, .F. ) ;
#1005 = CARTESIAN_POINT ( 'NONE',  ( -1.034595936873321076, -4.789217790999566127, -55.18033560642498969 ) ) ;
#1006 = DIRECTION ( 'NONE',  ( 0.000000000000000000, -1.000000000000000000, 2.257145581549999994E-12 ) ) ;
#1007 = CARTESIAN_POINT ( 'NONE',  ( 5.782996427689181651, 1.709881257618839356, -17.54190840230000603 ) ) ;
#1008 = CARTESIAN_POINT ( 'NONE',  ( -0.5080847461133405352, 4.304903296726419804, -39.57881079956060688 ) ) ;
#1009 = CARTESIAN_POINT ( 'NONE',  ( -4.561626939327173780, 0.9596751652757145035, -68.10000000002500542 ) ) ;
#1010 = ORIENTED_EDGE ( 'NONE', *, *, #19425, .F. ) ;
#1011 = VERTEX_POINT ( 'NONE', #27918 ) ;
#1012 = CARTESIAN_POINT ( 'NONE',  ( -3.873164306260329592, -2.119290473573849809, -95.69213427724059784 ) ) ;
#1013 =( NAMED_UNIT ( * ) SI_UNIT ( $, .STERADIAN. ) SOLID_ANGLE_UNIT ( ) );
#1014 = EDGE_LOOP ( 'NONE', ( #29479, #29790, #6627, #16562 ) ) ;
#1015 = CARTESIAN_POINT ( 'NONE',  ( -10.46447140189999914, 20.99999999999999645, -54.63552859760000047 ) ) ;
#1016 = EDGE_CURVE ( 'NONE', #725, #3834, #25246, .T. ) ;
#1017 = CARTESIAN_POINT ( 'NONE',  ( -8.699999999945166707, -111.9817663798742444, 5.760339591697572814 ) ) ;
#1018 = CARTESIAN_POINT ( 'NONE',  ( 1.094823181362614140, 5.872682718251108547, -62.94744533522500518 ) ) ;
#1019 = CARTESIAN_POINT ( 'NONE',  ( -10.69999999999979856, -29.23060343762547220, -26.39054106483859741 ) ) ;
#1020 = EDGE_CURVE ( 'NONE', #9868, #26249, #30013, .T. ) ;
#1021 = CARTESIAN_POINT ( 'NONE',  ( -25.96688743241739061, 8.776138983998601262, -0.6999999999999784173 ) ) ;
#1022 = CARTESIAN_POINT ( 'NONE',  ( -28.23997156040000078, -4.869988983339999855, 222.0000000000000000 ) ) ;
#1023 = PRESENTATION_STYLE_ASSIGNMENT (( #20206 ) ) ;
#1024 = EDGE_CURVE ( 'NONE', #18614, #4760, #2033, .T. ) ;
#1025 = CARTESIAN_POINT ( 'NONE',  ( 14.94562240850000023, -8.628859120750000500, 225.0000000000000000 ) ) ;
#1026 = ORIENTED_EDGE ( 'NONE', *, *, #11785, .F. ) ;
#1027 = CARTESIAN_POINT ( 'NONE',  ( 3.685684228007439778, 0.6162076564309076909, 230.7072465799053020 ) ) ;
#1028 = LINE ( 'NONE', #10770, #14022 ) ;
#1029 = ORIENTED_EDGE ( 'NONE', *, *, #5957, .T. ) ;
#1030 = CARTESIAN_POINT ( 'NONE',  ( 25.20859211119999799, -13.29584934979999922, 224.6894611300000122 ) ) ;
#1031 = CARTESIAN_POINT ( 'NONE',  ( -22.77466902118896996, -14.12660345815406338, 4.296357262948782285 ) ) ;
#1032 = CARTESIAN_POINT ( 'NONE',  ( -28.50000000000000000, 4.194175870809999815E-15, 222.0000000000000000 ) ) ;
#1033 = CARTESIAN_POINT ( 'NONE',  ( 21.36643726116283659, 17.24662705154594988, 0.02487530000000459651 ) ) ;
#1034 = CARTESIAN_POINT ( 'NONE',  ( 16.29899378166743062, -9.691472637822489133, 0.000000000000000000 ) ) ;
#1035 = CARTESIAN_POINT ( 'NONE',  ( 3.309176925312228956, -2.636077854372748774, -0.6999999999999992895 ) ) ;
#1036 = CARTESIAN_POINT ( 'NONE',  ( -23.23277431133845994, -15.26692929363520257, 4.999998581000003384 ) ) ;
#1037 = DIRECTION ( 'NONE',  ( 0.1090476345695675503, 0.6986477033489619792, 0.7071067811865496822 ) ) ;
#1038 = EDGE_LOOP ( 'NONE', ( #25052, #15396, #23007, #6576 ) ) ;
#1039 = FACE_OUTER_BOUND ( 'NONE', #21921, .T. ) ;
#1040 = CARTESIAN_POINT ( 'NONE',  ( 12.77819780750000156, 21.69999999929999390, -56.09999999999999432 ) ) ;
#1041 = CARTESIAN_POINT ( 'NONE',  ( 27.98881761119999823, 6.827871301039999175, 222.0000000000000000 ) ) ;
#1042 = FACE_OUTER_BOUND ( 'NONE', #3125, .T. ) ;
#1043 = CARTESIAN_POINT ( 'NONE',  ( 11.57608395239999943, -24.17108566339999953, -0.7028182531999965788 ) ) ;
#1044 = DIRECTION ( 'NONE',  ( 0.000000000000000000, 0.000000000000000000, 1.000000000000000000 ) ) ;
#1045 = CARTESIAN_POINT ( 'NONE',  ( -14.76964124820000102, 19.99999999999999645, -0.6999999999999992895 ) ) ;
#1046 = EDGE_CURVE ( 'NONE', #23432, #23963, #17250, .T. ) ;
#1047 = CARTESIAN_POINT ( 'NONE',  ( -0.8884012486115674401, 4.851036559086118416, -61.00324387862499975 ) ) ;
#1048 = ORIENTED_EDGE ( 'NONE', *, *, #17146, .F. ) ;
#1049 = CARTESIAN_POINT ( 'NONE',  ( 18.65395304217032901, 19.99999294228678792, 230.6088730870111476 ) ) ;
#1050 = EDGE_CURVE ( 'NONE', #7923, #29336, #21124, .T. ) ;
#1051 = EDGE_LOOP ( 'NONE', ( #1208, #22338, #9654, #26005 ) ) ;
#1052 = EDGE_CURVE ( 'NONE', #12887, #10989, #2292, .T. ) ;
#1053 = FACE_OUTER_BOUND ( 'NONE', #3329, .T. ) ;
#1054 = EDGE_CURVE ( 'NONE', #7914, #21685, #4510, .T. ) ;
#1055 = EDGE_LOOP ( 'NONE', ( #16172, #12715, #18535, #3982 ) ) ;
#1056 = FACE_OUTER_BOUND ( 'NONE', #19, .T. ) ;
#1057 = CARTESIAN_POINT ( 'NONE',  ( -23.73992238019999945, -12.43607998449999918, 225.0000000000000000 ) ) ;
#1058 = CARTESIAN_POINT ( 'NONE',  ( -24.68204616399999907, -14.25020164319999871, 223.9000014189999774 ) ) ;
#1059 = CARTESIAN_POINT ( 'NONE',  ( -17.22797207741465897, -26.41666101526536892, -33.83671177223448012 ) ) ;
#1060 = CARTESIAN_POINT ( 'NONE',  ( 24.83827472153076599, -12.48687851163286133, 5.104216618000034345 ) ) ;
#1061 = CARTESIAN_POINT ( 'NONE',  ( -0.1033151399490000039, -27.80006701330000141, 223.9040511909999793 ) ) ;
#1062 = ORIENTED_EDGE ( 'NONE', *, *, #30828, .F. ) ;
#1063 = CARTESIAN_POINT ( 'NONE',  ( 2.841665746808334170, -3.648605867525280821, -44.10000000002500542 ) ) ;
#1064 = CARTESIAN_POINT ( 'NONE',  ( -9.000000000000000000, 21.69999999990000106, -67.10000000019999788 ) ) ;
#1065 = AXIS2_PLACEMENT_3D ( 'NONE', #30651, #18673, #6410 ) ;
#1066 = CARTESIAN_POINT ( 'NONE',  ( 4.725722714813314518, -3.873618144263061946, -24.59674734060000745 ) ) ;
#1067 = CARTESIAN_POINT ( 'NONE',  ( 23.62133197435833409, -12.66014020633680914, 4.296357262547505940 ) ) ;
#1068 = DIRECTION ( 'NONE',  ( 0.000000000000000000, 0.5000000000001900702, -0.8660254037843290176 ) ) ;
#1069 = B_SPLINE_CURVE_WITH_KNOTS ( 'NONE', 3,
 ( #24794, #9698, #21667, #19302, #28895, #7344, #26539, #4979, #14590, #24178, #2618, #19455, #12210, #21822 ),
 .UNSPECIFIED., .F., .F.,
 ( 4, 2, 2, 2, 2, 2, 4 ),
 ( 0.000000000000000000, 0.2500000000000449640, 0.3750000000000674460, 0.4375000000000606182, 0.5000000000000538458, 0.7500000000000269784, 1.000000000000000000 ),
 .UNSPECIFIED. ) ;
#1070 = CARTESIAN_POINT ( 'NONE',  ( -1.100000000000000089, -27.47799119300000115, 225.0000000000000000 ) ) ;
#1071 = FACE_OUTER_BOUND ( 'NONE', #24230, .T. ) ;
#1072 = CARTESIAN_POINT ( 'NONE',  ( 5.643028086411650435, 2.011589847869324377, -45.44627377572500393 ) ) ;
#1073 = CARTESIAN_POINT ( 'NONE',  ( 0.000000000000000000, -1.776356839399999804E-15, 227.6412452697800006 ) ) ;
#1074 = CARTESIAN_POINT ( 'NONE',  ( 7.662090775718879421, -25.68204763724676454, 207.5103208889252357 ) ) ;
#1075 = CARTESIAN_POINT ( 'NONE',  ( -17.83931601680000156, 20.00000000000000000, 230.7000111870000012 ) ) ;
#1076 = CARTESIAN_POINT ( 'NONE',  ( 17.16657240420000008, 12.63606054916536614, 0.05106179917585308009 ) ) ;
#1077 = CARTESIAN_POINT ( 'NONE',  ( 6.496986506900683800, -26.00150201275823392, 21.45239876629313258 ) ) ;
#1078 = ORIENTED_EDGE ( 'NONE', *, *, #22876, .T. ) ;
#1079 = CARTESIAN_POINT ( 'NONE',  ( 2.224662748255027633, -4.232576503996232198, -34.14471934059999825 ) ) ;
#1080 = ORIENTED_EDGE ( 'NONE', *, *, #19351, .T. ) ;
#1081 = DIRECTION ( 'NONE',  ( -1.000000000000000000, 5.687697999151106851E-16, -6.771501495036750356E-12 ) ) ;
#1082 = CARTESIAN_POINT ( 'NONE',  ( 4.421972129926214023, 1.961202595004077232, -52.27998794302499164 ) ) ;
#1083 = ORIENTED_EDGE ( 'NONE', *, *, #8304, .F. ) ;
#1084 = EDGE_LOOP ( 'NONE', ( #29264, #25787, #11237, #9561 ) ) ;
#1085 = SHAPE_DEFINITION_REPRESENTATION ( #1867, #27424 ) ;
#1086 = AXIS2_PLACEMENT_3D ( 'NONE', #2652, #28767, #12245 ) ;
#1087 = ORIENTED_EDGE ( 'NONE', *, *, #23894, .T. ) ;
#1088 = EDGE_LOOP ( 'NONE', ( #13311, #8137, #3315, #26948, #18723, #26281, #19667, #6923, #6456, #7311, #3860, #7841, #18721, #26251, #1988, #26660, #13386, #29370, #11303, #12417, #30625, #13343, #13248, #22269, #29067, #21456, #29439, #26048, #28817, #4264, #9391, #19279, #17779, #17940, #28601, #166, #332, #23931, #19123, #1813, #6184, #27951, #18968, #5521 ) ) ;
#1089 = CARTESIAN_POINT ( 'NONE',  ( 24.14840829003316003, 13.77363891342296043, 4.098702612000016288 ) ) ;
#1090 = CARTESIAN_POINT ( 'NONE',  ( 17.33054985630230505, 9.902801559281119381, -4.336808689942018722E-16 ) ) ;
#1091 = FACE_OUTER_BOUND ( 'NONE', #5069, .T. ) ;
#1092 = CARTESIAN_POINT ( 'NONE',  ( -7.453090060300354480, -2.907137518772246576, 27.99999999999999645 ) ) ;
#1093 = CARTESIAN_POINT ( 'NONE',  ( -13.99999999969999820, 20.99999999999999645, -51.10000000000000142 ) ) ;
#1094 = CARTESIAN_POINT ( 'NONE',  ( -3.819171446108351464, 1.704510517422477722, -0.6999999999999991784 ) ) ;
#1095 = CARTESIAN_POINT ( 'NONE',  ( -1.392415278799822298, -4.107851135794777342, -0.07563051270000181736 ) ) ;
#1096 = CARTESIAN_POINT ( 'NONE',  ( -7.453090060300356257, -2.907137518772246576, 20.00000000000000000 ) ) ;
#1097 = CARTESIAN_POINT ( 'NONE',  ( -22.97593529893700648, 15.65128280014837081, 8.000000000000007105 ) ) ;
#1098 = CARTESIAN_POINT ( 'NONE',  ( 3.212457031643341399, -4.530353719951508928, -13.12388893670000378 ) ) ;
#1099 = CARTESIAN_POINT ( 'NONE',  ( 5.012492089930680628, -1.133010176900860477, -31.84627053310000733 ) ) ;
#1100 = CARTESIAN_POINT ( 'NONE',  ( -20.22682926819999949, -27.00000000000000000, -28.39999999989999679 ) ) ;
#1101 = EDGE_CURVE ( 'NONE', #7295, #11539, #25974, .T. ) ;
#1102 = CARTESIAN_POINT ( 'NONE',  ( -24.40276494859777046, -13.31831424753606008, 225.8868154035638156 ) ) ;
#1103 = FACE_BOUND ( 'NONE', #21065, .T. ) ;
#1104 = CARTESIAN_POINT ( 'NONE',  ( -11.50000000000000000, 22.40709319595134730, -62.85117013414870257 ) ) ;
#1105 = CARTESIAN_POINT ( 'NONE',  ( 3.326864889560396499, 2.374768916159259113, -35.37908769470001147 ) ) ;
#1106 = AXIS2_PLACEMENT_3D ( 'NONE', #23921, #152, #26722 ) ;
#1107 = B_SPLINE_CURVE_WITH_KNOTS ( 'NONE', 5,
 ( #18342, #6385, #25594, #4027, #13625, #1670, #26513, #9990, #12040, #12348, #2752, #12182 ),
 .UNSPECIFIED., .F., .F.,
 ( 6, 3, 3, 6 ),
 ( 0.000000000000000000, 2.812352519340000079, 5.624713925070000009, 7.679355244459999952 ),
 .UNSPECIFIED. ) ;
#1108 = CARTESIAN_POINT ( 'NONE',  ( 17.99934522968721495, 20.17941515401252417, -0.6999999999999784173 ) ) ;
#1109 = CARTESIAN_POINT ( 'NONE',  ( 10.35000000029999967, -25.00000000000000000, -7.274962170099999348 ) ) ;
#1110 = CARTESIAN_POINT ( 'NONE',  ( 0.000000000000000000, 0.000000000000000000, 36.39444872359999295 ) ) ;
#1111 = EDGE_LOOP ( 'NONE', ( #26780, #25862, #20091, #12457 ) ) ;
#1112 = ORIENTED_EDGE ( 'NONE', *, *, #24670, .T. ) ;
#1113 = EDGE_CURVE ( 'NONE', #7730, #30387, #4258, .T. ) ;
#1114 = CYLINDRICAL_SURFACE ( 'NONE', #26357, 1.100000000000002309 ) ;
#1115 = DIRECTION ( 'NONE',  ( 0.000000000000000000, 0.000000000000000000, 1.000000000000000000 ) ) ;
#1116 = EDGE_LOOP ( 'NONE', ( #4416, #12493, #12956, #27444 ) ) ;
#1117 = CARTESIAN_POINT ( 'NONE',  ( -22.63992238021892334, -14.34133587286723888, 224.9035646515725659 ) ) ;
#1118 = CARTESIAN_POINT ( 'NONE',  ( -24.46845037339999962, -13.19716075180000026, 224.2397332909999932 ) ) ;
#1119 = ORIENTED_EDGE ( 'NONE', *, *, #21500, .T. ) ;
#1120 = CARTESIAN_POINT ( 'NONE',  ( -0.1474957663552681764, -26.80000000000001492, 3.899999999999999911 ) ) ;
#1121 = ORIENTED_EDGE ( 'NONE', *, *, #17384, .F. ) ;
#1122 = ORIENTED_EDGE ( 'NONE', *, *, #9649, .F. ) ;
#1123 = ORIENTED_EDGE ( 'NONE', *, *, #11315, .F. ) ;
#1124 = B_SPLINE_CURVE_WITH_KNOTS ( 'NONE', 3,
 ( #23450, #1880, #6119, #11478, #30363, #30677, #8791, #22968, #3599, #6436, #1259, #28303 ),
 .UNSPECIFIED., .F., .F.,
 ( 4, 2, 2, 2, 2, 4 ),
 ( 0.000000000000000000, 0.2500000000000007216, 0.5000000000000014433, 0.6250000000000013323, 0.7500000000000012212, 1.000000000000000000 ),
 .UNSPECIFIED. ) ;
#1125 = CARTESIAN_POINT ( 'NONE',  ( 26.32519403849999762, 9.219495376610002069, 230.6577119970000069 ) ) ;
#1126 = CARTESIAN_POINT ( 'NONE',  ( -10.69999999969999926, -27.00000000000000000, -28.40000000000000213 ) ) ;
#1127 = FACE_OUTER_BOUND ( 'NONE', #4296, .T. ) ;
#1128 = DIRECTION ( 'NONE',  ( 0.000000000000000000, 0.000000000000000000, -1.000000000000000000 ) ) ;
#1129 = CARTESIAN_POINT ( 'NONE',  ( -24.34137756212881953, 13.42980562992878646, 6.099998581000020792 ) ) ;
#1130 = FACE_OUTER_BOUND ( 'NONE', #3387, .T. ) ;
#1131 = CARTESIAN_POINT ( 'NONE',  ( 9.797681423453981964, -25.69548940455785413, 203.8387348960827694 ) ) ;
#1132 = EDGE_CURVE ( 'NONE', #6418, #6498, #7888, .T. ) ;
#1133 = CARTESIAN_POINT ( 'NONE',  ( 9.000000000000000000, -55.00000000000001421, -42.39999999999999858 ) ) ;
#1134 = ORIENTED_EDGE ( 'NONE', *, *, #23818, .T. ) ;
#1135 = CARTESIAN_POINT ( 'NONE',  ( 3.123710955063065065, -2.074832491810036039, 0.04124526979999709742 ) ) ;
#1136 = CARTESIAN_POINT ( 'NONE',  ( -5.635022120045706018, 0.7837540840481607152, -18.25159460730000660 ) ) ;
#1137 = DIRECTION ( 'NONE',  ( 0.000000000000000000, 0.000000000000000000, -1.000000000000000000 ) ) ;
#1138 = CARTESIAN_POINT ( 'NONE',  ( 10.69999999999999929, -24.95051888409999918, -26.20881396380000083 ) ) ;
#1139 = CARTESIAN_POINT ( 'NONE',  ( 2.127246859547380353, -2.914123423641564070, -88.52261276302716908 ) ) ;
#1140 = CARTESIAN_POINT ( 'NONE',  ( -28.35924375250000296, -1.021553995729999846E-14, 229.7625741969999922 ) ) ;
#1141 = CARTESIAN_POINT ( 'NONE',  ( -18.29999999989999893, -27.00000000000000000, -28.39999999989999679 ) ) ;
#1142 = DIRECTION ( 'NONE',  ( -4.428977494234582379E-12, -0.8987940462991651502, 0.4383711467890810676 ) ) ;
#1143 = CARTESIAN_POINT ( 'NONE',  ( -1.854631282479999976, -18.18682133599999773, 230.6999999999999886 ) ) ;
#1144 = CARTESIAN_POINT ( 'NONE',  ( 3.827451119382927036, -1.796035916205476424, -39.94098974597989837 ) ) ;
#1145 = ORIENTED_EDGE ( 'NONE', *, *, #22578, .F. ) ;
#1146 = CARTESIAN_POINT ( 'NONE',  ( 3.312932182603874232, 3.356011527877053702, -57.70805965152499795 ) ) ;
#1147 = VECTOR ( 'NONE', #1778, 1000.000000000000114 ) ;
#1148 = CARTESIAN_POINT ( 'NONE',  ( -4.861312627776431583, -9.716283825163692711, -32.74022090983473987 ) ) ;
#1149 = ORIENTED_EDGE ( 'NONE', *, *, #12119, .F. ) ;
#1150 = EDGE_CURVE ( 'NONE', #26133, #24435, #22901, .T. ) ;
#1151 = CARTESIAN_POINT ( 'NONE',  ( -5.082228009654736312, -3.365126390422853220, -6.889929326000007848 ) ) ;
#1152 = ORIENTED_EDGE ( 'NONE', *, *, #20095, .T. ) ;
#1153 = CARTESIAN_POINT ( 'NONE',  ( -25.96688743241757535, 8.776138984008598598, 0.000000000000000000 ) ) ;
#1154 = CARTESIAN_POINT ( 'NONE',  ( -4.166989350266031344, 0.2041299532645725889, -68.10000000002500542 ) ) ;
#1155 = ORIENTED_EDGE ( 'NONE', *, *, #4608, .T. ) ;
#1156 = EDGE_LOOP ( 'NONE', ( #4268, #11999, #26019, #12570 ) ) ;
#1157 = ORIENTED_EDGE ( 'NONE', *, *, #15638, .T. ) ;
#1158 = CARTESIAN_POINT ( 'NONE',  ( 24.29812717139177636, -12.87956648213236832, 5.490554142100076085 ) ) ;
#1159 =( NAMED_UNIT ( * ) PLANE_ANGLE_UNIT ( ) SI_UNIT ( $, .RADIAN. ) );
#1160 = ORIENTED_EDGE ( 'NONE', *, *, #22690, .F. ) ;
#1161 = CARTESIAN_POINT ( 'NONE',  ( -8.903108651239966420, -22.82508830966961000, 140.0000000000000000 ) ) ;
#1162 = CARTESIAN_POINT ( 'NONE',  ( -12.29999999970000069, -27.00000000000000000, -28.40000000001083791 ) ) ;
#1163 = EDGE_CURVE ( 'NONE', #16579, #13261, #16538, .T. ) ;
#1164 = CARTESIAN_POINT ( 'NONE',  ( -4.469650141049659631, 2.071768678095493588, -65.02526299422498823 ) ) ;
#1165 = AXIS2_PLACEMENT_3D ( 'NONE', #23386, #2435, #6999 ) ;
#1166 = CARTESIAN_POINT ( 'NONE',  ( -10.69999999930000101, -24.87867965640000278, -30.52132034359999935 ) ) ;
#1167 = EDGE_CURVE ( 'NONE', #15899, #25472, #18720, .T. ) ;
#1168 = B_SPLINE_CURVE_WITH_KNOTS ( 'NONE', 3,
 ( #26996, #12366, #24485, #2922, #12515, #29350, #5435, #3071, #734, #10325, #29505, #7942, #17542, #4831, #22437, #15497, #3534, #22594, #3375, #12981, #25101, #3227, #13445, #8397 ),
 .UNSPECIFIED., .F., .F.,
 ( 4, 2, 2, 2, 2, 2, 2, 2, 2, 2, 2, 4 ),
 ( 0.000000000000000000, 0.001577043753785914524, 0.002365565630678863329, 0.003154087507571812134, 0.004731131261357737934, 0.005519653138250699316, 0.006308175015143660698, 0.007885218768929582595, 0.009462262522715505358, 0.01025078439960847021, 0.01103930627650143333, 0.01261635003028735783 ),
 .UNSPECIFIED. ) ;
#1169 = COLOUR_RGB ( '', 0.40784314, 0.44705882, 0.49803922) ;
#1170 = CARTESIAN_POINT ( 'NONE',  ( -24.73836043327892042, 13.50621019268970713, -0.5592437529999827461 ) ) ;
#1171 = DIRECTION ( 'NONE',  ( 0.000000000000000000, 0.000000000000000000, -1.000000000000000000 ) ) ;
#1172 = AXIS2_PLACEMENT_3D ( 'NONE', #21552, #13688, #21400 ) ;
#1173 = CARTESIAN_POINT ( 'NONE',  ( 3.389121577670000107, 11.55088360999999963, 224.6412452697800290 ) ) ;
#1174 = CARTESIAN_POINT ( 'NONE',  ( 0.000000000000000000, 0.000000000000000000, 227.6412452699999847 ) ) ;
#1175 = ORIENTED_EDGE ( 'NONE', *, *, #14244, .F. ) ;
#1176 = EDGE_CURVE ( 'NONE', #24619, #15474, #22131, .T. ) ;
#1177 = CARTESIAN_POINT ( 'NONE',  ( -0.7008090670319790938, 4.721317983490957992, -9.930220916600003278 ) ) ;
#1178 = CARTESIAN_POINT ( 'NONE',  ( 13.88844815065594496, 21.69999999930212198, -57.58022008509880862 ) ) ;
#1179 = CARTESIAN_POINT ( 'NONE',  ( 23.55411374389282386, 16.04538543799059980, 8.000000000000007105 ) ) ;
#1180 = ORIENTED_EDGE ( 'NONE', *, *, #1838, .T. ) ;
#1181 = DIRECTION ( 'NONE',  ( 0.9831920802501790124, -0.1715636151751586680, -0.06244404920691486172 ) ) ;
#1182 = CARTESIAN_POINT ( 'NONE',  ( -22.87891075612136760, -13.95728375031006685, 4.090187774257245223 ) ) ;
#1183 = CARTESIAN_POINT ( 'NONE',  ( -24.16679028379773797, -15.10730798416152609, 6.002747143000003227 ) ) ;
#1184 = CARTESIAN_POINT ( 'NONE',  ( 24.71356588429207690, 13.94368305229924232, 0.8585785770000020634 ) ) ;
#1185 = CARTESIAN_POINT ( 'NONE',  ( 10.32522729140000095, -24.73114799960000099, -1.399999999999998579 ) ) ;
#1186 = CARTESIAN_POINT ( 'NONE',  ( -0.06606756225350368661, 5.646037861211643083, -57.31818518972499277 ) ) ;
#1187 = ADVANCED_FACE ( 'NONE', ( #16518 ), #5026, .F. ) ;
#1188 = FACE_OUTER_BOUND ( 'NONE', #30134, .T. ) ;
#1189 = CARTESIAN_POINT ( 'NONE',  ( 22.63996212555145249, -14.34127312894895923, 224.8540320937674437 ) ) ;
#1190 = EDGE_LOOP ( 'NONE', ( #5983, #12137 ) ) ;
#1191 = CARTESIAN_POINT ( 'NONE',  ( -10.00000000024713742, -28.51085694111269575, -31.02135916506436430 ) ) ;
#1192 = DIRECTION ( 'NONE',  ( 1.000000000000000000, -9.219999999999999084E-13, 4.710999999999999616E-12 ) ) ;
#1193 = AXIS2_PLACEMENT_3D ( 'NONE', #12409, #5331, #2662 ) ;
#1194 = VECTOR ( 'NONE', #8324, 1000.000000000000000 ) ;
#1195 = AXIS2_PLACEMENT_3D ( 'NONE', #14636, #5486, #19510 ) ;
#1196 = CARTESIAN_POINT ( 'NONE',  ( -16.83342759582943060, -8.999999999996580513, -0.6999999999999784173 ) ) ;
#1197 = B_SPLINE_CURVE_WITH_KNOTS ( 'NONE', 3,
 ( #19881, #13084, #10731, #4703, #11053, #9258 ),
 .UNSPECIFIED., .F., .F.,
 ( 4, 2, 4 ),
 ( 0.000000000000000000, 0.5000000000000000000, 1.000000000000000000 ),
 .UNSPECIFIED. ) ;
#1198 = EDGE_CURVE ( 'NONE', #2707, #23086, #13529, .T. ) ;
#1199 = CARTESIAN_POINT ( 'NONE',  ( 10.00000000000000000, 21.72305290929948640, -60.97178489257708378 ) ) ;
#1200 = PRESENTATION_STYLE_ASSIGNMENT (( #17855 ) ) ;
#1201 = CARTESIAN_POINT ( 'NONE',  ( 14.72975346149532960, -25.75642680092629888, -33.45521746712941535 ) ) ;
#1202 = CARTESIAN_POINT ( 'NONE',  ( -10.97092057897609862, -24.67424207454737939, -1.714865362423650508 ) ) ;
#1203 = CARTESIAN_POINT ( 'NONE',  ( -3.750715812471464350, 4.529495762826656780, -63.79933298482499993 ) ) ;
#1204 = VERTEX_POINT ( 'NONE', #12261 ) ;
#1205 = CARTESIAN_POINT ( 'NONE',  ( 19.01242865374335267, 20.00033489853029778, 230.5035276049833044 ) ) ;
#1206 = EDGE_LOOP ( 'NONE', ( #7039, #213, #29911, #1121, #16764, #16573 ) ) ;
#1207 = CARTESIAN_POINT ( 'NONE',  ( 27.11703666554969416, -9.406552224315994692, 0.000000000000000000 ) ) ;
#1208 = ORIENTED_EDGE ( 'NONE', *, *, #5748, .F. ) ;
#1209 = AXIS2_PLACEMENT_3D ( 'NONE', #16925, #19297, #12205 ) ;
#1210 = AXIS2_PLACEMENT_3D ( 'NONE', #8253, #3381, #5296 ) ;
#1211 = CARTESIAN_POINT ( 'NONE',  ( 16.37473331889771089, 11.76353838340827984, -0.6999999999999784173 ) ) ;
#1212 = AXIS2_PLACEMENT_3D ( 'NONE', #26161, #16699, #18916 ) ;
#1213 = CARTESIAN_POINT ( 'NONE',  ( -12.29999999976166158, -29.62135916506277411, -29.91085694131270500 ) ) ;
#1214 = CARTESIAN_POINT ( 'NONE',  ( -15.75643827148868681, 10.73282780873525866, -0.6999999999999784173 ) ) ;
#1215 = AXIS2_PLACEMENT_3D ( 'NONE', #2118, #1815, #4167 ) ;
#1216 = CYLINDRICAL_SURFACE ( 'NONE', #11313, 3.000000000000005329 ) ;
#1217 = CARTESIAN_POINT ( 'NONE',  ( 25.46368747440213198, -12.80129684534102807, 5.104216618000034345 ) ) ;
#1218 = CYLINDRICAL_SURFACE ( 'NONE', #22576, 3.000000000000003997 ) ;
#1219 = ORIENTED_EDGE ( 'NONE', *, *, #2519, .F. ) ;
#1220 = CARTESIAN_POINT ( 'NONE',  ( 4.785280386522178020, 31.71089591180988876, 1.000000000000000888 ) ) ;
#1221 = LINE ( 'NONE', #1064, #2721 ) ;
#1222 = CARTESIAN_POINT ( 'NONE',  ( -2.837346519424604807, 2.085571669681350659, 230.8270369382007630 ) ) ;
#1223 = DIRECTION ( 'NONE',  ( 1.520059509754405802E-12, -0.4554456718803465698, -0.8902635789278700029 ) ) ;
#1224 = FACE_OUTER_BOUND ( 'NONE', #25517, .T. ) ;
#1225 = EDGE_CURVE ( 'NONE', #7840, #24939, #24789, .T. ) ;
#1226 = CARTESIAN_POINT ( 'NONE',  ( -9.993285220779425160, -25.61999708228226069, 136.3944487260000074 ) ) ;
#1227 = CARTESIAN_POINT ( 'NONE',  ( 4.101176313917073379, -1.931410228222276038, -51.89872167392500302 ) ) ;
#1228 = ADVANCED_FACE ( 'NONE', ( #4721 ), #23930, .F. ) ;
#1229 = LINE ( 'NONE', #17884, #20251 ) ;
#1230 = EDGE_CURVE ( 'NONE', #7767, #14785, #9674, .T. ) ;
#1231 = CARTESIAN_POINT ( 'NONE',  ( 9.484767271962898150, -25.06561782275612771, 204.0863404859320553 ) ) ;
#1232 = CARTESIAN_POINT ( 'NONE',  ( -20.01708959866950366, 19.99999743978112932, 229.8069797309569822 ) ) ;
#1233 = CARTESIAN_POINT ( 'NONE',  ( -24.90462872294775920, -9.900530325344874427, 43.21714158839293418 ) ) ;
#1234 = AXIS2_PLACEMENT_3D ( 'NONE', #16237, #4129, #16086 ) ;
#1235 = CIRCLE ( 'NONE', #17813, 6.000000000000001776 ) ;
#1236 = VECTOR ( 'NONE', #16768, 1000.000000000000000 ) ;
#1237 = CARTESIAN_POINT ( 'NONE',  ( 18.26639035967037827, -8.979988381807324060, -1.000005633855494125E-09 ) ) ;
#1238 = ORIENTED_EDGE ( 'NONE', *, *, #21745, .T. ) ;
#1239 = AXIS2_PLACEMENT_3D ( 'NONE', #10395, #13052, #5970 ) ;
#1240 = CARTESIAN_POINT ( 'NONE',  ( 4.437687981975763307, 3.340062028235890601, -33.36032172560000220 ) ) ;
#1241 = EDGE_LOOP ( 'NONE', ( #8778, #2335, #4602, #30893 ) ) ;
#1242 = DIRECTION ( 'NONE',  ( 0.000000000000000000, 0.000000000000000000, 1.000000000000000000 ) ) ;
#1243 = CARTESIAN_POINT ( 'NONE',  ( -4.185672079393978784, 2.483218523716627768, -50.83267869292499341 ) ) ;
#1244 = VERTEX_POINT ( 'NONE', #12847 ) ;
#1245 = APPLICATION_PROTOCOL_DEFINITION ( 'draft international standard', 'automotive_design', 1998, #18620 ) ;
#1246 = ORIENTED_EDGE ( 'NONE', *, *, #28669, .T. ) ;
#1247 = ORIENTED_EDGE ( 'NONE', *, *, #9957, .T. ) ;
#1248 = AXIS2_PLACEMENT_3D ( 'NONE', #26035, #21308, #6364 ) ;
#1249 = COLOUR_RGB ( '', 0.40784314, 0.44705882, 0.49803922) ;
#1250 = CARTESIAN_POINT ( 'NONE',  ( -17.64325308166371542, -9.745514112911177307, 0.000000000000000000 ) ) ;
#1251 = CARTESIAN_POINT ( 'NONE',  ( -0.04427422412647075145, -27.80047756270342063, 5.964026387038768640 ) ) ;
#1252 = CARTESIAN_POINT ( 'NONE',  ( 4.772623561773215783, 2.197494481170958913, -35.69999999999999574 ) ) ;
#1253 = FACE_OUTER_BOUND ( 'NONE', #18893, .T. ) ;
#1254 = DIRECTION ( 'NONE',  ( 1.000000000000000000, -1.224606353819999829E-16, 0.000000000000000000 ) ) ;
#1255 = CARTESIAN_POINT ( 'NONE',  ( -5.086464543762334145, -0.5886760371733784636, -0.6999999999999992895 ) ) ;
#1256 = CARTESIAN_POINT ( 'NONE',  ( 1.213582369797474136, 4.521795443253902924, -1.553410702900004825 ) ) ;
#1257 = AXIS2_PLACEMENT_3D ( 'NONE', #22632, #24529, #15386 ) ;
#1258 = CARTESIAN_POINT ( 'NONE',  ( -3.511528848185079266, -0.9178490657093262284, 227.7210190899423310 ) ) ;
#1259 = CARTESIAN_POINT ( 'NONE',  ( 25.46368747440757474, -12.80129684534242074, 5.147587687417541247 ) ) ;
#1260 = VECTOR ( 'NONE', #28010, 1000.000000000000000 ) ;
#1261 = CARTESIAN_POINT ( 'NONE',  ( -1.302427785971572716, -4.985450142227665360, -13.48772317839999602 ) ) ;
#1262 = CARTESIAN_POINT ( 'NONE',  ( -0.4155902256269943806, 5.929468065910143082, -33.89518930509999706 ) ) ;
#1263 = CARTESIAN_POINT ( 'NONE',  ( 0.1656472034149999717, -5.899424820049999241, 226.6412452697800006 ) ) ;
#1264 = DIRECTION ( 'NONE',  ( 0.3633921898465272138, -0.9316362575375356503, 1.850371707708593498E-14 ) ) ;
#1265 = CARTESIAN_POINT ( 'NONE',  ( 3.552713678799999608E-15, -3.552713678799999608E-15, 136.7828584120000244 ) ) ;
#1266 = CARTESIAN_POINT ( 'NONE',  ( 0.4821455018050000429, -28.49635764770000179, 226.0025203910000187 ) ) ;
#1267 = CARTESIAN_POINT ( 'NONE',  ( -3.538182117160495022, 0.8713469530890178838, 227.7293001947007269 ) ) ;
#1268 = CYLINDRICAL_SURFACE ( 'NONE', #30824, 1.099999999999999867 ) ;
#1269 = CARTESIAN_POINT ( 'NONE',  ( -10.00000000005000445, -14.23127763322419703, -74.05809100303530101 ) ) ;
#1270 = CARTESIAN_POINT ( 'NONE',  ( 0.2462945485190000117, -28.49939181899999951, 223.9202078600000050 ) ) ;
#1271 = ADVANCED_FACE ( 'NONE', ( #28635 ), #11802, .F. ) ;
#1272 = AXIS2_PLACEMENT_3D ( 'NONE', #3031, #29928, #8200 ) ;
#1273 = VERTEX_POINT ( 'NONE', #28778 ) ;
#1274 = ORIENTED_EDGE ( 'NONE', *, *, #21907, .T. ) ;
#1275 = CARTESIAN_POINT ( 'NONE',  ( 24.38199545065365115, 14.75707034588002564, 6.098654095000016540 ) ) ;
#1276 = CARTESIAN_POINT ( 'NONE',  ( -2.168672284410000206E-10, -27.14999999990000035, 0.000000000000000000 ) ) ;
#1277 = ORIENTED_EDGE ( 'NONE', *, *, #11164, .F. ) ;
#1278 = DIRECTION ( 'NONE',  ( 1.000000000000000000, 0.000000000000000000, 0.000000000000000000 ) ) ;
#1279 = CARTESIAN_POINT ( 'NONE',  ( -18.95046173579999760, -18.95046173579999760, -2.842170943039999687E-14 ) ) ;
#1280 = ORIENTED_EDGE ( 'NONE', *, *, #3659, .F. ) ;
#1281 = CARTESIAN_POINT ( 'NONE',  ( 6.000000000000000000, -17.74403716370463968, -75.33663091226621589 ) ) ;
#1282 = ORIENTED_EDGE ( 'NONE', *, *, #21795, .F. ) ;
#1283 = ORIENTED_EDGE ( 'NONE', *, *, #28659, .F. ) ;
#1284 = SURFACE_STYLE_USAGE ( .BOTH. , #7880 ) ;
#1285 = B_SPLINE_CURVE_WITH_KNOTS ( 'NONE', 1,
 ( #3231, #27001 ),
 .UNSPECIFIED., .F., .F.,
 ( 2, 2 ),
 ( -2.555885125540000124E-06, 0.7000000000009999335 ),
 .UNSPECIFIED. ) ;
#1286 = ORIENTED_EDGE ( 'NONE', *, *, #8341, .T. ) ;
#1287 = CARTESIAN_POINT ( 'NONE',  ( -1.087696845100000198, -27.77899371300000197, 224.7918862260000026 ) ) ;
#1288 = PRODUCT ( 'Front End Cap', 'Front End Cap', '', ( #16022 ) ) ;
#1289 = DIRECTION ( 'NONE',  ( 1.000000000000000000, -1.843431230200084908E-12, 2.650498504963248473E-12 ) ) ;
#1290 = VERTEX_POINT ( 'NONE', #7385 ) ;
#1291 = CARTESIAN_POINT ( 'NONE',  ( -24.63376349509220731, 12.88634507999193701, 5.901400367999992902 ) ) ;
#1292 = CARTESIAN_POINT ( 'NONE',  ( -2.845423091905608715, -4.282740972715254557, -93.71305981297928156 ) ) ;
#1293 = CARTESIAN_POINT ( 'NONE',  ( -8.000000000000000000, -17.74403716370463968, -75.33663091226621589 ) ) ;
#1294 = CARTESIAN_POINT ( 'NONE',  ( -23.26091398107482888, -13.42624119016083384, 0.000000000000000000 ) ) ;
#1295 = PRODUCT_DEFINITION_FORMATION_WITH_SPECIFIED_SOURCE ( 'ANY', '', #16179, .NOT_KNOWN. ) ;
#1296 = DIRECTION ( 'NONE',  ( -1.000000000000000000, 1.224606353819999829E-16, 0.000000000000000000 ) ) ;
#1297 = EDGE_CURVE ( 'NONE', #23190, #14788, #7235, .T. ) ;
#1298 = CARTESIAN_POINT ( 'NONE',  ( -2.507187057889194381, 3.594686560818127763, -1.627651354100000169 ) ) ;
#1299 = CARTESIAN_POINT ( 'NONE',  ( -5.151963982244392781, -3.152247574024123811, -21.90799200640000777 ) ) ;
#1300 = DIRECTION ( 'NONE',  ( -1.000000000000000000, 0.000000000000000000, 0.000000000000000000 ) ) ;
#1301 = CARTESIAN_POINT ( 'NONE',  ( 24.36724931188768650, 13.38201648792073684, 4.999998581000003384 ) ) ;
#1302 = CARTESIAN_POINT ( 'NONE',  ( -0.5564057544751848106, -3.564787113710755850, -88.52261276293012315 ) ) ;
#1303 = CARTESIAN_POINT ( 'NONE',  ( -24.15788560609999891, 13.40103774969999861, 230.6999999999999886 ) ) ;
#1304 = DIRECTION ( 'NONE',  ( 0.000000000000000000, 0.000000000000000000, -1.000000000000000000 ) ) ;
#1305 = CARTESIAN_POINT ( 'NONE',  ( 10.69999999995387086, -31.36650361035140477, -21.96235324005989753 ) ) ;
#1306 = CARTESIAN_POINT ( 'NONE',  ( 1.776356839399999804E-15, -5.329070518200000398E-15, 228.3912452697800006 ) ) ;
#1307 = CARTESIAN_POINT ( 'NONE',  ( 18.42247763970000207, -19.87503982779999845, 230.6999999999999886 ) ) ;
#1308 = CARTESIAN_POINT ( 'NONE',  ( 4.638804294843716036, -9.686171446567970023, -32.75490769819511172 ) ) ;
#1309 = EDGE_LOOP ( 'NONE', ( #18962, #2062, #1393, #5608, #28099, #12108, #20122, #17059, #7243, #25749, #28852, #21248 ) ) ;
#1310 = CARTESIAN_POINT ( 'NONE',  ( -4.178199994060139311, -1.098053884355550069, -56.05102360502500858 ) ) ;
#1311 = DIRECTION ( 'NONE',  ( -1.000000000000000000, 5.687698019341907056E-16, -6.771501495046482653E-12 ) ) ;
#1312 = VERTEX_POINT ( 'NONE', #14166 ) ;
#1313 = CARTESIAN_POINT ( 'NONE',  ( -3.057389860650357338, 5.459897439232808125, -16.67761783620000315 ) ) ;
#1314 = ORIENTED_EDGE ( 'NONE', *, *, #4200, .F. ) ;
#1315 = CARTESIAN_POINT ( 'NONE',  ( 26.80000000069999899, -3.281945028320000125E-15, 137.1101814800000227 ) ) ;
#1316 = FACE_OUTER_BOUND ( 'NONE', #18611, .T. ) ;
#1317 = ORIENTED_EDGE ( 'NONE', *, *, #28659, .T. ) ;
#1318 = DIRECTION ( 'NONE',  ( 0.000000000000000000, 0.000000000000000000, 1.000000000000000000 ) ) ;
#1319 = VERTEX_POINT ( 'NONE', #21878 ) ;
#1320 = ORIENTED_EDGE ( 'NONE', *, *, #24982, .T. ) ;
#1321 = CARTESIAN_POINT ( 'NONE',  ( -3.686970300939999667, -0.1862064327014488485, -68.94610314789107974 ) ) ;
#1322 = ORIENTED_EDGE ( 'NONE', *, *, #23592, .F. ) ;
#1323 = DIRECTION ( 'NONE',  ( 0.000000000000000000, 0.000000000000000000, -1.000000000000000000 ) ) ;
#1324 = CARTESIAN_POINT ( 'NONE',  ( 23.48807013373048491, -14.30280389787537842, 4.086914724217819206 ) ) ;
#1325 = CARTESIAN_POINT ( 'NONE',  ( 1.415268835064556363, -5.780081730213937341, -64.70397119102500483 ) ) ;
#1326 = ADVANCED_FACE ( 'NONE', ( #162, #324 ), #9277, .F. ) ;
#1327 = CARTESIAN_POINT ( 'NONE',  ( -23.10935684520000066, -20.42749692159999952, 229.1414198580000061 ) ) ;
#1328 = B_SPLINE_CURVE_WITH_KNOTS ( 'NONE', 3,
 ( #10500, #17710, #18187, #1213, #1368, #3401, #22303, #20101, #15370, #24967, #6075, #20239, #13005, #8423, #20558, #29837, #8272, #27472 ),
 .UNSPECIFIED., .F., .F.,
 ( 4, 2, 2, 2, 2, 2, 2, 2, 4 ),
 ( 0.000000000000000000, 0.1249999999999997224, 0.2499999999999994449, 0.3749999999999991673, 0.4999999999999993339, 0.6249999999999994449, 0.7499999999999996669, 0.8749999999999997780, 1.000000000000000000 ),
 .UNSPECIFIED. ) ;
#1329 = CARTESIAN_POINT ( 'NONE',  ( -10.00000000057842087, -23.99999999999979394, -28.79269908169899495 ) ) ;
#1330 = LINE ( 'NONE', #25245, #14054 ) ;
#1331 = CARTESIAN_POINT ( 'NONE',  ( 8.699999999994835420, -111.9817663798902885, 5.760339591779549018 ) ) ;
#1332 = ADVANCED_FACE ( 'NONE', ( #18883 ), #6663, .T. ) ;
#1333 = CYLINDRICAL_SURFACE ( 'NONE', #5437, 1.099999999999999867 ) ;
#1334 = EDGE_LOOP ( 'NONE', ( #21837, #26282, #22665, #4141 ) ) ;
#1335 = CARTESIAN_POINT ( 'NONE',  ( 1.483810035143914297, 4.536549859444123811, -10.13297964829999565 ) ) ;
#1336 = CARTESIAN_POINT ( 'NONE',  ( -4.000000000000000000, -29.27600094726834712, -81.66227801707495360 ) ) ;
#1337 = CARTESIAN_POINT ( 'NONE',  ( 19.80537707610000098, 19.50874960790000046, 229.0739602739999725 ) ) ;
#1338 = EDGE_LOOP ( 'NONE', ( #8212, #25635, #5309, #8348 ) ) ;
#1339 = CARTESIAN_POINT ( 'NONE',  ( 24.71695093370000151, -14.18891100779999981, 223.9013457789999961 ) ) ;
#1340 = CARTESIAN_POINT ( 'NONE',  ( 18.95046173579999760, -18.95046173579999760, 115.0000000000000000 ) ) ;
#1341 = DIRECTION ( 'NONE',  ( 0.000000000000000000, 0.000000000000000000, -1.000000000000000000 ) ) ;
#1342 = CARTESIAN_POINT ( 'NONE',  ( 18.50495734104858414, 20.74627095498905049, 0.8585787200000027930 ) ) ;
#1343 = CARTESIAN_POINT ( 'NONE',  ( 24.34663841809999951, -12.78636765230000094, 225.0000000000000000 ) ) ;
#1344 = CARTESIAN_POINT ( 'NONE',  ( 4.432674687120906398, 4.607520344841867121, -48.69426496242499525 ) ) ;
#1345 = CARTESIAN_POINT ( 'NONE',  ( -11.62710820939999934, -24.17108566160000294, -1.401657795899999392 ) ) ;
#1346 = DIRECTION ( 'NONE',  ( -9.868649108069999529E-17, -2.257145581549999994E-12, -1.000000000000000000 ) ) ;
#1347 = VERTEX_POINT ( 'NONE', #9746 ) ;
#1348 = EDGE_CURVE ( 'NONE', #7041, #9481, #16146, .T. ) ;
#1349 = CARTESIAN_POINT ( 'NONE',  ( 24.09407739349445876, -13.86899051613567480, 3.997190862000010725 ) ) ;
#1350 = CARTESIAN_POINT ( 'NONE',  ( 26.95545381250000361, 8.667969360499998999, 227.5999999999999943 ) ) ;
#1351 = EDGE_CURVE ( 'NONE', #5093, #30733, #10522, .T. ) ;
#1352 = APPLICATION_CONTEXT ( 'automotive_design' ) ;
#1353 = CARTESIAN_POINT ( 'NONE',  ( 1.503739165058197713, -3.819987766133262408, -68.10000000002500542 ) ) ;
#1354 = VECTOR ( 'NONE', #6354, 1000.000000000000000 ) ;
#1355 = CARTESIAN_POINT ( 'NONE',  ( 26.19759702725205486, 6.104572563141537955, -0.6999999999999784173 ) ) ;
#1356 = CARTESIAN_POINT ( 'NONE',  ( -4.246782972018593227, 0.8972508281424985688, -44.10000000002499831 ) ) ;
#1357 =( NAMED_UNIT ( * ) PLANE_ANGLE_UNIT ( ) SI_UNIT ( $, .RADIAN. ) );
#1358 = FACE_OUTER_BOUND ( 'NONE', #16961, .T. ) ;
#1359 = CARTESIAN_POINT ( 'NONE',  ( -18.95046173579999760, -18.95046173579999760, 115.0000000000000000 ) ) ;
#1360 = CARTESIAN_POINT ( 'NONE',  ( 5.258991878263315378, 0.1257858540645254708, -64.81686508972499894 ) ) ;
#1361 = ORIENTED_EDGE ( 'NONE', *, *, #16817, .F. ) ;
#1362 = CARTESIAN_POINT ( 'NONE',  ( 18.77987097257140903, 20.00007305761831589, 230.5773074074296005 ) ) ;
#1363 = ORIENTED_EDGE ( 'NONE', *, *, #22710, .F. ) ;
#1365 = ADVANCED_FACE ( 'NONE', ( #1358 ), #15662, .T. ) ;
#1364 = CARTESIAN_POINT ( 'NONE',  ( -20.24759346773182855, -21.13259110598446355, 0.7069231350000093617 ) ) ;
#1366 = VERTEX_POINT ( 'NONE', #18174 ) ;
#1367 = CARTESIAN_POINT ( 'NONE',  ( -23.25311087902445450, -15.23597700045494996, 4.689445057000002137 ) ) ;
#1368 = CARTESIAN_POINT ( 'NONE',  ( -12.29999999977708214, -29.39900052719453782, -30.24364016012474465 ) ) ;
#1369 = CARTESIAN_POINT ( 'NONE',  ( 2.635643612059070051, 2.346759556412466363, 0.000000000000000000 ) ) ;
#1370 = B_SPLINE_CURVE_WITH_KNOTS ( 'NONE', 3,
 ( #653, #3728, #17314, #26919, #19984, #11129, #26759, #24707, #25292, #6250 ),
 .UNSPECIFIED., .F., .F.,
 ( 4, 2, 2, 2, 4 ),
 ( 0.000000000000000000, 0.2500000000000000000, 0.5000000000000000000, 0.7500000000000000000, 1.000000000000000000 ),
 .UNSPECIFIED. ) ;
#1371 = CARTESIAN_POINT ( 'NONE',  ( 18.26261577949329151, 11.17152825599126054, -1.400000000000001910 ) ) ;
#1372 = CARTESIAN_POINT ( 'NONE',  ( -6.982632971260604116, 4.357143524085962838, -42.94209588230350505 ) ) ;
#1373 = FACE_OUTER_BOUND ( 'NONE', #9906, .T. ) ;
#1374 = EDGE_LOOP ( 'NONE', ( #18092, #3792, #29449, #21165 ) ) ;
#1375 = CARTESIAN_POINT ( 'NONE',  ( 10.14902473071748368, -26.01926976409366077, 87.93968498540000667 ) ) ;
#1376 = LINE ( 'NONE', #30160, #4251 ) ;
#1377 = EDGE_CURVE ( 'NONE', #21922, #24619, #143, .T. ) ;
#1378 = CARTESIAN_POINT ( 'NONE',  ( -8.000000000000000000, -15.86465192213301556, -74.65259062561435144 ) ) ;
#1379 = AXIS2_PLACEMENT_3D ( 'NONE', #11886, #4345, #16139 ) ;
#1380 = CARTESIAN_POINT ( 'NONE',  ( -3.542173841662227485, 0.8647749370036884597, 230.7522105547303966 ) ) ;
#1381 = CARTESIAN_POINT ( 'NONE',  ( -24.10559463919999956, -15.20494734660000091, 225.2084356629999888 ) ) ;
#1382 = FACE_OUTER_BOUND ( 'NONE', #9321, .T. ) ;
#1383 = CIRCLE ( 'NONE', #7898, 27.50000000000000000 ) ;
#1384 = CARTESIAN_POINT ( 'NONE',  ( 17.16657240419154462, 10.99999999996915179, -0.6999999999999784173 ) ) ;
#1385 = CARTESIAN_POINT ( 'NONE',  ( -15.76765990785340676, -8.693620616903867671, -0.6999999999999785283 ) ) ;
#1386 = CARTESIAN_POINT ( 'NONE',  ( -0.7556487780321456960, 4.453147011089717111, -50.85792092402500231 ) ) ;
#1387 = FACE_OUTER_BOUND ( 'NONE', #57, .T. ) ;
#1388 = EDGE_CURVE ( 'NONE', #28481, #19078, #8148, .T. ) ;
#1389 = CARTESIAN_POINT ( 'NONE',  ( 9.689803781819819051, -24.98716455116954549, 203.0573596598972017 ) ) ;
#1390 = CARTESIAN_POINT ( 'NONE',  ( -20.12793915297035952, 19.99999059665350387, 229.6434139119940312 ) ) ;
#1391 = CARTESIAN_POINT ( 'NONE',  ( -17.37135892817496696, 10.02943855699536613, -0.000000000000000000 ) ) ;
#1392 = LINE ( 'NONE', #16015, #6709 ) ;
#1393 = ORIENTED_EDGE ( 'NONE', *, *, #31039, .F. ) ;
#1395 = B_SPLINE_CURVE_WITH_KNOTS ( 'NONE', 5,
 ( #25094, #24937, #3063, #15177, #6041, #22267 ),
 .UNSPECIFIED., .F., .F.,
 ( 6, 6 ),
 ( -2.319814960280000005, 0.000000000000000000 ),
 .UNSPECIFIED. ) ;
#1394 = CARTESIAN_POINT ( 'NONE',  ( -0.3280975466111886174, 4.681158999438242319, -35.39518930510001127 ) ) ;
#1396 = ORIENTED_EDGE ( 'NONE', *, *, #18688, .T. ) ;
#1397 = CARTESIAN_POINT ( 'NONE',  ( -5.649653782182448403, -1.974543963569185046, -50.88743646232499884 ) ) ;
#1398 = EDGE_LOOP ( 'NONE', ( #8843, #21305, #25039, #18047 ) ) ;
#1399 = AXIS2_PLACEMENT_3D ( 'NONE', #949, #20134, #22648 ) ;
#1400 = APPLICATION_PROTOCOL_DEFINITION ( 'draft international standard', 'automotive_design', 1998, #24645 ) ;
#1401 = ORIENTED_EDGE ( 'NONE', *, *, #2120, .F. ) ;
#1402 = AXIS2_PLACEMENT_3D ( 'NONE', #24745, #14997, #2153 ) ;
#1404 = ADVANCED_FACE ( 'NONE', ( #13306 ), #27776, .F. ) ;
#1403 = AXIS2_PLACEMENT_3D ( 'NONE', #15802, #3679, #8082 ) ;
#1405 = ORIENTED_EDGE ( 'NONE', *, *, #3637, .F. ) ;
#1406 = CARTESIAN_POINT ( 'NONE',  ( -17.92646393081800582, -9.131743399318690280, 0.000000000000000000 ) ) ;
#1407 = FACE_OUTER_BOUND ( 'NONE', #15137, .T. ) ;
#1408 = CARTESIAN_POINT ( 'NONE',  ( 7.105427357599999217E-15, 3.552713678799999608E-15, 93.60555127549999099 ) ) ;
#1409 = ADVANCED_FACE ( 'NONE', ( #1519 ), #10951, .F. ) ;
#1410 = DIRECTION ( 'NONE',  ( 0.000000000000000000, 0.000000000000000000, 1.000000000000000000 ) ) ;
#1411 = CARTESIAN_POINT ( 'NONE',  ( -1.033595436889999888E-13, -27.50000000069999828, 3.899999999999999911 ) ) ;
#1412 = CARTESIAN_POINT ( 'NONE',  ( -3.444986276472465470, -4.029727111321103727, -0.6999999999999992895 ) ) ;
#1413 = CARTESIAN_POINT ( 'NONE',  ( -4.325159770583743679, -1.744232581393518666, -0.4971974345000021445 ) ) ;
#1414 = CARTESIAN_POINT ( 'NONE',  ( 1.949119511211575118, 0.5206197137392853946, 230.8412452700000301 ) ) ;
#1415 = FACE_OUTER_BOUND ( 'NONE', #27203, .T. ) ;
#1416 = EDGE_CURVE ( 'NONE', #27427, #6530, #20546, .T. ) ;
#1417 = CARTESIAN_POINT ( 'NONE',  ( 0.9833222185976336904, 5.418310215658684648, -15.02400681850000019 ) ) ;
#1418 = CARTESIAN_POINT ( 'NONE',  ( 5.672553144689285176, -0.9485505809898806540, -35.14517599850000806 ) ) ;
#1419 = CARTESIAN_POINT ( 'NONE',  ( 5.799375405969999342, 1.094484689620000006, 226.6412452697800006 ) ) ;
#1420 = CARTESIAN_POINT ( 'NONE',  ( -8.999999999699999975, 21.34999999950001026, -70.09999999999999432 ) ) ;
#1421 = CARTESIAN_POINT ( 'NONE',  ( 10.46446609389999871, 20.99999999999999645, -54.63553390589999736 ) ) ;
#1422 = CARTESIAN_POINT ( 'NONE',  ( -14.55829176637774935, -23.98013756361786974, 8.000000000000007105 ) ) ;
#1423 = DIRECTION ( 'NONE',  ( -1.000000000000000000, 0.000000000000000000, 0.000000000000000000 ) ) ;
#1424 = CARTESIAN_POINT ( 'NONE',  ( 20.30405755279999980, 20.00000000000000000, 227.3999999149999951 ) ) ;
#1425 = FACE_OUTER_BOUND ( 'NONE', #16091, .T. ) ;
#1426 = CARTESIAN_POINT ( 'NONE',  ( 0.1319790757220171973, -27.80015609199433158, 3.957670871000018575 ) ) ;
#1427 = VECTOR ( 'NONE', #9255, 1000.000000000000000 ) ;
#1428 = ORIENTED_EDGE ( 'NONE', *, *, #28444, .T. ) ;
#1429 = EDGE_LOOP ( 'NONE', ( #7369, #15757, #8978, #15625 ) ) ;
#1430 = CARTESIAN_POINT ( 'NONE',  ( 23.87963657767028280, 15.55698410313905988, 5.506989593000027661 ) ) ;
#1431 = DIRECTION ( 'NONE',  ( 1.000000000000000000, -1.224606353820000075E-16, 0.000000000000000000 ) ) ;
#1432 = EDGE_LOOP ( 'NONE', ( #299, #9426, #4454, #14051 ) ) ;
#1433 = CARTESIAN_POINT ( 'NONE',  ( -22.70120178296838986, -14.24511786445138206, 224.5052107108826647 ) ) ;
#1434 = CARTESIAN_POINT ( 'NONE',  ( -24.55564696219999732, -13.03410599059999875, 224.4928762930000232 ) ) ;
#1435 = CARTESIAN_POINT ( 'NONE',  ( 0.8466631608419120658, -26.78674355063222734, 4.296357544259503669 ) ) ;
#1436 = EDGE_LOOP ( 'NONE', ( #19200, #25509, #1669, #15010, #4840, #15096, #3053, #26439, #4768, #7960 ) ) ;
#1437 = CARTESIAN_POINT ( 'NONE',  ( -9.738910687886987105, -24.96785170200594095, 143.2171415880000040 ) ) ;
#1438 = ORIENTED_EDGE ( 'NONE', *, *, #28112, .T. ) ;
#1439 = EDGE_LOOP ( 'NONE', ( #11897, #21831, #3160, #7996 ) ) ;
#1440 = CIRCLE ( 'NONE', #9974, 10.00000000000000355 ) ;
#1441 = ORIENTED_EDGE ( 'NONE', *, *, #10698, .F. ) ;
#1442 = CARTESIAN_POINT ( 'NONE',  ( -3.552713678799999608E-15, -3.552713678799999608E-15, 141.6604601749999972 ) ) ;
#1443 = EDGE_CURVE ( 'NONE', #12111, #5252, #1887, .T. ) ;
#1444 = EDGE_LOOP ( 'NONE', ( #2096, #20345, #12000, #15130 ) ) ;
#1445 = CIRCLE ( 'NONE', #16504, 2.100000000000000089 ) ;
#1446 = CARTESIAN_POINT ( 'NONE',  ( -8.699999998997657968, -25.77531388886905006, -25.66136093486021608 ) ) ;
#1447 = DIRECTION ( 'NONE',  ( 0.8775825618903718706, -0.4794255386042047262, 0.000000000000000000 ) ) ;
#1448 = CARTESIAN_POINT ( 'NONE',  ( 1.212514609374590213, 3.905384712586410068, -35.69999999999998863 ) ) ;
#1449 = EDGE_CURVE ( 'NONE', #11197, #15367, #17700, .T. ) ;
#1450 = CARTESIAN_POINT ( 'NONE',  ( -4.870417428126710746, 6.462009008221302864, -40.63090155203821752 ) ) ;
#1451 = VECTOR ( 'NONE', #7899, 1000.000000000000114 ) ;
#1452 = ADVANCED_FACE ( 'NONE', ( #5755 ), #12994, .F. ) ;
#1453 = CARTESIAN_POINT ( 'NONE',  ( 9.944225187684267553, -25.63929276476995156, 203.0591393848753512 ) ) ;
#1454 = CARTESIAN_POINT ( 'NONE',  ( -21.30588112097817088, -16.35227051405537679, -0.000000000000000000 ) ) ;
#1455 = CARTESIAN_POINT ( 'NONE',  ( -0.2462327729630000017, -28.49941772390000239, 226.0797932899999978 ) ) ;
#1456 = EDGE_LOOP ( 'NONE', ( #28511, #8580, #30468, #16902, #27099, #12265, #27129, #24342 ) ) ;
#1457 = CARTESIAN_POINT ( 'NONE',  ( 3.691964249065762260, -4.599677940684276933, -4.105321867100004241 ) ) ;
#1458 = CARTESIAN_POINT ( 'NONE',  ( -0.4514894588696777289, 4.335480228600245844, -25.88903409329999761 ) ) ;
#1459 = CARTESIAN_POINT ( 'NONE',  ( -5.420768140797359358, -26.96154273974103077, 209.3135392056180706 ) ) ;
#1460 = B_SPLINE_CURVE_WITH_KNOTS ( 'NONE', 3,
 ( #24696, #12889, #8581, #3131, #3879, #3285 ),
 .UNSPECIFIED., .F., .F.,
 ( 4, 2, 4 ),
 ( 0.000000000000000000, 0.5000000000000000000, 1.000000000000000000 ),
 .UNSPECIFIED. ) ;
#1461 = CARTESIAN_POINT ( 'NONE',  ( -26.80000000000000071, -8.704148513059999178E-14, 230.6999999999999886 ) ) ;
#1462 = FACE_OUTER_BOUND ( 'NONE', #30891, .T. ) ;
#1463 = CARTESIAN_POINT ( 'NONE',  ( -27.56257419730000180, -2.228452907019999617E-14, 230.5592437530000041 ) ) ;
#1464 = CARTESIAN_POINT ( 'NONE',  ( 0.4193002349296617859, -0.2844359550551249782, -98.16700801147769084 ) ) ;
#1465 = DIRECTION ( 'NONE',  ( 0.000000000000000000, 0.000000000000000000, -1.000000000000000000 ) ) ;
#1466 = CIRCLE ( 'NONE', #5956, 0.9999999999999981126 ) ;
#1467 = CARTESIAN_POINT ( 'NONE',  ( -23.10935684540000068, -20.42749692129999772, 222.0000000000000000 ) ) ;
#1468 = CARTESIAN_POINT ( 'NONE',  ( 26.80000000069999899, -1.877389046380000037, 230.6999999999999886 ) ) ;
#1469 = CARTESIAN_POINT ( 'NONE',  ( 6.127633414585145211, -7.367024628712027123, -33.88603117893229921 ) ) ;
#1470 = VERTEX_POINT ( 'NONE', #25114 ) ;
#1471 = CARTESIAN_POINT ( 'NONE',  ( -1.157762119782732135, -5.359362766143966006, -55.13033560642499253 ) ) ;
#1472 = DIRECTION ( 'NONE',  ( 0.000000000000000000, 0.3420201433259318913, -0.9396926207858126157 ) ) ;
#1473 = VERTEX_POINT ( 'NONE', #3548 ) ;
#1474 = CARTESIAN_POINT ( 'NONE',  ( 6.105340317929710992, -0.2107885888489036130, -2.685409721200002320 ) ) ;
#1475 = VERTEX_POINT ( 'NONE', #25437 ) ;
#1476 = CARTESIAN_POINT ( 'NONE',  ( 10.00000000020000002, -25.00000000000000000, -2.400000000399998612 ) ) ;
#1477 = AXIS2_PLACEMENT_3D ( 'NONE', #30131, #20218, #29810 ) ;
#1478 = CYLINDRICAL_SURFACE ( 'NONE', #29859, 3.000000000000002220 ) ;
#1479 = ORIENTED_EDGE ( 'NONE', *, *, #30200, .F. ) ;
#1480 = DIRECTION ( 'NONE',  ( 3.134067079931429195E-12, 0.3568421334038983650, -0.9341647027306021478 ) ) ;
#1481 = ORIENTED_EDGE ( 'NONE', *, *, #24442, .T. ) ;
#1482 = EDGE_CURVE ( 'NONE', #3709, #30998, #2661, .T. ) ;
#1483 = ORIENTED_EDGE ( 'NONE', *, *, #9638, .T. ) ;
#1484 = CARTESIAN_POINT ( 'NONE',  ( -23.25788685383076881, -13.43083806724688500, 186.7828584123333826 ) ) ;
#1485 =( LENGTH_UNIT ( ) NAMED_UNIT ( * ) SI_UNIT ( .MILLI., .METRE. ) );
#1486 = ORIENTED_EDGE ( 'NONE', *, *, #27163, .T. ) ;
#1487 = CARTESIAN_POINT ( 'NONE',  ( 9.999999999979998222, -127.2537437101000108, -34.36317024011000143 ) ) ;
#1488 = CARTESIAN_POINT ( 'NONE',  ( 1.484924240490000047, -1.484924240490000047, 226.6412452697800006 ) ) ;
#1489 = LINE ( 'NONE', #4922, #26302 ) ;
#1490 = CARTESIAN_POINT ( 'NONE',  ( 5.229687933750000184, -30.84198039029999805, 229.1414219810000077 ) ) ;
#1491 = DIRECTION ( 'NONE',  ( 0.4999999999969509945, -0.4151946956549595336, -0.7600087925169251024 ) ) ;
#1492 = CARTESIAN_POINT ( 'NONE',  ( -17.46645031549676830, -23.90523224175912631, -24.41319780928835925 ) ) ;
#1493 = VERTEX_POINT ( 'NONE', #13937 ) ;
#1494 = CARTESIAN_POINT ( 'NONE',  ( -25.25401215124432852, 13.21081861195569296, 4.098596794000014754 ) ) ;
#1495 = VECTOR ( 'NONE', #9365, 1000.000000000000000 ) ;
#1496 = AXIS2_PLACEMENT_3D ( 'NONE', #1293, #13078, #29613 ) ;
#1497 = CARTESIAN_POINT ( 'NONE',  ( 3.212457031643341399, -4.530353719951508928, -11.12388893670000378 ) ) ;
#1498 = CARTESIAN_POINT ( 'NONE',  ( 25.43121960300669215, -8.635379644106567554, 136.7828584120000244 ) ) ;
#1499 = CARTESIAN_POINT ( 'NONE',  ( -10.69999999967832949, -27.41951581582461372, -31.60007023061346842 ) ) ;
#1500 = ORIENTED_EDGE ( 'NONE', *, *, #28250, .F. ) ;
#1501 = CARTESIAN_POINT ( 'NONE',  ( -10.69999999996760742, -30.00000000000001421, -28.04899130767095983 ) ) ;
#1502 = CYLINDRICAL_SURFACE ( 'NONE', #243, 26.80000000000002203 ) ;
#1503 = CARTESIAN_POINT ( 'NONE',  ( -2.299991308520000465E-10, 21.69999999990000106, -70.09999999999999432 ) ) ;
#1504 = CARTESIAN_POINT ( 'NONE',  ( 18.32611613475859258, 20.54576746904009710, 0.2686742950000209351 ) ) ;
#1505 = DIRECTION ( 'NONE',  ( 1.000000000000000000, 0.000000000000000000, 0.000000000000000000 ) ) ;
#1506 = CLOSED_SHELL ( 'NONE', ( #15794, #6412, #1752, #1409 ) ) ;
#1507 = CARTESIAN_POINT ( 'NONE',  ( -5.212126283948660621, -2.851000302232811201, -53.34982952342500084 ) ) ;
#1508 = CARTESIAN_POINT ( 'NONE',  ( -11.63809019400000011, -24.14124255240000139, -0.6999999999999992895 ) ) ;
#1509 = CYLINDRICAL_SURFACE ( 'NONE', #21807, 2.500000000000000888 ) ;
#1510 = ORIENTED_EDGE ( 'NONE', *, *, #2441, .T. ) ;
#1511 = EDGE_CURVE ( 'NONE', #24890, #28814, #18024, .T. ) ;
#1512 = DIRECTION ( 'NONE',  ( -3.924189347185963153E-12, 0.4082287037029530552, 0.9128796883888953273 ) ) ;
#1513 = CARTESIAN_POINT ( 'NONE',  ( -26.05511412830000140, 14.93229958979999950, 222.0000000000000000 ) ) ;
#1514 = EDGE_CURVE ( 'NONE', #5941, #3457, #12030, .T. ) ;
#1515 = CARTESIAN_POINT ( 'NONE',  ( 2.341423236568627164, -3.556873072008999159, -68.10000000002500542 ) ) ;
#1516 = EDGE_CURVE ( 'NONE', #28644, #30907, #1985, .T. ) ;
#1517 = CARTESIAN_POINT ( 'NONE',  ( 1.070547230664766758, 2.553693132251782405, -67.94886126136832161 ) ) ;
#1518 = CARTESIAN_POINT ( 'NONE',  ( -2.794029045709408354, -2.766466238262267119, -44.10000000002498410 ) ) ;
#1519 = FACE_OUTER_BOUND ( 'NONE', #22369, .T. ) ;
#1520 = DIRECTION ( 'NONE',  ( -0.000000000000000000, -0.000000000000000000, -1.000000000000000000 ) ) ;
#1521 = CARTESIAN_POINT ( 'NONE',  ( -4.150389416700803302, 1.923785201099231790, -65.77526299422500244 ) ) ;
#1522 = VERTEX_POINT ( 'NONE', #12607 ) ;
#1523 = CARTESIAN_POINT ( 'NONE',  ( 19.58403526555239793, 20.00013581975909815, 230.2127468032437889 ) ) ;
#1524 = EDGE_LOOP ( 'NONE', ( #22834, #29814, #9317, #26166 ) ) ;
#1525 = CARTESIAN_POINT ( 'NONE',  ( -24.64719444845753671, -14.72745526642161451, 0.08279798700003282441 ) ) ;
#1526 = VERTEX_POINT ( 'NONE', #5375 ) ;
#1527 = CARTESIAN_POINT ( 'NONE',  ( -11.32877539260000077, -24.28840542069999842, -0.7339858089999984347 ) ) ;
#1528 = EDGE_CURVE ( 'NONE', #24268, #24784, #17639, .T. ) ;
#1529 = CARTESIAN_POINT ( 'NONE',  ( -26.93395402219999824, 3.298349122909999612E-15, 187.7567592740000180 ) ) ;
#1530 = CARTESIAN_POINT ( 'NONE',  ( 8.000000000281330514, -5.981227587277713198, -27.94042817480428198 ) ) ;
#1531 = LINE ( 'NONE', #30484, #20482 ) ;
#1532 = CARTESIAN_POINT ( 'NONE',  ( -0.4969045691571343237, -28.49594262166996828, 4.493528488000025689 ) ) ;
#1533 = CARTESIAN_POINT ( 'NONE',  ( 8.000000000000000000, -15.86465192213301556, -74.65259062561435144 ) ) ;
#1534 = FACE_OUTER_BOUND ( 'NONE', #20098, .T. ) ;
#1535 = EDGE_CURVE ( 'NONE', #13631, #11921, #27089, .T. ) ;
#1536 = VERTEX_POINT ( 'NONE', #26055 ) ;
#1537 = CARTESIAN_POINT ( 'NONE',  ( 0.4314002833255045632, -3.971307163432137077, -44.10000000002498410 ) ) ;
#1538 = CARTESIAN_POINT ( 'NONE',  ( -8.699999999715409160, -23.99014701217026513, -28.09041065100222312 ) ) ;
#1539 = DIRECTION ( 'NONE',  ( -1.000000000000000000, 5.687697913153403713E-16, -6.771501495041734442E-12 ) ) ;
#1540 = DIRECTION ( 'NONE',  ( 0.000000000000000000, 0.000000000000000000, 1.000000000000000000 ) ) ;
#1541 = CARTESIAN_POINT ( 'NONE',  ( -7.999999999712662735, -24.01208138055985941, -28.87597782795289802 ) ) ;
#1542 = PLANE ( 'NONE',  #10003 ) ;
#1543 = APPLICATION_CONTEXT ( 'automotive_design' ) ;
#1544 = CARTESIAN_POINT ( 'NONE',  ( -0.5569265645694643219, -27.49469370722579242, 225.9595466040883878 ) ) ;
#1545 = CIRCLE ( 'NONE', #4053, 6.000000000000001776 ) ;
#1546 = CARTESIAN_POINT ( 'NONE',  ( 7.999999999977091214, -107.4273096626279482, 14.66297538114749344 ) ) ;
#1547 = CARTESIAN_POINT ( 'NONE',  ( -4.320323480314926634, -1.509945384023519965, -50.00743646232500339 ) ) ;
#1548 = CARTESIAN_POINT ( 'NONE',  ( -23.56630063302987921, -14.17280417044578655, 5.994883229690994852 ) ) ;
#1549 = CARTESIAN_POINT ( 'NONE',  ( -17.59696597919420213, 10.20816091468181774, 0.000000000000000000 ) ) ;
#1550 = CARTESIAN_POINT ( 'NONE',  ( 17.95841148948556310, 10.23646161652002817, -0.6999999999999784173 ) ) ;
#1551 = B_SPLINE_CURVE_WITH_KNOTS ( 'NONE', 3,
 ( #19893, #12485, #396, #24610, #20036, #5403, #7910, #29163, #15157, #22098, #7610, #7761, #2743, #10594 ),
 .UNSPECIFIED., .F., .F.,
 ( 4, 2, 2, 1, 1, 2, 2, 4 ),
 ( 0.000000000000000000, 0.2500000000000100475, 0.3750000000000123790, 0.4375000000000153211, 0.4687500000000160427, 0.4843750000000174305, 0.5000000000000187628, 1.000000000000000000 ),
 .UNSPECIFIED. ) ;
#1552 = EDGE_CURVE ( 'NONE', #23036, #12853, #28911, .T. ) ;
#1553 = CARTESIAN_POINT ( 'NONE',  ( -1.100000000000000311, -27.47799119299999759, 224.9035402883650647 ) ) ;
#1554 = PRESENTATION_LAYER_ASSIGNMENT (  '', '', ( #20635 ) ) ;
#1555 = ORIENTED_EDGE ( 'NONE', *, *, #14905, .T. ) ;
#1556 = CARTESIAN_POINT ( 'NONE',  ( 2.022420680230021972, -3.847796821814266632, -33.20721934060000535 ) ) ;
#1557 = VERTEX_POINT ( 'NONE', #11725 ) ;
#1558 = CARTESIAN_POINT ( 'NONE',  ( -4.890954027203302523, -0.1236851485102684334, -54.30673954922499291 ) ) ;
#1559 = ORIENTED_EDGE ( 'NONE', *, *, #28153, .F. ) ;
#1560 = APPLICATION_PROTOCOL_DEFINITION ( 'draft international standard', 'automotive_design', 1998, #12597 ) ;
#1561 = ORIENTED_EDGE ( 'NONE', *, *, #20981, .T. ) ;
#1562 = EDGE_LOOP ( 'NONE', ( #10993, #30576, #17167, #18297 ) ) ;
#1563 = EDGE_CURVE ( 'NONE', #7142, #20367, #26643, .T. ) ;
#1564 = CARTESIAN_POINT ( 'NONE',  ( -8.699999999681903518, -14.92844969908904851, -33.25053330396269047 ) ) ;
#1565 = CARTESIAN_POINT ( 'NONE',  ( -0.1620084139599508588, -27.79990535609617197, 5.886603267324479027 ) ) ;
#1566 = CARTESIAN_POINT ( 'NONE',  ( -17.47972357343302363, -29.97921655931956764, -24.34654879079820233 ) ) ;
#1567 = EDGE_CURVE ( 'NONE', #13375, #14059, #30931, .T. ) ;
#1568 = CIRCLE ( 'NONE', #4075, 27.49999999619999969 ) ;
#1569 = DIRECTION ( 'NONE',  ( -0.3633921898465274913, 0.9316362575375356503, 0.000000000000000000 ) ) ;
#1570 = CARTESIAN_POINT ( 'NONE',  ( 8.000000000232340369, -25.77531388888444752, -25.66136093478154123 ) ) ;
#1571 = DIRECTION ( 'NONE',  ( 0.000000000000000000, 0.000000000000000000, -1.000000000000000000 ) ) ;
#1572 = CARTESIAN_POINT ( 'NONE',  ( -3.673964118181757943, -4.849481262180703744, -3.728945369300004753 ) ) ;
#1573 = CARTESIAN_POINT ( 'NONE',  ( 11.00000000000000000, 26.42151601322854759, -59.26168417594741555 ) ) ;
#1574 = CARTESIAN_POINT ( 'NONE',  ( 11.20000000009999930, -27.00000000000000355, -22.62649730800000114 ) ) ;
#1575 = ADVANCED_FACE ( 'NONE', ( #17176 ), #5217, .T. ) ;
#1576 = CARTESIAN_POINT ( 'NONE',  ( 1.102985302404366097, 4.375751030832064181, -17.98830441500000177 ) ) ;
#1577 = CARTESIAN_POINT ( 'NONE',  ( -4.773116892509256637, 0.6906165796890335606, -33.32033976330000513 ) ) ;
#1578 = CARTESIAN_POINT ( 'NONE',  ( -12.77820031409999935, 20.99999999999999645, -56.09999999999999432 ) ) ;
#1579 = CARTESIAN_POINT ( 'NONE',  ( -3.907985046680000082E-14, -26.80000000000000071, 6.099999999630000502 ) ) ;
#1580 = CARTESIAN_POINT ( 'NONE',  ( -19.06860189597471944, 19.69237645765742073, 0.2003674019999956979 ) ) ;
#1581 = CARTESIAN_POINT ( 'NONE',  ( 25.74138181328865826, -11.15269228347309038, 8.000000000000007105 ) ) ;
#1582 = CARTESIAN_POINT ( 'NONE',  ( -3.521608956067899587, 0.9000755979543652030, 227.7241098089399713 ) ) ;
#1583 = CARTESIAN_POINT ( 'NONE',  ( -23.23277431133845994, -15.26692929363520257, 4.999998581000003384 ) ) ;
#1584 = CARTESIAN_POINT ( 'NONE',  ( 2.749352377422821903, -2.213834474264458230, 226.6412452697750837 ) ) ;
#1585 = CARTESIAN_POINT ( 'NONE',  ( 18.28639557936419280, 10.97998838177520931, 0.05106179917585291356 ) ) ;
#1586 = EDGE_CURVE ( 'NONE', #22430, #26248, #13128, .T. ) ;
#1587 = CARTESIAN_POINT ( 'NONE',  ( -27.92857142909999979, 3.420150602519999655E-15, 42.06031501480000401 ) ) ;
#1588 = CIRCLE ( 'NONE', #28218, 27.50000000000000000 ) ;
#1589 = ORIENTED_EDGE ( 'NONE', *, *, #8530, .T. ) ;
#1590 = CARTESIAN_POINT ( 'NONE',  ( 1.275182700919280654, -3.500000000000000444, 227.7673180537732947 ) ) ;
#1591 = FACE_OUTER_BOUND ( 'NONE', #20842, .T. ) ;
#1592 = CARTESIAN_POINT ( 'NONE',  ( 9.999999999958726349, -35.47767383584782408, -24.90806880973072879 ) ) ;
#1593 = VERTEX_POINT ( 'NONE', #5679 ) ;
#1594 = CARTESIAN_POINT ( 'NONE',  ( 0.5498575204270217398, -4.501552459765377101, -43.78057807742499818 ) ) ;
#1595 = ORIENTED_EDGE ( 'NONE', *, *, #1972, .F. ) ;
#1596 = EDGE_CURVE ( 'NONE', #6530, #7809, #10987, .T. ) ;
#1597 = EDGE_LOOP ( 'NONE', ( #9088, #27743, #23180, #6425 ) ) ;
#1598 = VERTEX_POINT ( 'NONE', #1437 ) ;
#1599 = CARTESIAN_POINT ( 'NONE',  ( -6.999999999262594308, -5.572998883415898774, -27.02754848611273530 ) ) ;
#1600 = ORIENTED_EDGE ( 'NONE', *, *, #17500, .F. ) ;
#1601 = CARTESIAN_POINT ( 'NONE',  ( -25.17394274020000111, -13.36230406159999973, 225.5071265450000055 ) ) ;
#1602 = CARTESIAN_POINT ( 'NONE',  ( 8.000000000836740455, -15.37655846826601014, -33.05014450755139421 ) ) ;
#1603 = CARTESIAN_POINT ( 'NONE',  ( -3.414938295376681587, -3.730152739507092363, -94.17120874162482380 ) ) ;
#1604 = LINE ( 'NONE', #20794, #16956 ) ;
#1605 = CARTESIAN_POINT ( 'NONE',  ( 5.160560622299999345, 6.288231966779999738, 227.7662452697800006 ) ) ;
#1606 = CARTESIAN_POINT ( 'NONE',  ( -1.127665019380000189, -28.47796022459999676, 225.0000014190000002 ) ) ;
#1607 = VERTEX_POINT ( 'NONE', #10712 ) ;
#1608 = VECTOR ( 'NONE', #14619, 1000.000000000000114 ) ;
#1609 = CARTESIAN_POINT ( 'NONE',  ( 5.763395275750641922, -2.111988417859953504, -5.836105321700000736 ) ) ;
#1610 = CARTESIAN_POINT ( 'NONE',  ( -2.496099253731141943, 5.577352528212363048, -22.73780126169999605 ) ) ;
#1611 = CARTESIAN_POINT ( 'NONE',  ( 10.89131017139999891, -24.73114799890000270, -1.811764705899998606 ) ) ;
#1612 = CARTESIAN_POINT ( 'NONE',  ( 24.71695093370000151, -14.18891100779999981, 223.9013457789999961 ) ) ;
#1613 = DIRECTION ( 'NONE',  ( 1.000000000000000000, 0.000000000000000000, 0.000000000000000000 ) ) ;
#1614 = DIRECTION ( 'NONE',  ( 0.7198537139083028835, -0.6941258031311204890, 0.000000000000000000 ) ) ;
#1615 = CARTESIAN_POINT ( 'NONE',  ( -24.62906106470000012, -14.34164290000000008, 226.0959707279999975 ) ) ;
#1616 = B_SPLINE_CURVE_WITH_KNOTS ( 'NONE', 1,
 ( #9249, #23599 ),
 .UNSPECIFIED., .F., .F.,
 ( 2, 2 ),
 ( -2.557302930970000000E-06, 0.7000000000009999335 ),
 .UNSPECIFIED. ) ;
#1617 = LINE ( 'NONE', #20810, #27270 ) ;
#1618 = CARTESIAN_POINT ( 'NONE',  ( 9.315522638039999137, 15.62494945029999904, 230.6999999999999886 ) ) ;
#1619 = CARTESIAN_POINT ( 'NONE',  ( -17.72558663072204155, 11.65945330601512175, -0.6999999999999783062 ) ) ;
#1620 = EDGE_CURVE ( 'NONE', #6179, #13261, #23694, .T. ) ;
#1621 = ORIENTED_EDGE ( 'NONE', *, *, #22367, .F. ) ;
#1622 = CARTESIAN_POINT ( 'NONE',  ( 1.387947292976095426, 4.364053279572889465, -60.06492395752500357 ) ) ;
#1623 = FACE_OUTER_BOUND ( 'NONE', #6376, .T. ) ;
#1624 = EDGE_LOOP ( 'NONE', ( #12461, #24851, #2719, #20904 ) ) ;
#1625 = EDGE_CURVE ( 'NONE', #3626, #8936, #3622, .T. ) ;
#1626 = CARTESIAN_POINT ( 'NONE',  ( 28.49999999990000177, 3.413935693800000060, 222.0000000000000000 ) ) ;
#1627 = CARTESIAN_POINT ( 'NONE',  ( 5.195105410215491659, 3.969764343816663210, -23.36727430110000014 ) ) ;
#1628 = ORIENTED_EDGE ( 'NONE', *, *, #2753, .F. ) ;
#1629 = EDGE_CURVE ( 'NONE', #3949, #4546, #9480, .T. ) ;
#1630 = CARTESIAN_POINT ( 'NONE',  ( -24.87138426050000106, -13.91768300640000078, 226.0425107039999943 ) ) ;
#1631 = CARTESIAN_POINT ( 'NONE',  ( -3.842035491633269739, -1.137847961864614899, -68.10000000002500542 ) ) ;
#1632 = EDGE_CURVE ( 'NONE', #30700, #30026, #3779, .T. ) ;
#1633 = EDGE_LOOP ( 'NONE', ( #13346, #45, #30897, #13735, #27902 ) ) ;
#1634 = VERTEX_POINT ( 'NONE', #27695 ) ;
#1635 = VERTEX_POINT ( 'NONE', #20464 ) ;
#1636 = CARTESIAN_POINT ( 'NONE',  ( 3.556846951432204751, 0.09270462095633093258, -91.35798291625272327 ) ) ;
#1637 = EDGE_LOOP ( 'NONE', ( #5645, #24469, #17522, #7195 ) ) ;
#1638 = CARTESIAN_POINT ( 'NONE',  ( 8.699999999564820286, -13.66682223739023350, -36.55330428411032528 ) ) ;
#1639 = DIRECTION ( 'NONE',  ( 0.3633921898465273803, -0.9316362575375355393, -1.387778780781445044E-14 ) ) ;
#1640 = B_SPLINE_CURVE_WITH_KNOTS ( 'NONE', 1,
 ( #22386, #24898 ),
 .UNSPECIFIED., .F., .F.,
 ( 2, 2 ),
 ( -9.355471259890000464E-07, 0.7003637394550000783 ),
 .UNSPECIFIED. ) ;
#1641 = CARTESIAN_POINT ( 'NONE',  ( -4.287590041606506475, 1.413705153860729924, -68.34019511502499711 ) ) ;
#1642 = CARTESIAN_POINT ( 'NONE',  ( 5.068184391690000012, -29.88946390619999960, 230.0000000000000000 ) ) ;
#1643 = CARTESIAN_POINT ( 'NONE',  ( -0.9560301558052189952, -26.78297054395609322, 224.4510318449164004 ) ) ;
#1645 = VECTOR ( 'NONE', #4875, 1000.000000000000000 ) ;
#1644 = CARTESIAN_POINT ( 'NONE',  ( -18.43841600009999837, -21.14227905559999954, 222.0000000000000000 ) ) ;
#1646 = CARTESIAN_POINT ( 'NONE',  ( 8.699999999979134202, -115.7892272573602668, 9.034522711534439310 ) ) ;
#1647 = VERTEX_POINT ( 'NONE', #27238 ) ;
#1648 = FACE_OUTER_BOUND ( 'NONE', #26090, .T. ) ;
#1649 = CARTESIAN_POINT ( 'NONE',  ( 6.482330152203070739, 0.4632910120546396282, -14.64454535870000207 ) ) ;
#1650 = DIRECTION ( 'NONE',  ( -1.000000000000000000, 5.687697993419811493E-16, -6.771501495049272772E-12 ) ) ;
#1651 = CARTESIAN_POINT ( 'NONE',  ( -10.69999999968267090, -28.96604956106295603, -30.95933451744668830 ) ) ;
#1652 = AXIS2_PLACEMENT_3D ( 'NONE', #7185, #14277, #21357 ) ;
#1653 = ORIENTED_EDGE ( 'NONE', *, *, #4274, .T. ) ;
#1654 = CARTESIAN_POINT ( 'NONE',  ( 20.84977244261583706, 16.87341063695685150, -1.399999999999998357 ) ) ;
#1655 = DIRECTION ( 'NONE',  ( 2.257102469710000208E-12, 0.000000000000000000, 1.000000000000000000 ) ) ;
#1656 = CARTESIAN_POINT ( 'NONE',  ( -9.000000000000000000, 19.99999999999999645, -44.10000000000000142 ) ) ;
#1657 = CARTESIAN_POINT ( 'NONE',  ( 26.79556473285982321, 0.4875557887249727385, 0.000000000000000000 ) ) ;
#1658 = CARTESIAN_POINT ( 'NONE',  ( -13.46485713443429511, 20.99999999997146105, -56.74255209446624093 ) ) ;
#1659 = CARTESIAN_POINT ( 'NONE',  ( -4.251243323665415907, -4.132078999800212316, -47.20083066912499703 ) ) ;
#1660 = CARTESIAN_POINT ( 'NONE',  ( -23.76534794678204321, -14.42397063190348483, 6.095965061000018892 ) ) ;
#1661 = CARTESIAN_POINT ( 'NONE',  ( 8.000000000050000892, -13.98526668056139144, -73.96855033896248699 ) ) ;
#1662 = ORIENTED_EDGE ( 'NONE', *, *, #19198, .F. ) ;
#1663 = CARTESIAN_POINT ( 'NONE',  ( 9.993285220779439371, -25.61999708228226069, 27.99999999999999645 ) ) ;
#1664 = CARTESIAN_POINT ( 'NONE',  ( -17.83930458849792089, 19.99999999999597478, -1.000005633855494125E-09 ) ) ;
#1665 = CARTESIAN_POINT ( 'NONE',  ( 2.288615330823977168, -3.575176636938152352, -68.10000000002500542 ) ) ;
#1666 = EDGE_CURVE ( 'NONE', #17343, #27013, #22991, .T. ) ;
#1667 = CARTESIAN_POINT ( 'NONE',  ( 3.046043134278133557, -1.783682052637085125, -0.6999999999999784173 ) ) ;
#1668 = CARTESIAN_POINT ( 'NONE',  ( -4.184103756552774556, 0.3543491974005151812, -44.10000000002499121 ) ) ;
#1669 = ORIENTED_EDGE ( 'NONE', *, *, #31035, .T. ) ;
#1670 = CARTESIAN_POINT ( 'NONE',  ( 2.476206779668751246, 3.511840374477381843, -39.19200816759646955 ) ) ;
#1671 = AXIS2_PLACEMENT_3D ( 'NONE', #6906, #26120, #28627 ) ;
#1672 = CARTESIAN_POINT ( 'NONE',  ( 4.434603606053169500, 2.142645224031550555, -67.60315453642500927 ) ) ;
#1673 = EDGE_LOOP ( 'NONE', ( #15667, #2741, #7837, #6105 ) ) ;
#1674 = CARTESIAN_POINT ( 'NONE',  ( 24.77037083723135780, -12.62110030509766645, 4.441416311653765270 ) ) ;
#1675 = ORIENTED_EDGE ( 'NONE', *, *, #19444, .T. ) ;
#1676 = CARTESIAN_POINT ( 'NONE',  ( -18.31101975560000028, 19.88193351600000014, 229.9783743860000129 ) ) ;
#1677 = VERTEX_POINT ( 'NONE', #1281 ) ;
#1678 = CARTESIAN_POINT ( 'NONE',  ( -1.630907768819999992, -5.558498092260000689, 226.6412452697800006 ) ) ;
#1679 = EDGE_CURVE ( 'NONE', #23122, #20967, #8493, .T. ) ;
#1680 =( LENGTH_UNIT ( ) NAMED_UNIT ( * ) SI_UNIT ( .MILLI., .METRE. ) );
#1681 = CARTESIAN_POINT ( 'NONE',  ( 9.760738032020000787, 19.99999999999999645, -43.05080462335000391 ) ) ;
#1682 = DIRECTION ( 'NONE',  ( 0.000000000000000000, 0.000000000000000000, -1.000000000000000000 ) ) ;
#1683 = CARTESIAN_POINT ( 'NONE',  ( 0.5057536231481327693, -27.79562098839016571, 3.899998581000013509 ) ) ;
#1684 = CARTESIAN_POINT ( 'NONE',  ( -16.09019580745308176, -9.813945847455975979, 0.000000000000000000 ) ) ;
#1685 = CARTESIAN_POINT ( 'NONE',  ( -9.999999999959999997, -29.06671945329999929, -26.22544931050000017 ) ) ;
#1686 = ORIENTED_EDGE ( 'NONE', *, *, #20758, .T. ) ;
#1687 = FACE_BOUND ( 'NONE', #30689, .T. ) ;
#1688 = CARTESIAN_POINT ( 'NONE',  ( 27.51770821245201759, 4.728187301810311105, 8.000000000000007105 ) ) ;
#1690 = EDGE_CURVE ( 'NONE', #12603, #12725, #19535, .T. ) ;
#1689 = CONICAL_SURFACE ( 'NONE', #23821, 3.491271820449999286, 1.047197551199999799 ) ;
#1691 = CARTESIAN_POINT ( 'NONE',  ( 1.379841223609999723, 12.21656123380000025, 232.6627643349999914 ) ) ;
#1692 = CARTESIAN_POINT ( 'NONE',  ( -1.776356839399999804E-15, -1.776356839399999804E-15, 230.0000000000000000 ) ) ;
#1693 = DIRECTION ( 'NONE',  ( 0.3326278240906416217, 0.000000000000000000, 0.9430581798811381589 ) ) ;
#1694 = DIRECTION ( 'NONE',  ( 0.000000000000000000, 0.3420201433259318358, -0.9396926207858125046 ) ) ;
#1695 = CARTESIAN_POINT ( 'NONE',  ( -1.317578093351431834, 0.7169295418041747858, 231.6412452697749984 ) ) ;
#1696 = FACE_BOUND ( 'NONE', #18455, .T. ) ;
#1697 = CARTESIAN_POINT ( 'NONE',  ( 1.423503787547387933, 4.651298240777052229, -50.71125421252500587 ) ) ;
#1698 = CARTESIAN_POINT ( 'NONE',  ( 27.08859402333790101, 0.4928875713652651203, 0.02487529600000981667 ) ) ;
#1699 = CARTESIAN_POINT ( 'NONE',  ( -6.661312627754254478, -7.245008774417666331, -33.94554228739334434 ) ) ;
#1700 = CARTESIAN_POINT ( 'NONE',  ( 0.000000000000000000, 21.70000000000000284, -44.10000000017312516 ) ) ;
#1701 = FACE_OUTER_BOUND ( 'NONE', #27105, .T. ) ;
#1702 = ORIENTED_EDGE ( 'NONE', *, *, #26033, .F. ) ;
#1703 = CARTESIAN_POINT ( 'NONE',  ( -23.62732472759999780, -14.64974168890000072, 224.3191706570000292 ) ) ;
#1704 = CIRCLE ( 'NONE', #21365, 4.175165894169885483 ) ;
#1705 = ORIENTED_EDGE ( 'NONE', *, *, #20203, .F. ) ;
#1706 = ADVANCED_FACE ( 'NONE', ( #20781 ), #26066, .F. ) ;
#1707 = CARTESIAN_POINT ( 'NONE',  ( 2.964344385329936937, 3.936232207905868030, -55.37619010302499589 ) ) ;
#1708 = AXIS2_PLACEMENT_3D ( 'NONE', #30537, #18565, #30994 ) ;
#1709 = VERTEX_POINT ( 'NONE', #28014 ) ;
#1710 = CIRCLE ( 'NONE', #5716, 2.000000000000000000 ) ;
#1711 = APPLICATION_PROTOCOL_DEFINITION ( 'draft international standard', 'automotive_design', 1998, #6954 ) ;
#1712 = AXIS2_PLACEMENT_3D ( 'NONE', #10527, #1242, #20425 ) ;
#1713 = ORIENTED_EDGE ( 'NONE', *, *, #10777, .F. ) ;
#1714 = VECTOR ( 'NONE', #9605, 1000.000000000000000 ) ;
#1715 = PLANE ( 'NONE',  #24649 ) ;
#1716 = ORIENTED_EDGE ( 'NONE', *, *, #13633, .F. ) ;
#1717 = CARTESIAN_POINT ( 'NONE',  ( 14.83997978847363619, -29.88586221491316053, -24.29280345199157054 ) ) ;
#1718 = DIRECTION ( 'NONE',  ( 0.000000000000000000, 0.000000000000000000, 1.000000000000000000 ) ) ;
#1719 = CARTESIAN_POINT ( 'NONE',  ( -17.31982526421591828, -31.07774283049385033, -24.98078322917286442 ) ) ;
#1720 = CARTESIAN_POINT ( 'NONE',  ( -20.30396346370000060, 20.00000000000000000, 227.0000000000000000 ) ) ;
#1721 = DIRECTION ( 'NONE',  ( 0.000000000000000000, 0.000000000000000000, 1.000000000000000000 ) ) ;
#1722 = CARTESIAN_POINT ( 'NONE',  ( 2.914708617673689606, -3.631324690002112110, -2.605321867100001132 ) ) ;
#1723 = CARTESIAN_POINT ( 'NONE',  ( 20.08301454169999900, -20.21156784769999959, 230.6999999999999886 ) ) ;
#1724 = ORIENTED_EDGE ( 'NONE', *, *, #1020, .T. ) ;
#1725 = LINE ( 'NONE', #21080, #29557 ) ;
#1726 = EDGE_CURVE ( 'NONE', #125, #7204, #1445, .T. ) ;
#1727 = CARTESIAN_POINT ( 'NONE',  ( -5.295622588438499534, 1.541709225419852780, -17.30443125760000456 ) ) ;
#1728 = CARTESIAN_POINT ( 'NONE',  ( 4.978085835933289793, 6.462009008182098668, -40.63090155201910392 ) ) ;
#1729 = B_SPLINE_CURVE_WITH_KNOTS ( 'NONE', 3,
 ( #3155, #17170, #5061, #26934, #19388, #7722 ),
 .UNSPECIFIED., .F., .F.,
 ( 4, 2, 4 ),
 ( 0.000000000000000000, 0.5000000000000000000, 1.000000000000000000 ),
 .UNSPECIFIED. ) ;
#1730 = CIRCLE ( 'NONE', #7253, 26.80000000000000071 ) ;
#1731 = CARTESIAN_POINT ( 'NONE',  ( 27.55801272791059731, 0.5014288284349825986, -0.5592437529999827461 ) ) ;
#1732 = CARTESIAN_POINT ( 'NONE',  ( 0.3737937747629999641, -27.79795631750000240, 223.9576737099999946 ) ) ;
#1733 =( GEOMETRIC_REPRESENTATION_CONTEXT ( 3 ) GLOBAL_UNCERTAINTY_ASSIGNED_CONTEXT ( ( #11892 ) ) GLOBAL_UNIT_ASSIGNED_CONTEXT ( ( #10483, #15192, #15352 ) ) REPRESENTATION_CONTEXT ( 'NONE', 'WORKASPACE' ) );
#1734 = CARTESIAN_POINT ( 'NONE',  ( -28.34732274966954790, -3.134629491153491987, 8.000000000000007105 ) ) ;
#1735 = CARTESIAN_POINT ( 'NONE',  ( -2.208189912596424609, 3.175302878607322743, 227.8506595042306060 ) ) ;
#1736 = AXIS2_PLACEMENT_3D ( 'NONE', #9220, #16004, #14272 ) ;
#1737 = VECTOR ( 'NONE', #728, 1000.000000000000000 ) ;
#1738 = CARTESIAN_POINT ( 'NONE',  ( 7.614137047270383540, -5.654631194664418992, -27.21009439270542885 ) ) ;
#1739 = CARTESIAN_POINT ( 'NONE',  ( -2.947640775130000104E-14, -27.50000000000000000, 226.0999999999999943 ) ) ;
#1740 = CARTESIAN_POINT ( 'NONE',  ( -0.5944614571882205212, -27.79380703160649446, 4.895947184000021046 ) ) ;
#1741 = EDGE_CURVE ( 'NONE', #17533, #18378, #27065, .T. ) ;
#1742 = EDGE_CURVE ( 'NONE', #10713, #24430, #2938, .T. ) ;
#1743 = CARTESIAN_POINT ( 'NONE',  ( 2.400053023253180040, 2.842866040618700296, 230.7188131565947629 ) ) ;
#1744 = ORIENTED_EDGE ( 'NONE', *, *, #15831, .F. ) ;
#1745 = CARTESIAN_POINT ( 'NONE',  ( 0.1546076948666131046, -3.500000000000000000, 227.6466545571240943 ) ) ;
#1746 = CARTESIAN_POINT ( 'NONE',  ( 1.850829058368556268, -2.615810859427025736, -36.20335296945545167 ) ) ;
#1747 = CARTESIAN_POINT ( 'NONE',  ( -1.074316293124689015, -5.123231133482405220, -0.7000242870099097070 ) ) ;
#1748 = VERTEX_POINT ( 'NONE', #6457 ) ;
#1749 = DIRECTION ( 'NONE',  ( 1.000000000000000000, 0.000000000000000000, 0.000000000000000000 ) ) ;
#1750 = VERTEX_POINT ( 'NONE', #23623 ) ;
#1751 = ORIENTED_EDGE ( 'NONE', *, *, #13656, .F. ) ;
#1752 = ADVANCED_FACE ( 'NONE', ( #14018 ), #21373, .T. ) ;
#1753 =( NAMED_UNIT ( * ) PLANE_ANGLE_UNIT ( ) SI_UNIT ( $, .RADIAN. ) );
#1754 = ORIENTED_EDGE ( 'NONE', *, *, #30180, .F. ) ;
#1755 = CYLINDRICAL_SURFACE ( 'NONE', #5919, 1.000000000000000666 ) ;
#1756 = CIRCLE ( 'NONE', #8768, 4.000000004070001225 ) ;
#1757 = VERTEX_POINT ( 'NONE', #23702 ) ;
#1759 = CARTESIAN_POINT ( 'NONE',  ( -25.08454981450000076, -13.52946590100000179, 225.7602695480000250 ) ) ;
#1758 = AXIS2_PLACEMENT_3D ( 'NONE', #6175, #1472, #20659 ) ;
#1760 = SURFACE_STYLE_USAGE ( .BOTH. , #16069 ) ;
#1761 = CARTESIAN_POINT ( 'NONE',  ( -24.29089620838935204, -14.90695587844356673, 3.920145809000019632 ) ) ;
#1762 = CARTESIAN_POINT ( 'NONE',  ( -9.999999999959999997, -29.06671945329999929, -26.22544931050000017 ) ) ;
#1763 = CARTESIAN_POINT ( 'NONE',  ( -0.3076636919694037964, -28.49867017228337573, 4.240370246000018994 ) ) ;
#1764 = EDGE_CURVE ( 'NONE', #30855, #1904, #14298, .T. ) ;
#1765 = CARTESIAN_POINT ( 'NONE',  ( 18.89227650605998932, -19.04064001868236389, -1.399999999999998801 ) ) ;
#1766 = CARTESIAN_POINT ( 'NONE',  ( 2.256478611577762194, -3.091664398557809168, 227.8316576175172656 ) ) ;
#1767 = CARTESIAN_POINT ( 'NONE',  ( -26.80000000069999899, 3.281945028329999726E-15, 43.21714158909999526 ) ) ;
#1768 = ORIENTED_EDGE ( 'NONE', *, *, #496, .F. ) ;
#1769 = CARTESIAN_POINT ( 'NONE',  ( -4.646804529178781173, -0.2974863596997279203, -4.148838774900000637 ) ) ;
#1770 = CARTESIAN_POINT ( 'NONE',  ( -1.961220842241857554, 4.382205557890588743, -21.80030126170000315 ) ) ;
#1771 = CARTESIAN_POINT ( 'NONE',  ( -8.566424601805399774, -26.13212873426111926, 206.6925145176014098 ) ) ;
#1772 = AXIS2_PLACEMENT_3D ( 'NONE', #11123, #11436, #18818 ) ;
#1773 = FACE_BOUND ( 'NONE', #1786, .T. ) ;
#1774 = CARTESIAN_POINT ( 'NONE',  ( 0.7992118188004544432, 3.499831230570420004, 227.6979960600617119 ) ) ;
#1775 = CARTESIAN_POINT ( 'NONE',  ( -24.84642331740000287, 12.90500083959999955, 222.0000000000000000 ) ) ;
#1776 = LINE ( 'NONE', #16234, #8698 ) ;
#1777 = EDGE_CURVE ( 'NONE', #23829, #25431, #8605, .T. ) ;
#1778 = DIRECTION ( 'NONE',  ( -0.7071067811869131692, -0.6918940811759506371, -0.1458855045341028167 ) ) ;
#1779 = CARTESIAN_POINT ( 'NONE',  ( 0.8794532062938354988, -27.78659480101258694, 6.042323509000024906 ) ) ;
#1780 = CARTESIAN_POINT ( 'NONE',  ( -10.82908725742657019, -27.76276047461853835, 193.2171415880000040 ) ) ;
#1781 = ORIENTED_EDGE ( 'NONE', *, *, #21395, .F. ) ;
#1782 = CARTESIAN_POINT ( 'NONE',  ( 1.815007998551255941, 5.706838904126064094, -59.98492395752499817 ) ) ;
#1783 = CARTESIAN_POINT ( 'NONE',  ( -23.83437493864195389, -15.62616283475966661, 5.290530235267004500 ) ) ;
#1784 = ORIENTED_EDGE ( 'NONE', *, *, #11351, .T. ) ;
#1785 = AXIS2_PLACEMENT_3D ( 'NONE', #27160, #27614, #10632 ) ;
#1786 = EDGE_LOOP ( 'NONE', ( #12509, #4725, #14097, #22822, #2263, #20982, #11767, #26636 ) ) ;
#1787 = DIRECTION ( 'NONE',  ( 1.000000000000000000, -9.219999999999999084E-13, 4.710999999999999616E-12 ) ) ;
#1788 = CARTESIAN_POINT ( 'NONE',  ( 5.307277461536620500, -2.951504967841703131, -26.93037294500000201 ) ) ;
#1789 = ORIENTED_EDGE ( 'NONE', *, *, #16604, .F. ) ;
#1790 = CARTESIAN_POINT ( 'NONE',  ( -25.22658730140000216, -13.26242337740000110, 225.0000014190000002 ) ) ;
#1791 = LINE ( 'NONE', #25394, #9769 ) ;
#1792 = ORIENTED_EDGE ( 'NONE', *, *, #3920, .T. ) ;
#1793 = ORIENTED_EDGE ( 'NONE', *, *, #25948, .F. ) ;
#1794 = ORIENTED_EDGE ( 'NONE', *, *, #22467, .T. ) ;
#1795 = DIRECTION ( 'NONE',  ( 0.2815395311429191860, 0.9595496299847263710, 0.000000000000000000 ) ) ;
#1796 = EDGE_LOOP ( 'NONE', ( #5260, #1320, #4571, #30312 ) ) ;
#1797 = CARTESIAN_POINT ( 'NONE',  ( -12.29999999999139781, -26.16240677005030335, -31.51671256534945087 ) ) ;
#1798 = AXIS2_PLACEMENT_3D ( 'NONE', #6774, #24229, #2671 ) ;
#1799 = CARTESIAN_POINT ( 'NONE',  ( 27.79539923781684507, 0.5057481689249235801, 8.000000000000007105 ) ) ;
#1800 = CARTESIAN_POINT ( 'NONE',  ( -4.155524648305278568, -2.455537445457761869, -68.32382590962500046 ) ) ;
#1801 = CARTESIAN_POINT ( 'NONE',  ( 27.71720220710000149, -7.261079543219999266, 229.4485730569999760 ) ) ;
#1802 = B_SPLINE_CURVE_WITH_KNOTS ( 'NONE', 5,
 ( #3037, #26961, #3189, #22093, #5248, #3338 ),
 .UNSPECIFIED., .F., .F.,
 ( 6, 6 ),
 ( 0.000000000000000000, 2.319815199919999849 ),
 .UNSPECIFIED. ) ;
#1803 = CARTESIAN_POINT ( 'NONE',  ( 1.127732790480000080, -28.47784299079999926, 225.0000014190000002 ) ) ;
#1804 = EDGE_CURVE ( 'NONE', #13930, #18290, #10758, .T. ) ;
#1805 = DIRECTION ( 'NONE',  ( 0.000000000000000000, -1.000000000000000000, 0.000000000000000000 ) ) ;
#1806 = CARTESIAN_POINT ( 'NONE',  ( -23.73992238019999945, -12.43607998449999918, 5.000000000000000000 ) ) ;
#1807 = ORIENTED_EDGE ( 'NONE', *, *, #18680, .F. ) ;
#1808 = CARTESIAN_POINT ( 'NONE',  ( -22.75759213010913484, -14.15424219528663130, 225.6766013745738348 ) ) ;
#1809 = EDGE_CURVE ( 'NONE', #6144, #22416, #15167, .T. ) ;
#1810 = CARTESIAN_POINT ( 'NONE',  ( -1.302427785971572716, -4.985450142227665360, -11.61272317840000312 ) ) ;
#1811 = CARTESIAN_POINT ( 'NONE',  ( -13.67718144140000014, 21.70000000000000284, -57.16242377749999548 ) ) ;
#1812 = CARTESIAN_POINT ( 'NONE',  ( 9.961462855526637128, 7.265485266898056516, 232.6627635728646908 ) ) ;
#1813 = ORIENTED_EDGE ( 'NONE', *, *, #30225, .F. ) ;
#1814 = CARTESIAN_POINT ( 'NONE',  ( -9.738910687886855655, -24.96785170200598714, 27.99999999999999645 ) ) ;
#1815 = DIRECTION ( 'NONE',  ( 1.000000000000000000, -6.668066630619518976E-24, -2.257150022442225012E-12 ) ) ;
#1816 = FACE_OUTER_BOUND ( 'NONE', #5552, .T. ) ;
#1817 = CARTESIAN_POINT ( 'NONE',  ( 1.115119965759999943, -28.47834310740000063, 225.2081038119999903 ) ) ;
#1818 = CARTESIAN_POINT ( 'NONE',  ( 11.19633374170000018, -24.50869455149999965, -1.530575659700002200 ) ) ;
#1819 = CARTESIAN_POINT ( 'NONE',  ( -5.545418199629476241, -2.237997381628727300, -59.38491726642499202 ) ) ;
#1820 = CARTESIAN_POINT ( 'NONE',  ( 27.79999999999999716, -2.352606998100000196E-11, 229.0000000000000000 ) ) ;
#1821 = CARTESIAN_POINT ( 'NONE',  ( 16.37473331889771089, 11.76353838340827984, -0.6999999999999784173 ) ) ;
#1822 = EDGE_LOOP ( 'NONE', ( #6644, #944, #26325, #17336 ) ) ;
#1823 = CARTESIAN_POINT ( 'NONE',  ( 0.000000000000000000, 0.000000000000000000, 229.1412452697749984 ) ) ;
#1824 = DIRECTION ( 'NONE',  ( 0.9316362575375356503, 0.3633921898465274913, 0.000000000000000000 ) ) ;
#1825 = CARTESIAN_POINT ( 'NONE',  ( 2.188149499615938964, -3.610012245673223319, -68.10000000002503384 ) ) ;
#1826 = CARTESIAN_POINT ( 'NONE',  ( 1.335589245615521836, -3.267430459516901475, -0.6999999999999783062 ) ) ;
#1827 = CARTESIAN_POINT ( 'NONE',  ( -23.95771898018137236, -13.50170546705606789, 226.0719093208724075 ) ) ;
#1828 = VERTEX_POINT ( 'NONE', #24929 ) ;
#1829 = CARTESIAN_POINT ( 'NONE',  ( -10.00000000008316370, -24.60099947280619404, -26.55635984007588490 ) ) ;
#1830 = CARTESIAN_POINT ( 'NONE',  ( 3.916181512753878824, -4.480608557854155904, -64.97605006312500109 ) ) ;
#1831 = ORIENTED_EDGE ( 'NONE', *, *, #8892, .T. ) ;
#1832 = DIRECTION ( 'NONE',  ( 0.9316362575375356503, 0.3633921898465274913, 0.000000000000000000 ) ) ;
#1833 = CARTESIAN_POINT ( 'NONE',  ( -3.388043077342722142, -1.111846212892217522, -88.52261276308685467 ) ) ;
#1834 = ORIENTED_EDGE ( 'NONE', *, *, #16604, .T. ) ;
#1835 = CARTESIAN_POINT ( 'NONE',  ( 1.630907767950000142, 5.558498091389999729, 226.6412452697800006 ) ) ;
#1836 = DIRECTION ( 'NONE',  ( 2.612942924549014782E-24, -1.000000000000000000, 2.257145581549775024E-12 ) ) ;
#1837 = DIRECTION ( 'NONE',  ( 1.000000000000000000, -6.668066630619518976E-24, -2.257150022442225012E-12 ) ) ;
#1838 = EDGE_CURVE ( 'NONE', #4180, #4540, #6968, .T. ) ;
#1839 = CARTESIAN_POINT ( 'NONE',  ( 0.5184513693225318853, -28.49550581263314086, 3.899998581000013509 ) ) ;
#1840 = CARTESIAN_POINT ( 'NONE',  ( -12.38084235052671822, -22.00000000000000355, -29.54157481573779975 ) ) ;
#1841 = EDGE_CURVE ( 'NONE', #11998, #790, #5415, .T. ) ;
#1842 = CYLINDRICAL_SURFACE ( 'NONE', #13013, 2.500000000000002220 ) ;
#1843 = ORIENTED_EDGE ( 'NONE', *, *, #15798, .F. ) ;
#1844 = CARTESIAN_POINT ( 'NONE',  ( -28.68577476999353237, 9.950727454195712696, 1.000000000000000888 ) ) ;
#1845 = DIRECTION ( 'NONE',  ( 1.000000000000000000, 0.000000000000000000, -2.257150022439999944E-12 ) ) ;
#1846 = CARTESIAN_POINT ( 'NONE',  ( 20.30406631279999985, 20.00000862929999812, 229.1257344590000002 ) ) ;
#1847 = CARTESIAN_POINT ( 'NONE',  ( -16.01886467873034547, -9.739971655381781446, 0.000000000000000000 ) ) ;
#1848 = DIRECTION ( 'NONE',  ( 1.000000000000000000, -3.757855673434259506E-24, -2.257150022441365115E-12 ) ) ;
#1849 = CARTESIAN_POINT ( 'NONE',  ( -1.089818731930000117, -28.47945802909999813, 225.3102023309999993 ) ) ;
#1850 = CARTESIAN_POINT ( 'NONE',  ( -0.2860395613546503069, -27.49884598709234496, 226.0719093208176673 ) ) ;
#1851 = DIRECTION ( 'NONE',  ( 1.000000000000000000, 0.000000000000000000, 0.000000000000000000 ) ) ;
#1852 = CARTESIAN_POINT ( 'NONE',  ( -5.206543681532186163, -1.819677770405741413, -49.60743646232500481 ) ) ;
#1853 = CARTESIAN_POINT ( 'NONE',  ( 10.46446609389999871, 20.99999999999999645, -54.63553390589999736 ) ) ;
#1854 = DIRECTION ( 'NONE',  ( 0.000000000000000000, 0.000000000000000000, -1.000000000000000000 ) ) ;
#1855 = LINE ( 'NONE', #16324, #16326 ) ;
#1856 = CARTESIAN_POINT ( 'NONE',  ( -24.34131725940281044, -12.79741914667978619, 224.7820750478432217 ) ) ;
#1857 = ORIENTED_EDGE ( 'NONE', *, *, #6043, .F. ) ;
#1858 = CARTESIAN_POINT ( 'NONE',  ( 3.436082050571383828, -2.282315740991611719, -36.89625473019999902 ) ) ;
#1859 = EDGE_LOOP ( 'NONE', ( #31058, #20185, #25944, #5885 ) ) ;
#1860 = B_SPLINE_CURVE_WITH_KNOTS ( 'NONE', 1,
 ( #6195, #25409 ),
 .UNSPECIFIED., .F., .F.,
 ( 2, 2 ),
 ( -0.7000000000030000002, -4.440892098500626162E-16 ),
 .UNSPECIFIED. ) ;
#1861 = CARTESIAN_POINT ( 'NONE',  ( -3.221934060409652023, 3.671197199744479001, -53.98587006832499924 ) ) ;
#1862 = ORIENTED_EDGE ( 'NONE', *, *, #1050, .F. ) ;
#1863 = EDGE_CURVE ( 'NONE', #11498, #6120, #24556, .T. ) ;
#1864 = ITEM_DEFINED_TRANSFORMATION ( 'NONE', 'NONE', #11830,  #17722 ) ;
#1865 = VERTEX_POINT ( 'NONE', #20050 ) ;
#1866 = DIRECTION ( 'NONE',  ( 1.000000000000000000, 3.757855673434259506E-24, -2.257150022441365115E-12 ) ) ;
#1867 = PRODUCT_DEFINITION_SHAPE ( 'NONE', 'NONE',  #15813 ) ;
#1868 = ORIENTED_EDGE ( 'NONE', *, *, #9506, .T. ) ;
#1869 = CARTESIAN_POINT ( 'NONE',  ( 8.700000000277906764, -15.94902145836247342, -35.53273252485295330 ) ) ;
#1870 = CARTESIAN_POINT ( 'NONE',  ( -27.23548387100000312, 1.421085471519999843E-14, 91.66046017469999185 ) ) ;
#1871 = CARTESIAN_POINT ( 'NONE',  ( -9.800032898256745284, -130.0000000000000000, -43.01413704553658590 ) ) ;
#1872 = CIRCLE ( 'NONE', #11449, 17.84349269770000035 ) ;
#1873 = FACE_OUTER_BOUND ( 'NONE', #20051, .T. ) ;
#1874 = CARTESIAN_POINT ( 'NONE',  ( 10.80000000000790550, -15.94902145823651907, -35.53273252494266643 ) ) ;
#1875 = CARTESIAN_POINT ( 'NONE',  ( -16.99740504728543655, 12.09719844076589013, -4.336808689942018722E-16 ) ) ;
#1876 = CARTESIAN_POINT ( 'NONE',  ( -1.949381390262891589, -5.750991590113663676, 0.02436948729999527385 ) ) ;
#1877 =( GEOMETRIC_REPRESENTATION_CONTEXT ( 3 ) GLOBAL_UNCERTAINTY_ASSIGNED_CONTEXT ( ( #4352 ) ) GLOBAL_UNIT_ASSIGNED_CONTEXT ( ( #261, #26672, #12356 ) ) REPRESENTATION_CONTEXT ( 'NONE', 'WORKASPACE' ) );
#1878 = CARTESIAN_POINT ( 'NONE',  ( -22.47789033090000288, -19.86937924559999757, 230.6999999999999886 ) ) ;
#1879 = ORIENTED_EDGE ( 'NONE', *, *, #15322, .T. ) ;
#1880 = CARTESIAN_POINT ( 'NONE',  ( 25.00848081462686068, -13.67001763210799758, 6.099998580999997699 ) ) ;
#1881 = CARTESIAN_POINT ( 'NONE',  ( 1.403799475828179766, 5.569137675590418723, -17.65080441500000674 ) ) ;
#1882 = CARTESIAN_POINT ( 'NONE',  ( 5.877945039781666381, 1.734296231098907182, -34.93159726780001506 ) ) ;
#1883 = CARTESIAN_POINT ( 'NONE',  ( -0.2196051096525505342, -26.79904497467719438, 6.087620938723986797 ) ) ;
#1884 = CARTESIAN_POINT ( 'NONE',  ( 0.03533597110129999691, -28.50021994999999819, 223.9000014189999774 ) ) ;
#1885 = CARTESIAN_POINT ( 'NONE',  ( 1.498515220174240659, -28.61801908170006925, 8.000000000000007105 ) ) ;
#1886 = CARTESIAN_POINT ( 'NONE',  ( -17.47315945020183037, -28.94086986751210588, -33.05294095162887658 ) ) ;
#1887 = B_SPLINE_CURVE_WITH_KNOTS ( 'NONE', 3,
 ( #23076, #22606, #13141, #11110, #18341, #27943 ),
 .UNSPECIFIED., .F., .F.,
 ( 4, 2, 4 ),
 ( 0.000000000000000000, 0.5000000000000000000, 1.000000000000000000 ),
 .UNSPECIFIED. ) ;
#1888 = B_SPLINE_SURFACE_WITH_KNOTS ( 'NONE', 5, 1, ( 
 ( #25832, #30398 ),
 ( #13549, #23631 ),
 ( #20632, #9290 ),
 ( #4270, #11190 ),
 ( #1601, #11042 ),
 ( #28331, #20789 ),
 ( #1759, #8979 ),
 ( #6780, #27702 ),
 ( #21106, #6149 ),
 ( #8820, #2066 ),
 ( #25984, #16068 ),
 ( #15748, #4421 ),
 ( #25677, #23311 ),
 ( #11657, #25361 ),
 ( #11349, #22998 ) ),
 .UNSPECIFIED., .F., .F., .F.,
 ( 6, 3, 3, 3, 6 ),
 ( 2, 2 ),
 ( 0.000000000000000000, 0.5239049114870000246, 1.047809822970000138, 1.571714734459999985, 1.746349704960000082 ),
 ( -0.7000000000009999335, 2.557517344899999924E-06 ),
 .UNSPECIFIED. ) ;
#1889 = CARTESIAN_POINT ( 'NONE',  ( 26.79556473285982321, 0.4875557887249821198, -0.6999999999999784173 ) ) ;
#1890 = LINE ( 'NONE', #6760, #17257 ) ;
#1891 = CARTESIAN_POINT ( 'NONE',  ( 8.700000000233908182, -29.89969810940666406, -27.53547359536790395 ) ) ;
#1892 = EDGE_CURVE ( 'NONE', #3795, #15436, #7619, .T. ) ;
#1893 = AXIS2_PLACEMENT_3D ( 'NONE', #15878, #8621, #6738 ) ;
#1894 = CARTESIAN_POINT ( 'NONE',  ( -3.629744515141296368, -1.804033921010813835, -69.53494419781382874 ) ) ;
#1895 = ORIENTED_EDGE ( 'NONE', *, *, #2972, .T. ) ;
#1896 = VECTOR ( 'NONE', #8931, 1000.000000000000000 ) ;
#1897 = CARTESIAN_POINT ( 'NONE',  ( -17.83908356944316864, -8.536708948802910868, 0.000000000000000000 ) ) ;
#1898 = CARTESIAN_POINT ( 'NONE',  ( -24.19505510210000310, -13.69211658319999891, 223.9201349309999785 ) ) ;
#1899 = DIRECTION ( 'NONE',  ( -1.000000000000000000, 5.687697999151106851E-16, -6.771501495036750356E-12 ) ) ;
#1900 = ORIENTED_EDGE ( 'NONE', *, *, #25212, .T. ) ;
#1901 = CARTESIAN_POINT ( 'NONE',  ( 3.001777156698443250, -4.698362801289899693, -43.56966640442499283 ) ) ;
#1902 = ORIENTED_EDGE ( 'NONE', *, *, #16079, .T. ) ;
#1903 = EDGE_CURVE ( 'NONE', #19512, #21002, #23668, .T. ) ;
#1904 = VERTEX_POINT ( 'NONE', #22573 ) ;
#1905 = VERTEX_POINT ( 'NONE', #1017 ) ;
#1906 = CARTESIAN_POINT ( 'NONE',  ( 21.20256267760000313, 17.00023892710000339, 230.6999999999999886 ) ) ;
#1907 = EDGE_LOOP ( 'NONE', ( #7559, #15440 ) ) ;
#1908 = CARTESIAN_POINT ( 'NONE',  ( 23.77307027441306531, -14.41181805765238444, 4.999998581000003384 ) ) ;
#1909 = CARTESIAN_POINT ( 'NONE',  ( 24.41841038956698640, 14.69667349781389376, 3.899998581000013509 ) ) ;
#1910 = CARTESIAN_POINT ( 'NONE',  ( -24.21906834513991313, -15.02342241408235068, 3.957526371000025023 ) ) ;
#1911 = CARTESIAN_POINT ( 'NONE',  ( 2.301205939271937950, 3.174620980500392875, -35.69999999999999574 ) ) ;
#1912 = AXIS2_PLACEMENT_3D ( 'NONE', #21616, #66, #9646 ) ;
#1913 = B_SPLINE_CURVE_WITH_KNOTS ( 'NONE', 1,
 ( #30730, #51 ),
 .UNSPECIFIED., .F., .F.,
 ( 2, 2 ),
 ( -0.0003775010496399999857, 0.7000000000080000007 ),
 .UNSPECIFIED. ) ;
#1914 = CARTESIAN_POINT ( 'NONE',  ( 0.9930499629047704335, -5.067522214784211165, -93.52962329551429832 ) ) ;
#1915 = VECTOR ( 'NONE', #13110, 1000.000000000000000 ) ;
#1916 = CYLINDRICAL_SURFACE ( 'NONE', #2394, 1.700000000000000178 ) ;
#1917 = CARTESIAN_POINT ( 'NONE',  ( 2.520003984824367826, -2.635225063011365609, 227.7302799852730288 ) ) ;
#1918 = PLANE ( 'NONE',  #23555 ) ;
#1919 = EDGE_CURVE ( 'NONE', #23553, #25078, #23536, .T. ) ;
#1920 = ORIENTED_EDGE ( 'NONE', *, *, #20595, .F. ) ;
#1921 = AXIS2_PLACEMENT_3D ( 'NONE', #21953, #5105, #17369 ) ;
#1922 = CARTESIAN_POINT ( 'NONE',  ( -3.357947603668644199, 3.429589946161242242, -5.506232180600006743 ) ) ;
#1923 = CARTESIAN_POINT ( 'NONE',  ( 5.972505199797514486, -1.290950946386169917, -23.79036215650000230 ) ) ;
#1924 = LINE ( 'NONE', #30714, #27909 ) ;
#1925 = VECTOR ( 'NONE', #13869, 1000.000000000000000 ) ;
#1926 = CARTESIAN_POINT ( 'NONE',  ( -3.521042344302073079, -0.5632927345592675383, -88.52261276306772686 ) ) ;
#1927 = FACE_OUTER_BOUND ( 'NONE', #29291, .T. ) ;
#1928 = DIRECTION ( 'NONE',  ( -3.018418848199642865E-16, -1.000000000000000000, 0.000000000000000000 ) ) ;
#1929 = DIRECTION ( 'NONE',  ( -0.9316362575375349842, 0.3633921898465292122, -0.000000000000000000 ) ) ;
#1930 = CARTESIAN_POINT ( 'NONE',  ( -6.000000000000000000, -23.85203919881242385, -77.55976184388477179 ) ) ;
#1931 = CARTESIAN_POINT ( 'NONE',  ( 1.645560275461343203, -28.45273235261698019, 5.104056378000016103 ) ) ;
#1932 = CARTESIAN_POINT ( 'NONE',  ( -9.999999999949999108, -30.49286765380000119, -21.04171673159999756 ) ) ;
#1933 = EDGE_LOOP ( 'NONE', ( #30266, #6187, #28949, #10531 ) ) ;
#1934 = CARTESIAN_POINT ( 'NONE',  ( -4.631110635561381805, 2.546857509239208728, -59.06908057272500656 ) ) ;
#1935 = CARTESIAN_POINT ( 'NONE',  ( -24.43008698341936835, 14.67811372381255630, 5.507121130000014020 ) ) ;
#1936 = TOROIDAL_SURFACE ( 'NONE', #28572, 12.03781779390000040, 6.000000000000000000 ) ;
#1937 = CARTESIAN_POINT ( 'NONE',  ( 1.186786632755666426, -28.47586096821117252, 4.099089508000003157 ) ) ;
#1938 = CARTESIAN_POINT ( 'NONE',  ( 49.56288048729999218, -32.92067553680000458, 44.14124526979999530 ) ) ;
#1939 = ORIENTED_EDGE ( 'NONE', *, *, #28404, .T. ) ;
#1940 = CARTESIAN_POINT ( 'NONE',  ( -17.83930458849792089, 19.99999999999597478, -1.000005633855494125E-09 ) ) ;
#1941 = FACE_OUTER_BOUND ( 'NONE', #25354, .T. ) ;
#1942 = B_SPLINE_CURVE_WITH_KNOTS ( 'NONE', 3,
 ( #1979, #9825, #26502, #2126, #30923, #21476, #4945, #17056, #14556, #26049, #14240 ),
 .UNSPECIFIED., .F., .F.,
 ( 4, 1, 1, 1, 2, 2, 4 ),
 ( 0.000000000000000000, 0.2500000000000019429, 0.3750000000000003886, 0.4375000000000022204, 0.4687500000000021649, 0.5000000000000019984, 1.000000000000000000 ),
 .UNSPECIFIED. ) ;
#1943 = ORIENTED_EDGE ( 'NONE', *, *, #7815, .T. ) ;
#1944 = EDGE_LOOP ( 'NONE', ( #7584, #29136, #1792, #3087 ) ) ;
#1945 = EDGE_CURVE ( 'NONE', #24116, #11717, #903, .T. ) ;
#1946 = EDGE_LOOP ( 'NONE', ( #26278, #25673, #20554, #24299 ) ) ;
#1947 = ORIENTED_EDGE ( 'NONE', *, *, #186, .T. ) ;
#1948 = CARTESIAN_POINT ( 'NONE',  ( 24.43008698959658176, -14.67811372800087000, 5.507121129000008608 ) ) ;
#1949 = VECTOR ( 'NONE', #7026, 1000.000000000000000 ) ;
#1950 = CARTESIAN_POINT ( 'NONE',  ( 23.56630063294606714, -14.17280417058648467, 4.005116770382093350 ) ) ;
#1951 = CARTESIAN_POINT ( 'NONE',  ( -1.595193757947241497, 6.212219048941578059, -66.20876360962500939 ) ) ;
#1952 = CARTESIAN_POINT ( 'NONE',  ( 25.39242439670000095, -14.55250846959999933, 229.2930774670000176 ) ) ;
#1953 = B_SPLINE_CURVE_WITH_KNOTS ( 'NONE', 3,
 ( #25642, #6882, #11469, #4071, #21215, #11154 ),
 .UNSPECIFIED., .F., .F.,
 ( 4, 2, 4 ),
 ( 0.000000000000000000, 0.5000000000000001110, 1.000000000000000000 ),
 .UNSPECIFIED. ) ;
#1954 =( REPRESENTATION_RELATIONSHIP ('NONE','NONE', #2712, #20820 ) REPRESENTATION_RELATIONSHIP_WITH_TRANSFORMATION ( #23436 )SHAPE_REPRESENTATION_RELATIONSHIP( ) );
#1955 = CARTESIAN_POINT ( 'NONE',  ( -17.83930458829795640, 19.99999999999961631, -0.6999999999999784173 ) ) ;
#1956 = FACE_OUTER_BOUND ( 'NONE', #2093, .T. ) ;
#1957 = ADVANCED_FACE ( 'NONE', ( #29792 ), #8224, .F. ) ;
#1958 = CARTESIAN_POINT ( 'NONE',  ( -17.48108435972565644, -24.10675719422536289, -24.29685974197550280 ) ) ;
#1959 = VERTEX_POINT ( 'NONE', #25081 ) ;
#1960 = CARTESIAN_POINT ( 'NONE',  ( -19.00669913905015918, 20.00027147608937028, -0.5056402829912918229 ) ) ;
#1961 = CIRCLE ( 'NONE', #8463, 2.000000000000000000 ) ;
#1962 = EDGE_CURVE ( 'NONE', #4471, #28870, #27131, .T. ) ;
#1963 = CARTESIAN_POINT ( 'NONE',  ( 4.315341029122434335, -4.279276102762477940, -14.46112212870000135 ) ) ;
#1964 = CARTESIAN_POINT ( 'NONE',  ( -9.738910687886981776, -24.96785170200593384, 193.2171415880000040 ) ) ;
#1965 = EDGE_CURVE ( 'NONE', #23901, #1607, #22719, .T. ) ;
#1966 = CARTESIAN_POINT ( 'NONE',  ( 3.441895497200000431, 11.73074891959999988, 232.6627635220000059 ) ) ;
#1967 = ORIENTED_EDGE ( 'NONE', *, *, #25601, .F. ) ;
#1968 = CARTESIAN_POINT ( 'NONE',  ( 8.000000000363138852, -29.66236253008535328, -29.83737202107615971 ) ) ;
#1969 = CARTESIAN_POINT ( 'NONE',  ( -9.499999999560001740, 21.70000000000000284, -64.10000000000000853 ) ) ;
#1970 = CARTESIAN_POINT ( 'NONE',  ( -23.08673860280000056, 15.48734418929999990, 222.0000000000000000 ) ) ;
#1971 = LINE ( 'NONE', #14815, #3096 ) ;
#1972 = EDGE_CURVE ( 'NONE', #12725, #15866, #29634, .T. ) ;
#1973 = CARTESIAN_POINT ( 'NONE',  ( -9.000000000000000000, 19.99999999999999645, -42.39999999999999858 ) ) ;
#1974 = CARTESIAN_POINT ( 'NONE',  ( 9.738910687886868089, -24.96785170200598358, 115.0000000000000000 ) ) ;
#1975 = AXIS2_PLACEMENT_3D ( 'NONE', #17193, #24446, #16723 ) ;
#1976 = CARTESIAN_POINT ( 'NONE',  ( 16.06675444873834380, 10.97998838177521286, -0.6999999989999727834 ) ) ;
#1977 = CARTESIAN_POINT ( 'NONE',  ( -12.30800288698999978, -24.60220466956999985, -24.01086508779000184 ) ) ;
#1978 = ORIENTED_EDGE ( 'NONE', *, *, #2333, .F. ) ;
#1979 = CARTESIAN_POINT ( 'NONE',  ( -12.30800288698999978, -24.60220466956999985, -24.01086508779000184 ) ) ;
#1980 = CARTESIAN_POINT ( 'NONE',  ( 0.000000000000000000, 27.10555629988041204, -61.14106941751904856 ) ) ;
#1981 = CARTESIAN_POINT ( 'NONE',  ( 2.771604730552712947, -3.765259971643367010, -68.10000000002500542 ) ) ;
#1982 = EDGE_CURVE ( 'NONE', #27268, #21389, #15470, .T. ) ;
#1983 = AXIS2_PLACEMENT_3D ( 'NONE', #20686, #8871, #4163 ) ;
#1984 = CARTESIAN_POINT ( 'NONE',  ( 17.83931306984926835, 20.00000000000176570, -0.6999999999999784173 ) ) ;
#1985 = LINE ( 'NONE', #14834, #7163 ) ;
#1986 = ADVANCED_FACE ( 'NONE', ( #30114, #6190 ), #13906, .F. ) ;
#1987 = FILL_AREA_STYLE ('',( #18340 ) ) ;
#1988 = ORIENTED_EDGE ( 'NONE', *, *, #29277, .T. ) ;
#1989 = FACE_BOUND ( 'NONE', #6422, .T. ) ;
#1990 = CARTESIAN_POINT ( 'NONE',  ( 6.385918709370476343, 0.1527399656023400998, -64.54686508972500292 ) ) ;
#1991 = ORIENTED_EDGE ( 'NONE', *, *, #13667, .F. ) ;
#1992 = EDGE_CURVE ( 'NONE', #5428, #16559, #22508, .T. ) ;
#1993 = CARTESIAN_POINT ( 'NONE',  ( -17.83931601680000156, 20.00000000000000000, 230.7000111870000012 ) ) ;
#1994 = CARTESIAN_POINT ( 'NONE',  ( -2.914123423697624116, -2.127246859470591112, -88.52261276302716908 ) ) ;
#1995 = ORIENTED_EDGE ( 'NONE', *, *, #12701, .T. ) ;
#1996 = CARTESIAN_POINT ( 'NONE',  ( 0.7577809307819999285, 5.814680484680000205, 226.6412452697800006 ) ) ;
#1997 = CARTESIAN_POINT ( 'NONE',  ( -23.23955040174346465, -15.25661106733265981, 4.791628272000025390 ) ) ;
#1998 = CARTESIAN_POINT ( 'NONE',  ( 9.707106781189999367, 19.99999999999999645, -43.10710678118599759 ) ) ;
#1999 = LINE ( 'NONE', #29299, #4426 ) ;
#2000 = CARTESIAN_POINT ( 'NONE',  ( -0.5821515579339680002, -27.79407096281863687, 4.791896188000022150 ) ) ;
#2001 = CARTESIAN_POINT ( 'NONE',  ( -7.783406290388187543, 3.155933242387642057, -42.35622648219886344 ) ) ;
#2002 = CARTESIAN_POINT ( 'NONE',  ( -10.00000000070000183, -29.30501631370000482, -26.47986984990000181 ) ) ;
#2003 = VERTEX_POINT ( 'NONE', #13269 ) ;
#2004 = CARTESIAN_POINT ( 'NONE',  ( 14.47923079777836008, -32.00000000000144951, -25.78086934637092753 ) ) ;
#2005 = LINE ( 'NONE', #6708, #24844 ) ;
#2006 = CARTESIAN_POINT ( 'NONE',  ( 19.65673127730000402, 20.00000654480000151, 230.1824637990000042 ) ) ;
#2007 = CARTESIAN_POINT ( 'NONE',  ( -25.27355175290000133, 12.75978488059999805, 227.5999999999999943 ) ) ;
#2008 = CARTESIAN_POINT ( 'NONE',  ( -12.75378086759999796, -32.00000000000000000, -31.28675134614999820 ) ) ;
#2009 = CARTESIAN_POINT ( 'NONE',  ( -3.389121577140000063, -11.55088360979999962, 230.6412452697800006 ) ) ;
#2010 = DIRECTION ( 'NONE',  ( -0.8090169943751909232, 0.5877852522921378498, 0.000000000000000000 ) ) ;
#2011 = DIRECTION ( 'NONE',  ( 1.000000000000000000, 0.000000000000000000, 0.000000000000000000 ) ) ;
#2012 = CARTESIAN_POINT ( 'NONE',  ( -5.939015604524707115, -0.1501891088408410790, -53.55673954922500002 ) ) ;
#2013 = AXIS2_PLACEMENT_3D ( 'NONE', #490, #2676, #5037 ) ;
#2014 = B_SPLINE_CURVE_WITH_KNOTS ( 'NONE', 5,
 ( #9521, #12345, #12036, #12180, #7006, #19274, #16744, #403, #21791, #6843, #248, #24006, #14248, #9831, #21483 ),
 .UNSPECIFIED., .F., .F.,
 ( 6, 3, 3, 3, 6 ),
 ( 0.000000000000000000, 0.2499999999995511091, 0.4999999999991022182, 0.7499999999986531884, 1.000000000000000000 ),
 .UNSPECIFIED. ) ;
#2015 = CARTESIAN_POINT ( 'NONE',  ( 27.24406355354254217, 0.4957164003247224726, 0.08279779300002232389 ) ) ;
#2016 = CARTESIAN_POINT ( 'NONE',  ( 8.700000000286559398, -7.565603753668719733, -31.48340496194444782 ) ) ;
#2017 = CARTESIAN_POINT ( 'NONE',  ( 3.479864333095661344, -0.9723755506658986469, 230.7708768453293260 ) ) ;
#2018 = EDGE_CURVE ( 'NONE', #26248, #16461, #3994, .T. ) ;
#2019 = CARTESIAN_POINT ( 'NONE',  ( -1.100000000000000089, -27.47799119300000115, 225.0000000000000000 ) ) ;
#2020 = ADVANCED_FACE ( 'NONE', ( #22883 ), #3838, .T. ) ;
#2021 = EDGE_CURVE ( 'NONE', #6914, #5828, #23517, .T. ) ;
#2022 = CARTESIAN_POINT ( 'NONE',  ( 10.69999999999999929, -24.87867965640000278, -30.52132034359999935 ) ) ;
#2023 = EDGE_CURVE ( 'NONE', #2398, #16829, #7123, .T. ) ;
#2024 = EDGE_LOOP ( 'NONE', ( #11963, #29832 ) ) ;
#2025 = CARTESIAN_POINT ( 'NONE',  ( -1.256295066205788347, -5.815478746186413694, -56.41033560642500078 ) ) ;
#2026 = ORIENTED_EDGE ( 'NONE', *, *, #3615, .T. ) ;
#2027 = ORIENTED_EDGE ( 'NONE', *, *, #20844, .F. ) ;
#2028 = CARTESIAN_POINT ( 'NONE',  ( 0.000000000000000000, 0.000000000000000000, 190.0000000000000000 ) ) ;
#2029 = ORIENTED_EDGE ( 'NONE', *, *, #10803, .T. ) ;
#2030 = CARTESIAN_POINT ( 'NONE',  ( -10.00000000000000000, -13.98526668056139144, -73.96855033896248699 ) ) ;
#2031 = CYLINDRICAL_SURFACE ( 'NONE', #9951, 26.80000000000002203 ) ;
#2032 = CARTESIAN_POINT ( 'NONE',  ( -27.07233446963630996, 8.380005019355408535, 3.799999999999998046 ) ) ;
#2033 = CIRCLE ( 'NONE', #14094, 18.16530045500000057 ) ;
#2034 = CARTESIAN_POINT ( 'NONE',  ( -5.056117937459999823, -11.13261400500000065, 232.6627648150000027 ) ) ;
#2035 = CARTESIAN_POINT ( 'NONE',  ( -4.667733413579616908, -30.93201666723582122, 1.000000000000000888 ) ) ;
#2036 = CARTESIAN_POINT ( 'NONE',  ( 4.638687372303287759, 5.146895567816208938, -43.32728369091725540 ) ) ;
#2037 = CARTESIAN_POINT ( 'NONE',  ( -2.014747437493234816, 4.354226950121528716, -6.794225184300000997 ) ) ;
#2038 = CARTESIAN_POINT ( 'NONE',  ( 5.041582825300000792, -29.73257086209999756, 230.6999999999999886 ) ) ;
#2039 = ORIENTED_EDGE ( 'NONE', *, *, #17060, .F. ) ;
#2040 = CARTESIAN_POINT ( 'NONE',  ( 10.69999999989999928, -2.500000000000002220, -2.399999999999999467 ) ) ;
#2041 = CARTESIAN_POINT ( 'NONE',  ( 6.482330152203070739, 0.4632910120546396282, -14.64454535870000207 ) ) ;
#2042 = CARTESIAN_POINT ( 'NONE',  ( 0.8979745064479516259, 3.499999999999999112, 230.7711489403451424 ) ) ;
#2043 = LINE ( 'NONE', #26264, #3448 ) ;
#2044 = CARTESIAN_POINT ( 'NONE',  ( 27.47617339892474675, -9.531132158558678569, -0.6577119969999878357 ) ) ;
#2045 = CARTESIAN_POINT ( 'NONE',  ( -24.30742244220000003, -13.49161940279999961, 223.9971936000000028 ) ) ;
#2046 = CARTESIAN_POINT ( 'NONE',  ( -26.07456367145396214, -11.88770200349126327, 8.000000000000007105 ) ) ;
#2047 = CARTESIAN_POINT ( 'NONE',  ( 3.915051063684143795, -2.600456723069958453, -42.55875473022500444 ) ) ;
#2048 = CARTESIAN_POINT ( 'NONE',  ( 28.45300238704230367, 0.5177135156027404816, 0.5017677510000262409 ) ) ;
#2049 = CARTESIAN_POINT ( 'NONE',  ( -8.699999999715885224, -26.99999999997790923, -28.40000000002690683 ) ) ;
#2050 = CYLINDRICAL_SURFACE ( 'NONE', #20849, 10.00000000000000178 ) ;
#2051 = CARTESIAN_POINT ( 'NONE',  ( 2.910560681360000016E-11, 19.99999999999999645, -45.10000000000000142 ) ) ;
#2052 = ORIENTED_EDGE ( 'NONE', *, *, #16040, .T. ) ;
#2053 = FACE_OUTER_BOUND ( 'NONE', #14291, .T. ) ;
#2054 =( NAMED_UNIT ( * ) PLANE_ANGLE_UNIT ( ) SI_UNIT ( $, .RADIAN. ) );
#2055 = CARTESIAN_POINT ( 'NONE',  ( -2.825020644939634007, -4.425443225455641283, -0.6999999999999992895 ) ) ;
#2056 = ORIENTED_EDGE ( 'NONE', *, *, #26704, .F. ) ;
#2057 = CARTESIAN_POINT ( 'NONE',  ( 2.766343654246206984, -4.329863758072034940, -44.36966640442500420 ) ) ;
#2058 = VERTEX_POINT ( 'NONE', #13425 ) ;
#2059 = ORIENTED_EDGE ( 'NONE', *, *, #8464, .F. ) ;
#2060 = DIRECTION ( 'NONE',  ( 1.000000000000000000, 0.000000000000000000, 0.000000000000000000 ) ) ;
#2061 = TOROIDAL_SURFACE ( 'NONE', #7574, 29.80000000000000071, 3.000000000000000000 ) ;
#2062 = ORIENTED_EDGE ( 'NONE', *, *, #2738, .T. ) ;
#2063 = CARTESIAN_POINT ( 'NONE',  ( -0.2402207101440000103, -27.79943747540000132, 223.9202095490000204 ) ) ;
#2064 = ADVANCED_BREP_SHAPE_REPRESENTATION ( '', ( #21535, #17722 ), #25295 ) ;
#2065 = ORIENTED_EDGE ( 'NONE', *, *, #19134, .T. ) ;
#2066 = CARTESIAN_POINT ( 'NONE',  ( -24.26052213759999887, -13.57583965329999920, 226.0425107039999943 ) ) ;
#2067 = CARTESIAN_POINT ( 'NONE',  ( 23.25311087529421172, 15.23597699658644800, 4.689445052000001724 ) ) ;
#2068 = CARTESIAN_POINT ( 'NONE',  ( -2.595987296770100095, -16.63200279373747392, -109.8342699011499946 ) ) ;
#2069 = CARTESIAN_POINT ( 'NONE',  ( 1.612571865511672531, 3.683153181086038952, -35.70000000000000284 ) ) ;
#2070 = CARTESIAN_POINT ( 'NONE',  ( 18.62828648731074921, 19.99998815318511092, -0.6147320732107522945 ) ) ;
#2071 = CARTESIAN_POINT ( 'NONE',  ( 10.69999999999999929, -27.00000000000000000, -28.40000000000000213 ) ) ;
#2072 = CARTESIAN_POINT ( 'NONE',  ( -6.661312627754254478, -7.245008774417666331, -33.94554228739334434 ) ) ;
#2073 = CARTESIAN_POINT ( 'NONE',  ( -18.92356980859999993, 19.72862807099999927, 229.8505673220000176 ) ) ;
#2074 = EDGE_CURVE ( 'NONE', #13351, #2375, #5605, .T. ) ;
#2075 = ORIENTED_EDGE ( 'NONE', *, *, #1351, .F. ) ;
#2076 = CARTESIAN_POINT ( 'NONE',  ( -3.052679639724403593, 3.117809041995149411, -5.068732180600003190 ) ) ;
#2077 = CARTESIAN_POINT ( 'NONE',  ( 0.09521150875769815447, -4.665041947735804939, -23.91888333260000365 ) ) ;
#2078 = DIRECTION ( 'NONE',  ( 0.3633921898465272138, -0.9316362575375356503, 0.000000000000000000 ) ) ;
#2079 = CARTESIAN_POINT ( 'NONE',  ( -3.873164236031628516, -2.119290023631752007, -95.69213379017060106 ) ) ;
#2080 = DIRECTION ( 'NONE',  ( 0.000000000000000000, -2.257145581549999994E-12, -1.000000000000000000 ) ) ;
#2081 = DIRECTION ( 'NONE',  ( 1.000000000000000000, -9.219999999999999084E-13, 4.710999999999999616E-12 ) ) ;
#2082 = CARTESIAN_POINT ( 'NONE',  ( 26.57440914490000239, -3.469982507400000582, -0.6999999995999997005 ) ) ;
#2083 = EDGE_CURVE ( 'NONE', #24262, #22250, #20514, .T. ) ;
#2084 = STYLED_ITEM ( 'NONE', ( #22315 ), #21218 ) ;
#2085 = DIRECTION ( 'NONE',  ( 1.224606353819999829E-16, 1.000000000000000000, 0.000000000000000000 ) ) ;
#2086 = CARTESIAN_POINT ( 'NONE',  ( 0.5537481963840298338, -28.49486543565700813, 6.099998581000020792 ) ) ;
#2087 = CARTESIAN_POINT ( 'NONE',  ( -17.93324555108848628, -9.020011617866936504, 0.000000000000000000 ) ) ;
#2088 = ORIENTED_EDGE ( 'NONE', *, *, #11772, .T. ) ;
#2089 = CARTESIAN_POINT ( 'NONE',  ( -4.300317018729668206, 2.364939115720640750, -59.41908057272499377 ) ) ;
#2090 = CARTESIAN_POINT ( 'NONE',  ( -21.56316276399999765, 17.27952114640000048, 229.9172021830000006 ) ) ;
#2091 = CARTESIAN_POINT ( 'NONE',  ( 18.26639035964474900, 11.02001161816309072, -1.000005633855494125E-09 ) ) ;
#2092 = CARTESIAN_POINT ( 'NONE',  ( -1.611722395286938170, -6.291674585240492057, -27.54882611459999353 ) ) ;
#2093 = EDGE_LOOP ( 'NONE', ( #29555, #27466, #14678, #7835 ) ) ;
#2094 = CARTESIAN_POINT ( 'NONE',  ( -20.97486481260628821, 18.32139253905734932, 225.3333333333333712 ) ) ;
#2095 = CARTESIAN_POINT ( 'NONE',  ( 24.38199545065365115, 14.75707034588002564, 3.901343066999990228 ) ) ;
#2096 = ORIENTED_EDGE ( 'NONE', *, *, #11030, .F. ) ;
#2097 = ORIENTED_EDGE ( 'NONE', *, *, #25278, .F. ) ;
#2098 = VERTEX_POINT ( 'NONE', #27745 ) ;
#2099 = VERTEX_POINT ( 'NONE', #11390 ) ;
#2100 = CARTESIAN_POINT ( 'NONE',  ( 24.93720649360215802, -13.79881813812812297, 6.099998581000020792 ) ) ;
#2101 = EDGE_CURVE ( 'NONE', #26977, #14341, #7433, .T. ) ;
#2102 = CARTESIAN_POINT ( 'NONE',  ( -8.699999999651183202, -14.46922738198402136, -37.57413277573995458 ) ) ;
#2103 = CARTESIAN_POINT ( 'NONE',  ( 0.2444022557069348567, 3.892334458579129297, -68.95875473022499591 ) ) ;
#2104 = CARTESIAN_POINT ( 'NONE',  ( 25.16954019099999940, -14.42477239210000128, 229.7313254700000016 ) ) ;
#2105 = AXIS2_PLACEMENT_3D ( 'NONE', #20895, #1223, #18035 ) ;
#2106 = DIRECTION ( 'NONE',  ( 0.000000000000000000, -0.3420201433259318913, 0.9396926207858126157 ) ) ;
#2107 = CARTESIAN_POINT ( 'NONE',  ( 20.43731315469999998, -19.07003687599999964, 222.0000000000000000 ) ) ;
#2108 = VECTOR ( 'NONE', #7734, 1000.000000000000000 ) ;
#2109 = VECTOR ( 'NONE', #2270, 1000.000000000000114 ) ;
#2110 = CARTESIAN_POINT ( 'NONE',  ( 3.636072258898020770, -3.161266087984368145, -0.6999085127358649627 ) ) ;
#2111 = VERTEX_POINT ( 'NONE', #9019 ) ;
#2112 = CARTESIAN_POINT ( 'NONE',  ( -23.06578384684251048, -13.64653153747141801, 226.0721256962708878 ) ) ;
#2113 = CARTESIAN_POINT ( 'NONE',  ( 1.526412975746457290, -4.524531468931415112, -14.32664732020000287 ) ) ;
#2114 = DIRECTION ( 'NONE',  ( 6.386904893851405129E-12, 0.3322662713817149949, -0.9431856258987901809 ) ) ;
#2115 = CARTESIAN_POINT ( 'NONE',  ( -10.69999999969716065, -23.80000000000000071, -28.81986915868696641 ) ) ;
#2116 = ORIENTED_EDGE ( 'NONE', *, *, #25280, .F. ) ;
#2117 = DIRECTION ( 'NONE',  ( 0.000000000000000000, 1.000000000000000000, 0.000000000000000000 ) ) ;
#2118 = CARTESIAN_POINT ( 'NONE',  ( -10.69999999999999929, -27.00000000000000000, -28.40000000000000213 ) ) ;
#2119 = FACE_OUTER_BOUND ( 'NONE', #20985, .T. ) ;
#2120 = EDGE_CURVE ( 'NONE', #17525, #17033, #24050, .T. ) ;
#2121 = FACE_BOUND ( 'NONE', #7009, .T. ) ;
#2122 = CARTESIAN_POINT ( 'NONE',  ( -1.277581537031662107, -5.235359937796273400, -67.93704710652501433 ) ) ;
#2123 = LINE ( 'NONE', #25895, #3671 ) ;
#2124 = DIRECTION ( 'NONE',  ( 1.000000000000000000, -9.219999999999999084E-13, 4.710999999999999616E-12 ) ) ;
#2125 = ORIENTED_EDGE ( 'NONE', *, *, #4176, .F. ) ;
#2126 = CARTESIAN_POINT ( 'NONE',  ( -12.34886039478919173, -23.75151583055949800, -24.50201051798606855 ) ) ;
#2127 = CARTESIAN_POINT ( 'NONE',  ( -7.999999999667107176, -18.39629690576770926, -34.94743992953217315 ) ) ;
#2128 = VECTOR ( 'NONE', #5783, 1000.000000000000000 ) ;
#2129 = B_SPLINE_CURVE_WITH_KNOTS ( 'NONE', 3,
 ( #28979, #14517, #29128, #21599, #664, #26771, #361, #2553, #19229, #24114, #17328, #48, #10099, #14672, #2400, #19389, #19697, #10256, #9942, #12139 ),
 .UNSPECIFIED., .F., .F.,
 ( 4, 1, 1, 1, 2, 2, 2, 1, 1, 1, 2, 2, 4 ),
 ( 0.000000000000000000, 0.1250000000000031641, 0.1875000000000046352, 0.2187500000000062172, 0.2343750000000060785, 0.2500000000000059397, 0.5000000000000045519, 0.6250000000000027756, 0.6875000000000029976, 0.7187500000000029976, 0.7343750000000029976, 0.7500000000000031086, 1.000000000000000000 ),
 .UNSPECIFIED. ) ;
#2130 = CARTESIAN_POINT ( 'NONE',  ( -5.000296138419098924, -9.340612320833740156, -88.85875473022500159 ) ) ;
#2131 = CARTESIAN_POINT ( 'NONE',  ( -4.891993053148940618, -0.3028084928693625666, -68.10000000002500542 ) ) ;
#2132 = ADVANCED_FACE ( 'NONE', ( #23043 ), #25557, .F. ) ;
#2133 = EDGE_CURVE ( 'NONE', #7727, #10044, #5912, .T. ) ;
#2134 = CARTESIAN_POINT ( 'NONE',  ( 3.861721477338983632, 0.2146938847481238977, -40.92168819670553148 ) ) ;
#2135 = CARTESIAN_POINT ( 'NONE',  ( -4.574578478894093081, -2.192947688770922277, -44.10000000002499121 ) ) ;
#2136 =( NAMED_UNIT ( * ) PLANE_ANGLE_UNIT ( ) SI_UNIT ( $, .RADIAN. ) );
#2137 = EDGE_LOOP ( 'NONE', ( #29446, #13219, #24655, #9479 ) ) ;
#2138 = CARTESIAN_POINT ( 'NONE',  ( 27.50000000000000000, -6.735334946019999940E-15, 36.39444872359999295 ) ) ;
#2139 = APPLICATION_CONTEXT ( 'automotive_design' ) ;
#2140 = CARTESIAN_POINT ( 'NONE',  ( 1.311146135404979818, -27.76947565989378219, 4.240358041999986227 ) ) ;
#2141 = ORIENTED_EDGE ( 'NONE', *, *, #30800, .T. ) ;
#2142 = CARTESIAN_POINT ( 'NONE',  ( -3.389121647030000073, -11.55088358959999972, 229.6412452697800006 ) ) ;
#2143 = EDGE_CURVE ( 'NONE', #28317, #14785, #23667, .T. ) ;
#2144 = CARTESIAN_POINT ( 'NONE',  ( -27.63815568848399451, -7.780344951885712845, 0.7069222069999991920 ) ) ;
#2145 = ORIENTED_EDGE ( 'NONE', *, *, #29497, .T. ) ;
#2146 = DIRECTION ( 'NONE',  ( 0.9595496299847263710, -0.2815395311429191305, 0.000000000000000000 ) ) ;
#2147 = VECTOR ( 'NONE', #28800, 1000.000000000000000 ) ;
#2148 = DIRECTION ( 'NONE',  ( 0.000000000000000000, -0.3420201433259318358, 0.9396926207858125046 ) ) ;
#2149 = DIRECTION ( 'NONE',  ( 0.8923938138917432150, -1.018860921557045171E-12, -0.4512574441798702374 ) ) ;
#2150 = UNCERTAINTY_MEASURE_WITH_UNIT (LENGTH_MEASURE( 1.000000000000000082E-05 ), #3991, 'distance_accuracy_value', 'NONE');
#2151 = FACE_OUTER_BOUND ( 'NONE', #4462, .T. ) ;
#2152 = EDGE_CURVE ( 'NONE', #27598, #22033, #3753, .T. ) ;
#2153 = DIRECTION ( 'NONE',  ( 0.3633921898465276024, -0.9316362575375355393, -3.469446951953614189E-14 ) ) ;
#2154 = CARTESIAN_POINT ( 'NONE',  ( -10.69999999930000101, -25.00000000000000000, -26.16393202249999916 ) ) ;
#2155 = ORIENTED_EDGE ( 'NONE', *, *, #21760, .T. ) ;
#2156 = CARTESIAN_POINT ( 'NONE',  ( 22.97559295603346285, 15.65128684871516818, 8.000000000000007105 ) ) ;
#2157 = DIRECTION ( 'NONE',  ( 1.000000000000000000, 0.000000000000000000, 0.000000000000000000 ) ) ;
#2158 = CARTESIAN_POINT ( 'NONE',  ( 1.354415895940000114, 11.99145557159999953, 231.9999989789999972 ) ) ;
#2159 = CARTESIAN_POINT ( 'NONE',  ( -15.78883365603684474, -9.367159789388974644, 0.000000000000000000 ) ) ;
#2160 = DIRECTION ( 'NONE',  ( 0.000000000000000000, 0.000000000000000000, -1.000000000000000000 ) ) ;
#2161 = CARTESIAN_POINT ( 'NONE',  ( -0.03526712872429999673, -28.50022367440000082, 226.1000014189999945 ) ) ;
#2162 = DIRECTION ( 'NONE',  ( -0.8775825618903718706, 0.4794255386042047262, 0.000000000000000000 ) ) ;
#2163 = CARTESIAN_POINT ( 'NONE',  ( 13.99999999979999821, 20.99999999999999645, -58.51619795559999915 ) ) ;
#2164 = DIRECTION ( 'NONE',  ( 0.000000000000000000, 0.000000000000000000, -1.000000000000000000 ) ) ;
#2165 = CARTESIAN_POINT ( 'NONE',  ( -1.293561172433232986, -6.216321778783836294, -52.44706695232499527 ) ) ;
#2166 = EDGE_CURVE ( 'NONE', #22798, #14380, #26634, .T. ) ;
#2167 = CARTESIAN_POINT ( 'NONE',  ( 12.41421356240000051, 26.55509710711128335, -61.34142017886538412 ) ) ;
#2168 = CARTESIAN_POINT ( 'NONE',  ( -27.79999999999999716, -2.360778239559999931E-11, 229.0000000000000000 ) ) ;
#2169 = DIRECTION ( 'NONE',  ( 1.000000000000000000, 0.000000000000000000, 0.000000000000000000 ) ) ;
#2170 = AXIS2_PLACEMENT_3D ( 'NONE', #11835, #13885, #19068 ) ;
#2171 = ORIENTED_EDGE ( 'NONE', *, *, #30137, .F. ) ;
#2172 = DIRECTION ( 'NONE',  ( 0.000000000000000000, 0.000000000000000000, 1.000000000000000000 ) ) ;
#2173 = CARTESIAN_POINT ( 'NONE',  ( -23.50695179570000093, -14.84192241259999889, 224.8957841300000098 ) ) ;
#2174 = CARTESIAN_POINT ( 'NONE',  ( 3.357378826396556271, -2.722208303779470651, -55.40923804942499942 ) ) ;
#2175 = ORIENTED_EDGE ( 'NONE', *, *, #26586, .T. ) ;
#2176 = ITEM_DEFINED_TRANSFORMATION ( 'NONE', 'NONE', #17848,  #17722 ) ;
#2177 = ORIENTED_EDGE ( 'NONE', *, *, #9621, .F. ) ;
#2178 = B_SPLINE_CURVE_WITH_KNOTS ( 'NONE', 3,
 ( #4961, #2456, #259, #26825, #12502, #17072 ),
 .UNSPECIFIED., .F., .F.,
 ( 4, 2, 4 ),
 ( 0.000000000000000000, 0.5000000000000000000, 1.000000000000000000 ),
 .UNSPECIFIED. ) ;
#2179 = CARTESIAN_POINT ( 'NONE',  ( -17.20708009808130612, -31.51741709908550959, -31.56537071389317717 ) ) ;
#2180 = ORIENTED_EDGE ( 'NONE', *, *, #19887, .F. ) ;
#2181 = CARTESIAN_POINT ( 'NONE',  ( 14.63279312439116531, -27.79071840260195003, -23.08346332393403699 ) ) ;
#2182 = AXIS2_PLACEMENT_3D ( 'NONE', #9189, #6836, #18789 ) ;
#2183 = CARTESIAN_POINT ( 'NONE',  ( -8.699999999652812122, -10.55555246029782346, -37.33318641903195356 ) ) ;
#2184 = CYLINDRICAL_SURFACE ( 'NONE', #12936, 2.500000000000000888 ) ;
#2185 = PRODUCT_DEFINITION_SHAPE ( 'NONE', 'NONE',  #31140 ) ;
#2186 = AXIS2_PLACEMENT_3D ( 'NONE', #20936, #17927, #10709 ) ;
#2187 = CARTESIAN_POINT ( 'NONE',  ( -1.674213827660000042, -11.95100239910000006, 231.9999991140000191 ) ) ;
#2188 = DIRECTION ( 'NONE',  ( -1.000000000000000000, -1.433034374054745923E-13, -1.199006074477166028E-12 ) ) ;
#2189 = EDGE_CURVE ( 'NONE', #8183, #12643, #7285, .T. ) ;
#2190 = CARTESIAN_POINT ( 'NONE',  ( -19.80535357377644701, 19.50875577052588739, 1.800000043000016259 ) ) ;
#2191 = CARTESIAN_POINT ( 'NONE',  ( -3.010188847181571870, -5.300177381000955812, -6.085065142700004870 ) ) ;
#2192 = AXIS2_PLACEMENT_3D ( 'NONE', #7627, #22265, #12194 ) ;
#2193 = CARTESIAN_POINT ( 'NONE',  ( 5.361384718760000112, -31.61859215249999977, 229.0000000000000000 ) ) ;
#2194 = ORIENTED_EDGE ( 'NONE', *, *, #27275, .T. ) ;
#2195 = CARTESIAN_POINT ( 'NONE',  ( -24.09883371379999772, -15.21565466309999870, 225.0000014190000002 ) ) ;
#2196 = ADVANCED_FACE ( 'NONE', ( #26328 ), #14682, .F. ) ;
#2197 = CARTESIAN_POINT ( 'NONE',  ( 1.002713911322304696, 3.977955482547951505, -17.05080441500000177 ) ) ;
#2198 = CARTESIAN_POINT ( 'NONE',  ( -0.3083106915816442584, 3.499999999999999556, 230.8358029176229138 ) ) ;
#2199 = CARTESIAN_POINT ( 'NONE',  ( -10.22459498839999981, -25.00000000000000000, -1.538346542999995181 ) ) ;
#2200 = ADVANCED_FACE ( 'NONE', ( #19241 ), #16667, .T. ) ;
#2201 = LINE ( 'NONE', #4866, #16643 ) ;
#2202 = CARTESIAN_POINT ( 'NONE',  ( 27.92857142820000149, 1.776356839399999804E-15, 192.0603150150000147 ) ) ;
#2203 = CARTESIAN_POINT ( 'NONE',  ( 0.7190444496271986008, -5.886645524271489904, -43.78057807742499818 ) ) ;
#2204 = DIRECTION ( 'NONE',  ( 0.000000000000000000, 0.000000000000000000, 1.000000000000000000 ) ) ;
#2205 = CARTESIAN_POINT ( 'NONE',  ( -1.419173372180000084E-06, -27.80022181310000207, 223.9000014189999774 ) ) ;
#2206 = CARTESIAN_POINT ( 'NONE',  ( -24.61381496323305740, -14.36755986783201777, 6.042472825000033687 ) ) ;
#2207 = VECTOR ( 'NONE', #12915, 1000.000000000000114 ) ;
#2208 = AXIS2_PLACEMENT_3D ( 'NONE', #25383, #5703, #20493 ) ;
#2209 = CARTESIAN_POINT ( 'NONE',  ( -1.750888960315145848, -3.972249423281244862, -70.32411010211554014 ) ) ;
#2210 = ORIENTED_EDGE ( 'NONE', *, *, #18493, .F. ) ;
#2211 = CIRCLE ( 'NONE', #10247, 3.750000000000000000 ) ;
#2212 = CARTESIAN_POINT ( 'NONE',  ( -10.08101130870000084, 19.99999999999999645, -1.830192468500003944 ) ) ;
#2213 = FACE_OUTER_BOUND ( 'NONE', #18410, .T. ) ;
#2214 = CARTESIAN_POINT ( 'NONE',  ( -7.999999999655180716, -13.66682223735657864, -36.55330428419717492 ) ) ;
#2215 = EDGE_LOOP ( 'NONE', ( #12039, #1879, #19313, #18321, #26558, #13314 ) ) ;
#2216 = DIRECTION ( 'NONE',  ( 0.000000000000000000, 0.000000000000000000, 1.000000000000000000 ) ) ;
#2217 = EDGE_LOOP ( 'NONE', ( #23343, #25191, #17633, #24809, #15623, #4533 ) ) ;
#2218 = ORIENTED_EDGE ( 'NONE', *, *, #25626, .T. ) ;
#2219 = CARTESIAN_POINT ( 'NONE',  ( 0.000000000000000000, 0.000000000000000000, 0.000000000000000000 ) ) ;
#2220 = ORIENTED_EDGE ( 'NONE', *, *, #29973, .F. ) ;
#2221 = CARTESIAN_POINT ( 'NONE',  ( 11.20000000009999930, -32.00000000000000000, -31.28675134584999640 ) ) ;
#2222 = ORIENTED_EDGE ( 'NONE', *, *, #25739, .F. ) ;
#2223 = CARTESIAN_POINT ( 'NONE',  ( 24.10531740749999940, -15.20475527630000023, 225.2083717279999746 ) ) ;
#2224 = PRESENTATION_STYLE_ASSIGNMENT (( #30702 ) ) ;
#2225 = CYLINDRICAL_SURFACE ( 'NONE', #23013, 1.099999999999999867 ) ;
#2226 = CARTESIAN_POINT ( 'NONE',  ( 1.438618989620732647, 4.694460304239756354, -35.70000000000000284 ) ) ;
#2227 = CARTESIAN_POINT ( 'NONE',  ( 17.83931306984926835, 20.00000000000176570, -0.6999999999999784173 ) ) ;
#2228 = CARTESIAN_POINT ( 'NONE',  ( -24.37165444408190851, 14.77472139917419369, 4.999998581000003384 ) ) ;
#2229 = CARTESIAN_POINT ( 'NONE',  ( -4.861312627774928785, -9.411244188027135138, -32.88899868167055018 ) ) ;
#2230 = AXIS2_PLACEMENT_3D ( 'NONE', #15972, #10626, #18001 ) ;
#2231 = CARTESIAN_POINT ( 'NONE',  ( 17.73794748038870139, -9.950927728802978933, -4.336808689942017243E-16 ) ) ;
#2232 = ORIENTED_EDGE ( 'NONE', *, *, #3090, .T. ) ;
#2233 = AXIS2_PLACEMENT_3D ( 'NONE', #21913, #12300, #29127 ) ;
#2234 = EDGE_CURVE ( 'NONE', #29242, #170, #14064, .T. ) ;
#2235 = B_SPLINE_CURVE_WITH_KNOTS ( 'NONE', 5,
 ( #16448, #30469, #21174, #11578, #18648, #2138 ),
 .UNSPECIFIED., .F., .F.,
 ( 6, 6 ),
 ( -2.300779731029999997, 0.000000000000000000 ),
 .UNSPECIFIED. ) ;
#2236 = CARTESIAN_POINT ( 'NONE',  ( 6.086077541567210147, 0.7980478301550381071, -5.626979598400000171 ) ) ;
#2237 = CARTESIAN_POINT ( 'NONE',  ( -3.052438874386664835, 3.509528713898347974, -28.58728588869999143 ) ) ;
#2238 = CIRCLE ( 'NONE', #19816, 27.50000000000000000 ) ;
#2239 = DIRECTION ( 'NONE',  ( -0.000000000000000000, 1.000000000000000000, -2.255973188440000244E-12 ) ) ;
#2240 = EDGE_CURVE ( 'NONE', #10529, #27389, #10891, .T. ) ;
#2241 = DIRECTION ( 'NONE',  ( 0.000000000000000000, -1.000000000000000000, 0.000000000000000000 ) ) ;
#2242 = CARTESIAN_POINT ( 'NONE',  ( 24.96253706050071131, 13.75225324050492581, 5.310538874999992665 ) ) ;
#2243 = CARTESIAN_POINT ( 'NONE',  ( -25.40918998211758861, 12.90916337393047009, 5.498574322615646714 ) ) ;
#2244 = CARTESIAN_POINT ( 'NONE',  ( -4.430040892179083478, 1.363067613765873931, -22.32289663399999924 ) ) ;
#2245 = CARTESIAN_POINT ( 'NONE',  ( 23.85073401102529900, -14.28298790920352879, 5.558590095350946392 ) ) ;
#2246 = CARTESIAN_POINT ( 'NONE',  ( 7.557678206131123844, -6.153726849708399449, -34.47779604538695253 ) ) ;
#2247 = CARTESIAN_POINT ( 'NONE',  ( -26.57440607989999748, -3.469982107200002108, -1.399999999999998579 ) ) ;
#2248 = VERTEX_POINT ( 'NONE', #11694 ) ;
#2249 = VERTEX_POINT ( 'NONE', #14377 ) ;
#2250 = DIRECTION ( 'NONE',  ( 0.000000000000000000, -0.9128796883888953273, 0.4082287037029526666 ) ) ;
#2251 = CARTESIAN_POINT ( 'NONE',  ( 28.50000000000000000, -3.490128108379999702E-15, 190.0000000000000000 ) ) ;
#2252 = ORIENTED_EDGE ( 'NONE', *, *, #4611, .T. ) ;
#2253 = FACE_OUTER_BOUND ( 'NONE', #30967, .T. ) ;
#2254 = DIRECTION ( 'NONE',  ( 0.000000000000000000, 0.9396926207858125046, 0.3420201433259318358 ) ) ;
#2255 = VECTOR ( 'NONE', #24072, 1000.000000000000000 ) ;
#2256 = EDGE_LOOP ( 'NONE', ( #634, #29786, #11374, #18353 ) ) ;
#2257 = VECTOR ( 'NONE', #29780, 1000.000000000000000 ) ;
#2258 = VERTEX_POINT ( 'NONE', #26478 ) ;
#2259 = ORIENTED_EDGE ( 'NONE', *, *, #7317, .T. ) ;
#2260 = AXIS2_PLACEMENT_3D ( 'NONE', #19061, #9302, #31021 ) ;
#2261 = SURFACE_SIDE_STYLE ('',( #21449 ) ) ;
#2262 = CIRCLE ( 'NONE', #9195, 5.792819795729999832 ) ;
#2263 = ORIENTED_EDGE ( 'NONE', *, *, #25435, .F. ) ;
#2264 = CARTESIAN_POINT ( 'NONE',  ( 26.80000000069999899, -3.281945028320000125E-15, 37.11018146769999504 ) ) ;
#2265 = CARTESIAN_POINT ( 'NONE',  ( 14.09657531829999932, 28.30410039250000054, 222.0000000000000000 ) ) ;
#2266 = CARTESIAN_POINT ( 'NONE',  ( -28.50000000000000000, 1.776356839399999922E-14, 222.0000000000000000 ) ) ;
#2267 = ADVANCED_FACE ( 'NONE', ( #12150 ), #16414, .F. ) ;
#2268 = EDGE_LOOP ( 'NONE', ( #3914, #1479, #3538, #12148 ) ) ;
#2269 = DIRECTION ( 'NONE',  ( 1.000000000000000000, 0.000000000000000000, 0.000000000000000000 ) ) ;
#2270 = DIRECTION ( 'NONE',  ( -3.924189347185961537E-12, 0.4082287037029530552, 0.9128796883888952163 ) ) ;
#2271 = CARTESIAN_POINT ( 'NONE',  ( 27.79999999999999716, -0.8519342421209999960, 222.0000000000000000 ) ) ;
#2272 =( GEOMETRIC_REPRESENTATION_CONTEXT ( 3 ) GLOBAL_UNCERTAINTY_ASSIGNED_CONTEXT ( ( #574 ) ) GLOBAL_UNIT_ASSIGNED_CONTEXT ( ( #26475, #6972, #21757 ) ) REPRESENTATION_CONTEXT ( 'NONE', 'WORKASPACE' ) );
#2273 = DIRECTION ( 'NONE',  ( 1.000000000000000000, 0.000000000000000000, 0.000000000000000000 ) ) ;
#2274 = ORIENTED_EDGE ( 'NONE', *, *, #16284, .F. ) ;
#2275 = CARTESIAN_POINT ( 'NONE',  ( -24.35520125494996435, 11.39272192119609706, -1.399999999999998801 ) ) ;
#2276 = CARTESIAN_POINT ( 'NONE',  ( -3.283272085064022239, -5.616145207998583189, -15.08182079290000566 ) ) ;
#2277 = FACE_OUTER_BOUND ( 'NONE', #27313, .T. ) ;
#2278 = DIRECTION ( 'NONE',  ( 0.000000000000000000, 0.000000000000000000, 1.000000000000000000 ) ) ;
#2279 = ORIENTED_EDGE ( 'NONE', *, *, #17209, .F. ) ;
#2280 = B_SPLINE_CURVE_WITH_KNOTS ( 'NONE', 3,
 ( #9784, #15895, #15421, #20453, #18079, #8024 ),
 .UNSPECIFIED., .F., .F.,
 ( 4, 2, 4 ),
 ( 0.000000000000000000, 0.5000000000000000000, 1.000000000000000000 ),
 .UNSPECIFIED. ) ;
#2281 = CARTESIAN_POINT ( 'NONE',  ( -23.74433668060337155, -14.45919608462527606, 3.899998580999992193 ) ) ;
#2282 = CARTESIAN_POINT ( 'NONE',  ( 1.568292632099254291, -27.75603058367145692, 4.689797669000017599 ) ) ;
#2283 = AXIS2_PLACEMENT_3D ( 'NONE', #10910, #25547, #27579 ) ;
#2284 = CARTESIAN_POINT ( 'NONE',  ( 20.30396079652883756, 20.00000000004620304, 1.000000000000000888 ) ) ;
#2285 = DIRECTION ( 'NONE',  ( -1.000000000000000000, 0.000000000000000000, 0.000000000000000000 ) ) ;
#2286 = CARTESIAN_POINT ( 'NONE',  ( 6.385918709376013247, 0.1527399656106667725, -64.06686508972499894 ) ) ;
#2287 = CARTESIAN_POINT ( 'NONE',  ( 9.999999999959999997, -24.92624923460000019, -26.23177046869999884 ) ) ;
#2288 = CARTESIAN_POINT ( 'NONE',  ( 4.638687372223567529, -9.716283825201511348, -32.74022090981630839 ) ) ;
#2289 = ORIENTED_EDGE ( 'NONE', *, *, #11138, .F. ) ;
#2290 = FACE_OUTER_BOUND ( 'NONE', #6182, .T. ) ;
#2291 = FACE_OUTER_BOUND ( 'NONE', #5378, .T. ) ;
#2292 = B_SPLINE_CURVE_WITH_KNOTS ( 'NONE', 5,
 ( #67, #9334, #4615, #9493, #11858, #19095, #14222, #23828, #28385, #28536, #16718, #28689, #2570, #21304, #7135 ),
 .UNSPECIFIED., .F., .F.,
 ( 6, 3, 3, 3, 6 ),
 ( 0.000000000000000000, 0.2999999999999999889, 0.5999999999977094767, 0.8999999999994273692, 1.000000000000000000 ),
 .UNSPECIFIED. ) ;
#2293 = CARTESIAN_POINT ( 'NONE',  ( 0.5797420292678476805, -4.971399746194223646, -68.10000000002500542 ) ) ;
#2294 = DIRECTION ( 'NONE',  ( 0.000000000000000000, 1.000000000000000000, 0.000000000000000000 ) ) ;
#2295 = AXIS2_PLACEMENT_3D ( 'NONE', #9813, #21621, #21773 ) ;
#2296 =( GEOMETRIC_REPRESENTATION_CONTEXT ( 3 ) GLOBAL_UNCERTAINTY_ASSIGNED_CONTEXT ( ( #10001 ) ) GLOBAL_UNIT_ASSIGNED_CONTEXT ( ( #15439, #3164, #8338 ) ) REPRESENTATION_CONTEXT ( 'NONE', 'WORKASPACE' ) );
#2297 = ADVANCED_FACE ( 'NONE', ( #16566 ), #31110, .F. ) ;
#2298 = DIRECTION ( 'NONE',  ( 0.000000000000000000, -1.000000000000000000, 0.000000000000000000 ) ) ;
#2299 = ORIENTED_EDGE ( 'NONE', *, *, #752, .F. ) ;
#2300 = CARTESIAN_POINT ( 'NONE',  ( 24.26927060809864400, 14.94229634074801361, 6.073751781078700951 ) ) ;
#2301 = CARTESIAN_POINT ( 'NONE',  ( 23.81866167241657806, 14.33570040768432996, 6.099998581000020792 ) ) ;
#2302 = ORIENTED_EDGE ( 'NONE', *, *, #16603, .T. ) ;
#2303 = EDGE_CURVE ( 'NONE', #25231, #6269, #9777, .T. ) ;
#2304 = CARTESIAN_POINT ( 'NONE',  ( -4.299999999899999814, -27.00000000000000000, -28.39999999989999679 ) ) ;
#2305 = CARTESIAN_POINT ( 'NONE',  ( -0.8249440165340113928, 4.504533947698903695, -60.25324387862499975 ) ) ;
#2306 = EDGE_LOOP ( 'NONE', ( #11495, #9641, #26655, #18802 ) ) ;
#2307 = CARTESIAN_POINT ( 'NONE',  ( -4.054393030549999999, -4.288653550910000334, 226.6412452697800006 ) ) ;
#2308 = CARTESIAN_POINT ( 'NONE',  ( 17.33115445884845229, -10.09718743895510151, -0.6999999999999783062 ) ) ;
#2309 = CARTESIAN_POINT ( 'NONE',  ( 9.999999999539999962, 19.99999999999999645, -42.42023091910999710 ) ) ;
#2310 = CARTESIAN_POINT ( 'NONE',  ( 8.700000000294076941, -9.763850040216345505, -36.23184806385972934 ) ) ;
#2311 = CARTESIAN_POINT ( 'NONE',  ( -10.69999999989999928, -30.49251257979999963, -21.04205368470000082 ) ) ;
#2312 = CARTESIAN_POINT ( 'NONE',  ( -2.813083154009999692E-14, -26.79999999949999889, 3.899999999999999911 ) ) ;
#2313 = ORIENTED_EDGE ( 'NONE', *, *, #26633, .T. ) ;
#2314 = CARTESIAN_POINT ( 'NONE',  ( 22.97695743748386832, 16.89262754991261062, 7.000000000000006217 ) ) ;
#2315 = EDGE_CURVE ( 'NONE', #16525, #8872, #29756, .T. ) ;
#2316 = CARTESIAN_POINT ( 'NONE',  ( 24.10531740749999940, -15.20475527630000023, 225.2083717279999746 ) ) ;
#2317 = CARTESIAN_POINT ( 'NONE',  ( 0.3163327506049999904, 12.29016939549999954, 232.6627643349999914 ) ) ;
#2318 = EDGE_CURVE ( 'NONE', #3529, #5952, #15658, .T. ) ;
#2319 = CARTESIAN_POINT ( 'NONE',  ( -25.27355175290000133, 12.75978488059999805, 223.3999999999999773 ) ) ;
#2320 = DIRECTION ( 'NONE',  ( -0.000000000000000000, 1.000000000000000000, -2.258510841069999963E-12 ) ) ;
#2321 = CARTESIAN_POINT ( 'NONE',  ( -1.087696845100000198, -27.77899371300000197, 225.2081166120000262 ) ) ;
#2322 = CYLINDRICAL_SURFACE ( 'NONE', #1652, 3.000000000000003553 ) ;
#2323 = CARTESIAN_POINT ( 'NONE',  ( -24.54884434681240890, 13.04717673402245914, 3.997190761000024573 ) ) ;
#2324 = CARTESIAN_POINT ( 'NONE',  ( 2.000000000000000000, -0.2617993877991515728, 227.6412452702004430 ) ) ;
#2325 = PRODUCT_DEFINITION ( 'UNKNOWN', '', #16358, #30748 ) ;
#2326 = DIRECTION ( 'NONE',  ( -1.000000000000000000, -2.587524353642439916E-24, -2.257144471329210308E-12 ) ) ;
#2327 = CARTESIAN_POINT ( 'NONE',  ( 17.70481771267368032, -8.030294603601026537, -0.6999999999999785283 ) ) ;
#2328 = CARTESIAN_POINT ( 'NONE',  ( -7.861312627709997614, 3.765626869335708449, -39.31578811167678111 ) ) ;
#2329 = ORIENTED_EDGE ( 'NONE', *, *, #23249, .T. ) ;
#2330 = CARTESIAN_POINT ( 'NONE',  ( -17.49999999969999820, -32.00000000000000000, -31.28675134614999820 ) ) ;
#2331 = ORIENTED_EDGE ( 'NONE', *, *, #18288, .T. ) ;
#2332 = CARTESIAN_POINT ( 'NONE',  ( 5.318140750225764712, 1.569125161463077900, -36.53159726779999517 ) ) ;
#2333 = EDGE_CURVE ( 'NONE', #23754, #8842, #22384, .T. ) ;
#2334 = CARTESIAN_POINT ( 'NONE',  ( 4.332295931058598448, 4.388630459628991787, -58.18805965152500193 ) ) ;
#2335 = ORIENTED_EDGE ( 'NONE', *, *, #28038, .F. ) ;
#2336 = ORIENTED_EDGE ( 'NONE', *, *, #2412, .T. ) ;
#2337 = CARTESIAN_POINT ( 'NONE',  ( -15.73360964030186970, 11.02001161816959396, -0.6999999999999784173 ) ) ;
#2338 = VERTEX_POINT ( 'NONE', #27096 ) ;
#2339 = EDGE_CURVE ( 'NONE', #17478, #24321, #19694, .T. ) ;
#2340 = DIRECTION ( 'NONE',  ( 0.000000000000000000, 0.7113488923935510355, -0.7028390664230811380 ) ) ;
#2341 = LINE ( 'NONE', #26253, #30023 ) ;
#2342 = B_SPLINE_CURVE_WITH_KNOTS ( 'NONE', 1,
 ( #29544, #3262 ),
 .UNSPECIFIED., .F., .F.,
 ( 2, 2 ),
 ( -2.556026448610000073E-06, 0.7000000000009999335 ),
 .UNSPECIFIED. ) ;
#2344 = CARTESIAN_POINT ( 'NONE',  ( 9.000000000029999114, 21.69999999990000106, -70.09999999999999432 ) ) ;
#2343 = B_SPLINE_CURVE_WITH_KNOTS ( 'NONE', 3,
 ( #14729, #10007, #24323, #22271, #10320, #17080, #28888, #19605, #16923, #26680, #7338, #5286 ),
 .UNSPECIFIED., .F., .F.,
 ( 4, 2, 2, 2, 2, 4 ),
 ( 0.000000000000000000, 0.2499999999999773515, 0.3749999999999896749, 0.5000000000000019984, 0.7500000000000009992, 1.000000000000000000 ),
 .UNSPECIFIED. ) ;
#2345 = CARTESIAN_POINT ( 'NONE',  ( 23.47715715134837211, -20.00370206646827498, 1.000000000000000888 ) ) ;
#2346 = CARTESIAN_POINT ( 'NONE',  ( -20.30403093128963476, 20.00000000003735323, 2.200000064000007249 ) ) ;
#2347 = CARTESIAN_POINT ( 'NONE',  ( -1.831588579526997940, 3.958388136463042439, -7.731725184300007214 ) ) ;
#2348 = CARTESIAN_POINT ( 'NONE',  ( 24.72074161949999649, -14.16756531389999907, 230.6999999999999886 ) ) ;
#2349 = ORIENTED_EDGE ( 'NONE', *, *, #1167, .T. ) ;
#2350 = CARTESIAN_POINT ( 'NONE',  ( -24.10559463919999956, -15.20494734660000091, 224.7915671760000009 ) ) ;
#2351 = EDGE_CURVE ( 'NONE', #8650, #53, #9956, .T. ) ;
#2352 = CARTESIAN_POINT ( 'NONE',  ( 3.931047123110464891, -1.876836795983964912, -21.38180150030001059 ) ) ;
#2353 = CARTESIAN_POINT ( 'NONE',  ( 2.020725942159999899, 3.500000000000000000, 230.5235986622430175 ) ) ;
#2354 = DIRECTION ( 'NONE',  ( -1.224606353819999829E-16, -1.000000000000000000, 0.000000000000000000 ) ) ;
#2355 = ADVANCED_FACE ( 'NONE', ( #22224 ), #17490, .F. ) ;
#2356 = LINE ( 'NONE', #16655, #3079 ) ;
#2357 = CARTESIAN_POINT ( 'NONE',  ( 8.700000000235821318, -29.73863906516063693, -27.17531388883607590 ) ) ;
#2358 = PRODUCT_DEFINITION ( 'UNKNOWN', '', #14869, #22583 ) ;
#2359 = CARTESIAN_POINT ( 'NONE',  ( 3.248659393266399409, -2.157825791482659294, -43.35875473022499449 ) ) ;
#2360 = CARTESIAN_POINT ( 'NONE',  ( 9.499999999611546286, -18.04864474152872589, -34.59380650643552713 ) ) ;
#2361 = CARTESIAN_POINT ( 'NONE',  ( 1.638687372170419598, -20.50181238077955470, -27.47976714835314738 ) ) ;
#2362 = CARTESIAN_POINT ( 'NONE',  ( -0.1113126277332136399, -3.273367579602823429, -37.55154403890800552 ) ) ;
#2363 = CARTESIAN_POINT ( 'NONE',  ( 8.999999999770000869, 21.53714677049999793, -44.32440694871200293 ) ) ;
#2364 = ORIENTED_EDGE ( 'NONE', *, *, #17787, .T. ) ;
#2365 = CARTESIAN_POINT ( 'NONE',  ( 5.999999999999997335, -17.49802621104079137, -75.24709024819303238 ) ) ;
#2366 = EDGE_CURVE ( 'NONE', #3831, #19704, #12772, .T. ) ;
#2367 = CARTESIAN_POINT ( 'NONE',  ( 17.16657240420000008, 11.00000000000000355, -0.8000000000000020428 ) ) ;
#2368 = ORIENTED_EDGE ( 'NONE', *, *, #11363, .T. ) ;
#2369 = CARTESIAN_POINT ( 'NONE',  ( -5.861312627756135818, -5.597492073868338025, -34.74908987245776615 ) ) ;
#2370 = CARTESIAN_POINT ( 'NONE',  ( -0.5560430376289927645, 4.887756486939889733, -49.01410749632500341 ) ) ;
#2371 = ORIENTED_EDGE ( 'NONE', *, *, #18259, .T. ) ;
#2372 = ORIENTED_EDGE ( 'NONE', *, *, #6912, .F. ) ;
#2373 = VECTOR ( 'NONE', #6541, 1000.000000000000000 ) ;
#2374 = EDGE_CURVE ( 'NONE', #10752, #5681, #11247, .T. ) ;
#2375 = VERTEX_POINT ( 'NONE', #19713 ) ;
#2376 = CARTESIAN_POINT ( 'NONE',  ( -17.28486482095781085, -10.01258675972073675, 0.000000000000000000 ) ) ;
#2377 = ORIENTED_EDGE ( 'NONE', *, *, #7334, .T. ) ;
#2378 = CARTESIAN_POINT ( 'NONE',  ( 24.22190007760000086, -15.01852807150000046, 225.6806946080000102 ) ) ;
#2379 = CARTESIAN_POINT ( 'NONE',  ( 10.69999999999999929, -127.2537437101000108, -34.36317024011000143 ) ) ;
#2380 = EDGE_CURVE ( 'NONE', #15181, #14446, #21198, .T. ) ;
#2381 = DIRECTION ( 'NONE',  ( 0.000000000000000000, 0.000000000000000000, -1.000000000000000000 ) ) ;
#2382 = CARTESIAN_POINT ( 'NONE',  ( 0.5467022973628515858, 4.692255042463733261, -35.69999999999998863 ) ) ;
#2383 = CARTESIAN_POINT ( 'NONE',  ( 19.19680082505102447, 20.00027389960937185, -0.4288677566865453650 ) ) ;
#2384 = FACE_OUTER_BOUND ( 'NONE', #17339, .T. ) ;
#2385 = CARTESIAN_POINT ( 'NONE',  ( -27.23548386990000125, 3.335274659649999582E-15, 138.3395398259999922 ) ) ;
#2386 = CARTESIAN_POINT ( 'NONE',  ( 1.776356839399999804E-15, -5.329070518200000398E-15, 224.6412452697800290 ) ) ;
#2387 = EDGE_LOOP ( 'NONE', ( #6499, #20813, #11864, #16053 ) ) ;
#2388 = CARTESIAN_POINT ( 'NONE',  ( 0.5074138422395748638, -6.503547975687064664, -9.993384211800002248 ) ) ;
#2389 = CARTESIAN_POINT ( 'NONE',  ( -1.611722395286938170, -6.291674585240492057, -26.94882611460000632 ) ) ;
#2390 = LINE ( 'NONE', #11670, #11281 ) ;
#2391 = DIRECTION ( 'NONE',  ( -1.000000000000000000, 0.000000000000000000, -2.257144471330000330E-12 ) ) ;
#2392 = CARTESIAN_POINT ( 'NONE',  ( 8.261799387612766665, -15.86465192213917064, -74.65259062561659675 ) ) ;
#2393 = CARTESIAN_POINT ( 'NONE',  ( 2.326244606069574505, 3.379075471592551949, -17.21259163650000446 ) ) ;
#2394 = AXIS2_PLACEMENT_3D ( 'NONE', #6785, #16381, #4577 ) ;
#2395 = FACE_OUTER_BOUND ( 'NONE', #22755, .T. ) ;
#2396 = CARTESIAN_POINT ( 'NONE',  ( 7.638687372242944029, -5.784297784966613065, -34.65797863942491830 ) ) ;
#2397 = FACE_OUTER_BOUND ( 'NONE', #6665, .T. ) ;
#2398 = VERTEX_POINT ( 'NONE', #7588 ) ;
#2399 = DIRECTION ( 'NONE',  ( -1.000000000000000000, 5.687697999151106851E-16, -6.771501495036750356E-12 ) ) ;
#2400 = CARTESIAN_POINT ( 'NONE',  ( -12.39224864153120720, -31.99999999999999289, -27.17394816745003894 ) ) ;
#2401 = ORIENTED_EDGE ( 'NONE', *, *, #28748, .F. ) ;
#2402 = B_SPLINE_CURVE_WITH_KNOTS ( 'NONE', 3,
 ( #12371, #5441, #19925, #5297, #24950, #17240 ),
 .UNSPECIFIED., .F., .F.,
 ( 4, 2, 4 ),
 ( 0.000000000000000000, 0.5000000000000000000, 1.000000000000000000 ),
 .UNSPECIFIED. ) ;
#2403 = B_SPLINE_CURVE_WITH_KNOTS ( 'NONE', 3,
 ( #15394, #22486, #12882, #3429, #15544, #10673 ),
 .UNSPECIFIED., .F., .F.,
 ( 4, 2, 4 ),
 ( 0.000000000000000000, 0.5000000000000000000, 1.000000000000000000 ),
 .UNSPECIFIED. ) ;
#2404 = DIRECTION ( 'NONE',  ( 3.924189347185962345E-12, -0.4082287037029530552, -0.9128796883888953273 ) ) ;
#2405 = CARTESIAN_POINT ( 'NONE',  ( 18.95046173579999760, -18.95046173579999760, 43.21714158840000408 ) ) ;
#2406 = EDGE_CURVE ( 'NONE', #30214, #27320, #10267, .T. ) ;
#2407 = ORIENTED_EDGE ( 'NONE', *, *, #7790, .F. ) ;
#2408 = VERTEX_POINT ( 'NONE', #17181 ) ;
#2409 = ORIENTED_EDGE ( 'NONE', *, *, #20417, .F. ) ;
#2410 = ORIENTED_EDGE ( 'NONE', *, *, #6772, .T. ) ;
#2411 = FACE_OUTER_BOUND ( 'NONE', #12174, .T. ) ;
#2412 = EDGE_CURVE ( 'NONE', #16, #8184, #25150, .T. ) ;
#2413 = ADVANCED_FACE ( 'NONE', ( #530 ), #18170, .F. ) ;
#2414 = CARTESIAN_POINT ( 'NONE',  ( 28.49999999970000175, 10.47094317839999889, 222.0000000000000000 ) ) ;
#2415 = CYLINDRICAL_SURFACE ( 'NONE', #4772, 2.100000000000000977 ) ;
#2416 = ORIENTED_EDGE ( 'NONE', *, *, #3677, .T. ) ;
#2417 = DIRECTION ( 'NONE',  ( -1.000000000000000000, 0.000000000000000000, -2.257144471330000330E-12 ) ) ;
#2418 = AXIS2_PLACEMENT_3D ( 'NONE', #14565, #31084, #26819 ) ;
#2419 = LINE ( 'NONE', #9962, #9011 ) ;
#2420 = FACE_OUTER_BOUND ( 'NONE', #9603, .T. ) ;
#2421 = CARTESIAN_POINT ( 'NONE',  ( 3.030289999311443161, -3.940603520075978139, -0.6999848558563146472 ) ) ;
#2422 = EDGE_LOOP ( 'NONE', ( #30105, #6247, #24854, #29914 ) ) ;
#2423 = CARTESIAN_POINT ( 'NONE',  ( -18.82786841510930742, 20.00005837762122241, -0.5634673906915752539 ) ) ;
#2424 = CARTESIAN_POINT ( 'NONE',  ( -3.283272085064022239, -5.616145207998583189, -15.68182079290000175 ) ) ;
#2425 = FACE_BOUND ( 'NONE', #238, .T. ) ;
#2426 = CARTESIAN_POINT ( 'NONE',  ( -27.76135144349999706, 3.399672736839999702E-15, 142.3385858900000187 ) ) ;
#2427 = ORIENTED_EDGE ( 'NONE', *, *, #17591, .T. ) ;
#2428 = CARTESIAN_POINT ( 'NONE',  ( 16.40303402075260308, 10.20816091466531716, -0.6999999999999784173 ) ) ;
#2429 = CARTESIAN_POINT ( 'NONE',  ( 12.51136270434944109, 21.69999999994217532, -69.72111648971724662 ) ) ;
#2430 = DIRECTION ( 'NONE',  ( -1.000000000000000000, 5.687697999151106851E-16, -6.771501495036750356E-12 ) ) ;
#2431 = AXIS2_PLACEMENT_3D ( 'NONE', #27211, #9402, #20749 ) ;
#2432 = B_SPLINE_CURVE_WITH_KNOTS ( 'NONE', 3,
 ( #19714, #2564, #21611, #14683, #5225, #7127 ),
 .UNSPECIFIED., .F., .F.,
 ( 4, 2, 4 ),
 ( 0.000000000000000000, 0.5000000000000000000, 1.000000000000000000 ),
 .UNSPECIFIED. ) ;
#2433 = DIRECTION ( 'NONE',  ( -1.000000000000000000, 0.000000000000000000, 0.000000000000000000 ) ) ;
#2434 = CARTESIAN_POINT ( 'NONE',  ( 9.999999999969999109, -29.12127062269999911, -30.52127062070000107 ) ) ;
#2435 = DIRECTION ( 'NONE',  ( 0.000000000000000000, 0.000000000000000000, 1.000000000000000000 ) ) ;
#2436 = CARTESIAN_POINT ( 'NONE',  ( -8.990816569130000602, -15.87649056320000085, 230.6999999999999886 ) ) ;
#2437 = VERTEX_POINT ( 'NONE', #29293 ) ;
#2438 = ADVANCED_FACE ( 'NONE', ( #3322 ), #12927, .T. ) ;
#2439 = CARTESIAN_POINT ( 'NONE',  ( -9.999999999909999104, -25.00000000000000000, -2.399999999999999467 ) ) ;
#2440 = DIRECTION ( 'NONE',  ( 0.000000000000000000, 0.3420201433259318913, -0.9396926207858126157 ) ) ;
#2441 = EDGE_CURVE ( 'NONE', #1750, #26472, #30812, .T. ) ;
#2442 = VECTOR ( 'NONE', #2526, 1000.000000000000114 ) ;
#2443 = CARTESIAN_POINT ( 'NONE',  ( 2.062924749200377939, -4.402521781607152462, -68.10000000002503384 ) ) ;
#2444 = DIRECTION ( 'NONE',  ( 0.000000000000000000, 2.257157423930000049E-12, 1.000000000000000000 ) ) ;
#2445 = ORIENTED_EDGE ( 'NONE', *, *, #24054, .T. ) ;
#2446 = DIRECTION ( 'NONE',  ( 0.000000000000000000, -1.000000000000000000, 0.000000000000000000 ) ) ;
#2447 =( LENGTH_UNIT ( ) NAMED_UNIT ( * ) SI_UNIT ( .MILLI., .METRE. ) );
#2448 = EDGE_LOOP ( 'NONE', ( #6764, #479, #13207, #29754 ) ) ;
#2449 = CARTESIAN_POINT ( 'NONE',  ( 23.81776757409229361, 15.65134803726813217, 4.999998581000003384 ) ) ;
#2450 = CARTESIAN_POINT ( 'NONE',  ( -1.449312944839809658, 3.998683954144026220, -69.55099036452500627 ) ) ;
#2451 = ORIENTED_EDGE ( 'NONE', *, *, #7138, .F. ) ;
#2452 = CARTESIAN_POINT ( 'NONE',  ( -1.151230282303593366, -4.494053275198268693, -27.54882611460000774 ) ) ;
#2453 = DIRECTION ( 'NONE',  ( 3.590123367689346428E-13, 0.9128796883888948832, -0.4082287037029536658 ) ) ;
#2454 = AXIS2_PLACEMENT_3D ( 'NONE', #4821, #14417, #3027 ) ;
#2455 = CARTESIAN_POINT ( 'NONE',  ( 4.315256771988532414, 1.538274589489400990, -45.92627377572499370 ) ) ;
#2456 = CARTESIAN_POINT ( 'NONE',  ( 8.000000000368686415, -24.05737431370143398, -27.69631922065391905 ) ) ;
#2457 = LINE ( 'NONE', #31092, #18574 ) ;
#2458 = CARTESIAN_POINT ( 'NONE',  ( 24.09856112909999837, -15.21545593799999985, 224.8958160969999938 ) ) ;
#2459 = CARTESIAN_POINT ( 'NONE',  ( 8.700000000285857737, -13.61366271048277277, -34.64064744186795508 ) ) ;
#2460 = CIRCLE ( 'NONE', #29580, 26.80000000000000071 ) ;
#2461 = CARTESIAN_POINT ( 'NONE',  ( 9.999999999959799268, -29.23060343765324731, -26.39054106487359164 ) ) ;
#2462 = ORIENTED_EDGE ( 'NONE', *, *, #1742, .T. ) ;
#2463 = CARTESIAN_POINT ( 'NONE',  ( -26.84464183999999776, 3.287411896330000120E-15, 192.5624961750000068 ) ) ;
#2464 = EDGE_CURVE ( 'NONE', #27585, #21516, #11649, .T. ) ;
#2465 = CARTESIAN_POINT ( 'NONE',  ( 4.334836395473461224, -2.879286697580460519, -35.69999999999999574 ) ) ;
#2466 = CARTESIAN_POINT ( 'NONE',  ( -11.54682818539999900, -3.657609505980000009, 231.9999989789999972 ) ) ;
#2467 = CARTESIAN_POINT ( 'NONE',  ( -27.79999999990000248, 4.328052761039999474, 222.0000000000000000 ) ) ;
#2468 = CARTESIAN_POINT ( 'NONE',  ( -13.00000000000000000, 23.81663212713006672, -62.33813991915980779 ) ) ;
#2469 = CARTESIAN_POINT ( 'NONE',  ( 10.69999999999454232, -129.9401694263537479, -39.98253760374566923 ) ) ;
#2470 = CARTESIAN_POINT ( 'NONE',  ( 24.34609883811560849, -13.42112775176797612, 224.0360482199137380 ) ) ;
#2471 = CARTESIAN_POINT ( 'NONE',  ( -25.12046394328327281, 13.46291001840482160, 3.957489296000010981 ) ) ;
#2472 = CARTESIAN_POINT ( 'NONE',  ( 0.2617993877991493523, 1.999999999999999556, 227.6412452700154176 ) ) ;
#2473 = EDGE_CURVE ( 'NONE', #7813, #4043, #1545, .T. ) ;
#2474 = AXIS2_PLACEMENT_3D ( 'NONE', #5283, #7335, #24478 ) ;
#2475 = B_SPLINE_SURFACE_WITH_KNOTS ( 'NONE', 5, 1, ( 
 ( #9573, #21220 ),
 ( #30821, #28297 ),
 ( #2345, #18314 ),
 ( #11929, #26413 ),
 ( #2035, #24056 ),
 ( #14145, #23445 ),
 ( #19171, #18858 ),
 ( #16342, #4387 ),
 ( #30976, #23910 ) ),
 .UNSPECIFIED., .F., .F., .F.,
 ( 6, 3, 6 ),
 ( 2, 2 ),
 ( 0.000000000000000000, 53.95537973340000093, 92.42745556099998794 ),
 ( -3.500000000000000000, 3.500000000000000000 ),
 .UNSPECIFIED. ) ;
#2476 = CARTESIAN_POINT ( 'NONE',  ( 2.846903786944921855, -11.76275999642770742, 232.0000002394077399 ) ) ;
#2477 = CARTESIAN_POINT ( 'NONE',  ( 17.82602571118884427, -8.107840965023857649, -0.6999999999999783062 ) ) ;
#2478 = CYLINDRICAL_SURFACE ( 'NONE', #7762, 1.100000000000002309 ) ;
#2479 = ORIENTED_EDGE ( 'NONE', *, *, #11146, .T. ) ;
#2480 = DIRECTION ( 'NONE',  ( -1.000000000000000000, 0.000000000000000000, -2.257144471330000330E-12 ) ) ;
#2481 = CIRCLE ( 'NONE', #494, 3.999999999669999973 ) ;
#2482 = ORIENTED_EDGE ( 'NONE', *, *, #14035, .F. ) ;
#2483 = DIRECTION ( 'NONE',  ( -1.000000000000000000, 0.000000000000000000, 0.000000000000000000 ) ) ;
#2484 = VECTOR ( 'NONE', #18932, 1000.000000000000000 ) ;
#2485 = ADVANCED_FACE ( 'NONE', ( #28609 ), #1715, .F. ) ;
#2486 = CARTESIAN_POINT ( 'NONE',  ( 0.8945918243927832858, -4.819150861182647461, -58.74125695792500323 ) ) ;
#2487 = VERTEX_POINT ( 'NONE', #30968 ) ;
#2488 = ORIENTED_EDGE ( 'NONE', *, *, #30930, .F. ) ;
#2489 = CARTESIAN_POINT ( 'NONE',  ( -20.30396346370000060, 20.00000000000000000, 229.0000000000000000 ) ) ;
#2490 = ORIENTED_EDGE ( 'NONE', *, *, #28681, .T. ) ;
#2491 = ADVANCED_FACE ( 'NONE', ( #22681 ), #20621, .F. ) ;
#2492 = CARTESIAN_POINT ( 'NONE',  ( 27.63418825910000010, 8.886057489849999769, 229.0000000000000000 ) ) ;
#2493 = LINE ( 'NONE', #12080, #28070 ) ;
#2494 = FACE_BOUND ( 'NONE', #9502, .T. ) ;
#2495 = CARTESIAN_POINT ( 'NONE',  ( 10.79542655330000045, -5.882779935969999485, 232.6627648150000027 ) ) ;
#2496 = CARTESIAN_POINT ( 'NONE',  ( 0.000000000000000000, 0.000000000000000000, -44.00000000000000000 ) ) ;
#2497 = CARTESIAN_POINT ( 'NONE',  ( 3.530284718056032833, 5.524446756132658898, -5.200967428500000267 ) ) ;
#2498 = DIRECTION ( 'NONE',  ( 0.000000000000000000, 0.000000000000000000, 1.000000000000000000 ) ) ;
#2499 = VERTEX_POINT ( 'NONE', #30665 ) ;
#2500 = DIRECTION ( 'NONE',  ( 0.000000000000000000, -1.000000000000000000, 0.000000000000000000 ) ) ;
#2501 = AXIS2_PLACEMENT_3D ( 'NONE', #22301, #27019, #5916 ) ;
#2502 = CARTESIAN_POINT ( 'NONE',  ( 3.791027721911684800, -3.577548591872723449, -19.03565261000001385 ) ) ;
#2503 = CARTESIAN_POINT ( 'NONE',  ( 8.999999999770000869, 20.99999999999999645, -60.10000000000000142 ) ) ;
#2504 = AXIS2_PLACEMENT_3D ( 'NONE', #19203, #7396, #28789 ) ;
#2505 = CARTESIAN_POINT ( 'NONE',  ( 24.63375101535647360, -12.88633855010671247, 5.901400366999986602 ) ) ;
#2506 = CARTESIAN_POINT ( 'NONE',  ( 0.000000000000000000, 0.000000000000000000, 20.00000000000000355 ) ) ;
#2507 = DIRECTION ( 'NONE',  ( 0.000000000000000000, 1.000000000000000000, 0.000000000000000000 ) ) ;
#2508 = CARTESIAN_POINT ( 'NONE',  ( -20.28771362240119913, 20.00000013994726089, 0.7458731309999966363 ) ) ;
#2509 = EDGE_CURVE ( 'NONE', #5262, #15947, #26159, .T. ) ;
#2510 = CARTESIAN_POINT ( 'NONE',  ( 3.378474373710000034, 11.51459555979999827, 232.0000000000000000 ) ) ;
#2511 = CARTESIAN_POINT ( 'NONE',  ( 24.07552309629999954, -13.90001137829999855, 226.1000014189999945 ) ) ;
#2512 = DIRECTION ( 'NONE',  ( 0.000000000000000000, 0.000000000000000000, 1.000000000000000000 ) ) ;
#2513 = FACE_OUTER_BOUND ( 'NONE', #8026, .T. ) ;
#2514 = ORIENTED_EDGE ( 'NONE', *, *, #22485, .F. ) ;
#2515 = B_SPLINE_CURVE_WITH_KNOTS ( 'NONE', 3,
 ( #4871, #10058, #7677, #23925, #12407, #475 ),
 .UNSPECIFIED., .F., .F.,
 ( 4, 2, 4 ),
 ( 0.000000000000000000, 0.5000000000000000000, 1.000000000000000000 ),
 .UNSPECIFIED. ) ;
#2516 = CARTESIAN_POINT ( 'NONE',  ( -4.273414424137721213, 4.913340199448848367, -29.18728588869999641 ) ) ;
#2517 = CARTESIAN_POINT ( 'NONE',  ( 10.00000000070000183, -120.5233595624000174, -31.26042064949999855 ) ) ;
#2518 = ORIENTED_EDGE ( 'NONE', *, *, #6735, .F. ) ;
#2519 = EDGE_CURVE ( 'NONE', #9043, #24060, #14239, .T. ) ;
#2520 = CARTESIAN_POINT ( 'NONE',  ( 24.95427444975690889, -13.76797447160702070, 3.899998581000013509 ) ) ;
#2521 = CARTESIAN_POINT ( 'NONE',  ( -1.460566089872937789, -4.291843709425559261, -47.39520033292500045 ) ) ;
#2522 = ORIENTED_EDGE ( 'NONE', *, *, #26927, .T. ) ;
#2523 = VERTEX_POINT ( 'NONE', #13824 ) ;
#2524 = EDGE_CURVE ( 'NONE', #6267, #3589, #27162, .T. ) ;
#2525 = EDGE_LOOP ( 'NONE', ( #21481, #13778, #1991, #22145 ) ) ;
#2526 = DIRECTION ( 'NONE',  ( 0.000000000000000000, 0.3420201433259318358, -0.9396926207858125046 ) ) ;
#2527 = VERTEX_POINT ( 'NONE', #11771 ) ;
#2528 = CARTESIAN_POINT ( 'NONE',  ( -4.667733413579616908, -30.93201666723582122, 1.000000000000000888 ) ) ;
#2529 = FACE_OUTER_BOUND ( 'NONE', #4143, .T. ) ;
#2530 = CARTESIAN_POINT ( 'NONE',  ( 0.6438416807965144928, 4.176741662662551313, -35.69999999999999574 ) ) ;
#2531 = ADVANCED_FACE ( 'NONE', ( #29917 ), #30167, .T. ) ;
#2532 = CARTESIAN_POINT ( 'NONE',  ( -8.699999999662093586, -15.94902145834643115, -35.53273252493492862 ) ) ;
#2533 = CARTESIAN_POINT ( 'NONE',  ( -24.90302310912370132, 13.86047864606265279, 6.098655051000018368 ) ) ;
#2534 = CARTESIAN_POINT ( 'NONE',  ( -4.909305965083425427, -9.106205312618326886, -33.03777608198690530 ) ) ;
#2535 = CARTESIAN_POINT ( 'NONE',  ( -8.999999999796672867, 20.89222690361001256, -44.57801334123718107 ) ) ;
#2536 = ORIENTED_EDGE ( 'NONE', *, *, #19938, .T. ) ;
#2537 = CARTESIAN_POINT ( 'NONE',  ( -6.277996069133942925, 1.777976852108807737, -7.310827254900003069 ) ) ;
#2538 = CARTESIAN_POINT ( 'NONE',  ( -4.273414424137721213, 4.913340199448848367, -28.58728588869999143 ) ) ;
#2539 = DIRECTION ( 'NONE',  ( 0.000000000000000000, -0.9396926207858125046, -0.3420201433259318358 ) ) ;
#2540 = VECTOR ( 'NONE', #17749, 1000.000000000000114 ) ;
#2541 = ADVANCED_FACE ( 'NONE', ( #3629 ), #4226, .F. ) ;
#2542 = DIRECTION ( 'NONE',  ( 1.000000000000000000, -1.843431230200084908E-12, 2.650498504963248473E-12 ) ) ;
#2543 = DIRECTION ( 'NONE',  ( -1.000000000000000000, 0.000000000000000000, 0.000000000000000000 ) ) ;
#2544 = CARTESIAN_POINT ( 'NONE',  ( -23.30309534867867782, -14.60301215419051779, 225.4905541410415992 ) ) ;
#2545 = CARTESIAN_POINT ( 'NONE',  ( 5.420768140797370016, -26.96154273974102367, 20.68646079438196139 ) ) ;
#2546 = CARTESIAN_POINT ( 'NONE',  ( 2.914708617673698932, -3.631324690002109445, -3.105321867099997135 ) ) ;
#2547 = CARTESIAN_POINT ( 'NONE',  ( 16.51284149387604216, 10.10369150398561544, -1.400000000000001910 ) ) ;
#2548 = CARTESIAN_POINT ( 'NONE',  ( -23.87170005649112525, -14.24726900567271493, 3.904031772999999816 ) ) ;
#2549 = CARTESIAN_POINT ( 'NONE',  ( 16.19548821459394716, 11.53640331831526744, -4.336808689942018722E-16 ) ) ;
#2550 = ORIENTED_EDGE ( 'NONE', *, *, #5836, .T. ) ;
#2551 = ADVANCED_FACE ( 'NONE', ( #28140 ), #6578, .F. ) ;
#2552 = CARTESIAN_POINT ( 'NONE',  ( 17.93011078765611543, -8.208160914697428368, -0.6999999999999784173 ) ) ;
#2553 = CARTESIAN_POINT ( 'NONE',  ( -12.41253550773259562, -32.00000000000000000, -29.76654229695615683 ) ) ;
#2554 = VERTEX_POINT ( 'NONE', #9874 ) ;
#2555 = DIRECTION ( 'NONE',  ( 1.000000000000000000, 0.000000000000000000, 0.000000000000000000 ) ) ;
#2556 = DIRECTION ( 'NONE',  ( 0.000000000000000000, 0.000000000000000000, -1.000000000000000000 ) ) ;
#2557 = ORIENTED_EDGE ( 'NONE', *, *, #20470, .F. ) ;
#2558 = ORIENTED_EDGE ( 'NONE', *, *, #18694, .F. ) ;
#2559 = ORIENTED_EDGE ( 'NONE', *, *, #5934, .F. ) ;
#2560 =( NAMED_UNIT ( * ) SI_UNIT ( $, .STERADIAN. ) SOLID_ANGLE_UNIT ( ) );
#2561 = ORIENTED_EDGE ( 'NONE', *, *, #25280, .T. ) ;
#2562 = FACE_OUTER_BOUND ( 'NONE', #19509, .T. ) ;
#2563 = CARTESIAN_POINT ( 'NONE',  ( 14.09657531829999932, 28.30410039250000054, 229.0000000000000000 ) ) ;
#2564 = CARTESIAN_POINT ( 'NONE',  ( -7.799123028745747810, -5.730129976181659757, -27.37892452043196556 ) ) ;
#2565 = ORIENTED_EDGE ( 'NONE', *, *, #25565, .T. ) ;
#2566 = CARTESIAN_POINT ( 'NONE',  ( -24.83827471527357744, 12.48687850854618198, 4.999998581000003384 ) ) ;
#2567 = CARTESIAN_POINT ( 'NONE',  ( -4.276011752185619130, -110.9401521130015027, -1.050525799534463012 ) ) ;
#2568 = CARTESIAN_POINT ( 'NONE',  ( -13.92191802975810866, 20.99999999990301447, -67.88524365274894024 ) ) ;
#2569 = DIRECTION ( 'NONE',  ( 0.000000000000000000, 0.3420201433259318913, -0.9396926207858126157 ) ) ;
#2570 = CARTESIAN_POINT ( 'NONE',  ( 0.07063658732340000190, -28.50016343120000073, 226.0986540789999992 ) ) ;
#2571 = VERTEX_POINT ( 'NONE', #451 ) ;
#2572 = CARTESIAN_POINT ( 'NONE',  ( 9.738910687886868089, -24.96785170200598358, 115.0000000000000000 ) ) ;
#2573 = AXIS2_PLACEMENT_3D ( 'NONE', #24001, #2440, #18795 ) ;
#2574 = CARTESIAN_POINT ( 'NONE',  ( 5.782996427689181651, 1.709881257618839356, -17.54190840230000603 ) ) ;
#2575 = CARTESIAN_POINT ( 'NONE',  ( 18.05873143933198577, -9.659453306092730784, -0.6999999999999783062 ) ) ;
#2576 = B_SPLINE_CURVE_WITH_KNOTS ( 'NONE', 3,
 ( #4173, #18790, #11253, #21474, #16438, #9190 ),
 .UNSPECIFIED., .F., .F.,
 ( 4, 2, 4 ),
 ( 0.000000000000000000, 0.5000000000000000000, 1.000000000000000000 ),
 .UNSPECIFIED. ) ;
#2577 = EDGE_CURVE ( 'NONE', #6914, #4001, #2636, .T. ) ;
#2578 = CARTESIAN_POINT ( 'NONE',  ( 27.50000000000000000, -1.044349611129999949E-13, 0.000000000000000000 ) ) ;
#2579 = CARTESIAN_POINT ( 'NONE',  ( -12.36045835448409314, -28.65858880358294414, -33.21571233971392445 ) ) ;
#2580 = CARTESIAN_POINT ( 'NONE',  ( 10.99999999979999998, 20.99999999999999645, -58.51619795479999908 ) ) ;
#2581 = CARTESIAN_POINT ( 'NONE',  ( 27.51421515662130446, 9.168494879182089718, 1.000000000000000888 ) ) ;
#2582 = ADVANCED_FACE ( 'NONE', ( #21995 ), #16795, .F. ) ;
#2583 = EDGE_CURVE ( 'NONE', #2554, #19777, #7060, .T. ) ;
#2584 = CARTESIAN_POINT ( 'NONE',  ( -10.06596365874885812, -25.80632433378972124, 140.0000000000000000 ) ) ;
#2585 = CARTESIAN_POINT ( 'NONE',  ( -11.59065746630000149, -24.20066399839999960, -1.404983722500002807 ) ) ;
#2586 = CARTESIAN_POINT ( 'NONE',  ( -13.62111648911912631, 21.69999999994467998, -68.61136270525845759 ) ) ;
#2587 = EDGE_LOOP ( 'NONE', ( #8612, #16649, #27006, #22613, #16346, #29631 ) ) ;
#2588 = CARTESIAN_POINT ( 'NONE',  ( -10.69999999999999929, -24.59781467760000240, -30.21505918890000331 ) ) ;
#2589 = CARTESIAN_POINT ( 'NONE',  ( 1.746469154276752089, -4.581628552928044051, -68.10000000002500542 ) ) ;
#2590 = CARTESIAN_POINT ( 'NONE',  ( 15.51050023680984680, 10.97998838177520931, 0.05106179917585291356 ) ) ;
#2591 = ORIENTED_EDGE ( 'NONE', *, *, #25415, .T. ) ;
#2592 = CARTESIAN_POINT ( 'NONE',  ( 17.83929014045347827, 20.00000000006149392, -1.000005633855494125E-09 ) ) ;
#2593 = AXIS2_PLACEMENT_3D ( 'NONE', #3415, #27187, #12869 ) ;
#2594 = VERTEX_POINT ( 'NONE', #5140 ) ;
#2595 = FACE_OUTER_BOUND ( 'NONE', #17595, .T. ) ;
#2596 = B_SPLINE_CURVE_WITH_KNOTS ( 'NONE', 3,
 ( #3576, #12711, #1389, #22320, #1231, #774, #29549, #7983, #13021, #17583, #927, #5630, #1074, #15230, #25303, #8290, #17885, #3267, #12874, #10518, #20418, #29705, #8133, #17730, #27489, #15536 ),
 .UNSPECIFIED., .F., .F.,
 ( 4, 2, 2, 2, 2, 2, 2, 2, 2, 2, 2, 2, 4 ),
 ( 0.000000000000000000, 0.001576840078853157653, 0.002365260118279736805, 0.003153680157706315306, 0.004730520236559471008, 0.005518940275986051677, 0.006307360315412630612, 0.007884200394265785880, 0.008672620433692339662, 0.009461040473118895178, 0.01024946051254545069, 0.01103788055197200621, 0.01261472063082510163 ),
 .UNSPECIFIED. ) ;
#2597 = CARTESIAN_POINT ( 'NONE',  ( -5.434147616959247529, -3.211087428728324866, -68.80382590962500444 ) ) ;
#2598 = ORIENTED_EDGE ( 'NONE', *, *, #20579, .F. ) ;
#2599 = CARTESIAN_POINT ( 'NONE',  ( -0.4514894588696835021, 4.335480228600247621, -26.38903409329999761 ) ) ;
#2600 = CARTESIAN_POINT ( 'NONE',  ( -1.992768273746703400, -0.6766242680978976631, 226.6412452697800006 ) ) ;
#2601 = CARTESIAN_POINT ( 'NONE',  ( -4.568101251964836074, -0.2431723019727868862, -65.56421022022500722 ) ) ;
#2602 = DIRECTION ( 'NONE',  ( -4.428977494234582379E-12, -0.8987940462991651502, 0.4383711467890810676 ) ) ;
#2603 = CARTESIAN_POINT ( 'NONE',  ( 17.18658402241074867, -10.09981795543446736, -0.6999999999999784173 ) ) ;
#2604 = CARTESIAN_POINT ( 'NONE',  ( -4.858207114627580481, -18.06692763756964482, -28.66733978701845231 ) ) ;
#2605 = CARTESIAN_POINT ( 'NONE',  ( -7.999999999682589014, -15.17486759261230311, -33.15315993661145910 ) ) ;
#2606 = CARTESIAN_POINT ( 'NONE',  ( -17.33922399256787727, -22.00031055996563012, -26.74546041328948576 ) ) ;
#2607 = ORIENTED_EDGE ( 'NONE', *, *, #7583, .T. ) ;
#2608 = DIRECTION ( 'NONE',  ( -0.4911057670060950398, 1.966019939440381643E-12, 0.8710999515631688839 ) ) ;
#2609 = CARTESIAN_POINT ( 'NONE',  ( 8.700000000287717583, -16.96959321760160222, -37.81493174583334849 ) ) ;
#2610 = CARTESIAN_POINT ( 'NONE',  ( -10.90668548210000210, -5.673847184790000497, 232.6627643349999914 ) ) ;
#2611 = CARTESIAN_POINT ( 'NONE',  ( -22.83911268609999823, 16.42879705509999866, 229.0000000000000000 ) ) ;
#2612 = CIRCLE ( 'NONE', #19689, 28.50000000000000000 ) ;
#2613 = CARTESIAN_POINT ( 'NONE',  ( -10.69999999989999928, -45.00000000000000000, -7.274962170800002070 ) ) ;
#2614 = B_SPLINE_CURVE_WITH_KNOTS ( 'NONE', 3,
 ( #13940, #27944, #7010, #20873 ),
 .UNSPECIFIED., .F., .F.,
 ( 4, 4 ),
 ( 0.000000000000000000, 1.000000000000000000 ),
 .UNSPECIFIED. ) ;
#2615 = CARTESIAN_POINT ( 'NONE',  ( -8.699999999718343702, -24.19750589173278499, -27.32947359979484858 ) ) ;
#2616 = CARTESIAN_POINT ( 'NONE',  ( 1.243449787579999883E-14, -31.15538618883996946, -82.34631830372681804 ) ) ;
#2617 = CARTESIAN_POINT ( 'NONE',  ( 24.06826093652101051, -20.50742065841456707, 0.7595836940000044724 ) ) ;
#2619 = EDGE_CURVE ( 'NONE', #16921, #22622, #17600, .T. ) ;
#2618 = CARTESIAN_POINT ( 'NONE',  ( -0.4946807615411580872, -26.79522487540722153, 225.9931951744256367 ) ) ;
#2620 = LINE ( 'NONE', #12064, #6727 ) ;
#2621 = CARTESIAN_POINT ( 'NONE',  ( 1.747572776708514519, -1.007237960741800720, 227.6412452702466283 ) ) ;
#2622 = CARTESIAN_POINT ( 'NONE',  ( 12.55799324160000019, 20.99999999999999645, -55.95247857500000066 ) ) ;
#2623 = CARTESIAN_POINT ( 'NONE',  ( -16.37013654256265482, -7.994344025985067326, 0.000000000000000000 ) ) ;
#2624 = DIRECTION ( 'NONE',  ( 1.000000000000000000, 0.000000000000000000, 0.000000000000000000 ) ) ;
#2625 = EDGE_LOOP ( 'NONE', ( #31017, #27334, #3846, #5304 ) ) ;
#2626 = CARTESIAN_POINT ( 'NONE',  ( -16.83342759579999637, 11.00000000000000355, -0.8000000000000020428 ) ) ;
#2627 = CARTESIAN_POINT ( 'NONE',  ( 0.000000000000000000, 0.000000000000000000, 0.000000000000000000 ) ) ;
#2628 = ORIENTED_EDGE ( 'NONE', *, *, #23222, .F. ) ;
#2629 = B_SPLINE_CURVE_WITH_KNOTS ( 'NONE', 3,
 ( #24631, #876, #26678, #12663, #22270, #5582 ),
 .UNSPECIFIED., .F., .F.,
 ( 4, 2, 4 ),
 ( 0.4735259726301723759, 0.7367629863150860769, 1.000000000000000000 ),
 .UNSPECIFIED. ) ;
#2630 = CARTESIAN_POINT ( 'NONE',  ( 25.22625794089999829, -13.26224522399999906, 225.1041818340000020 ) ) ;
#2631 = AXIS2_PLACEMENT_3D ( 'NONE', #7709, #14813, #14506 ) ;
#2632 = CARTESIAN_POINT ( 'NONE',  ( -4.907595108193963718, 2.436408417516491287, -57.59877225282500746 ) ) ;
#2633 = ORIENTED_EDGE ( 'NONE', *, *, #7472, .F. ) ;
#2634 = CONTEXT_DEPENDENT_SHAPE_REPRESENTATION ( #19634, #2185 ) ;
#2635 = ORIENTED_EDGE ( 'NONE', *, *, #30861, .T. ) ;
#2636 = LINE ( 'NONE', #19783, #15101 ) ;
#2637 = ORIENTED_EDGE ( 'NONE', *, *, #5282, .T. ) ;
#2638 =( NAMED_UNIT ( * ) SI_UNIT ( $, .STERADIAN. ) SOLID_ANGLE_UNIT ( ) );
#2639 = EDGE_CURVE ( 'NONE', #17407, #15025, #4686, .T. ) ;
#2640 = CARTESIAN_POINT ( 'NONE',  ( -24.37821945910799926, 14.76389285725497125, 4.791564337000009388 ) ) ;
#2641 = DIRECTION ( 'NONE',  ( -1.000000000000000000, 5.687698019341907056E-16, -6.771501495046482653E-12 ) ) ;
#2642 = CARTESIAN_POINT ( 'NONE',  ( 3.901012673769999939, 11.36127833220000127, 231.9999991140000191 ) ) ;
#2643 = CARTESIAN_POINT ( 'NONE',  ( -5.082228009654736312, -3.365126390422853220, -6.889929326000007848 ) ) ;
#2644 = CARTESIAN_POINT ( 'NONE',  ( 3.389121577140000063, 11.55088360979999962, 230.6412452697800006 ) ) ;
#2645 = ORIENTED_EDGE ( 'NONE', *, *, #879, .T. ) ;
#2646 = DIRECTION ( 'NONE',  ( 1.000000000000000000, 0.000000000000000000, 0.000000000000000000 ) ) ;
#2647 = CARTESIAN_POINT ( 'NONE',  ( -2.595987296770100095, -18.41037502479620969, -108.0771722350183381 ) ) ;
#2648 = CARTESIAN_POINT ( 'NONE',  ( -3.331422745097509797, -2.438398348906448021, -19.37254627010001329 ) ) ;
#2649 = FACE_OUTER_BOUND ( 'NONE', #5464, .T. ) ;
#2650 = CARTESIAN_POINT ( 'NONE',  ( 14.39562240800000126, -9.581487064249998298, 225.0000000000000000 ) ) ;
#2651 = VECTOR ( 'NONE', #7343, 1000.000000000000114 ) ;
#2652 = CARTESIAN_POINT ( 'NONE',  ( -0.1113126274910280905, 46.88748299613427406, -63.68552844559068404 ) ) ;
#2653 = CARTESIAN_POINT ( 'NONE',  ( 17.16657240490000191, -8.999999999699998199, -1.399999999999998579 ) ) ;
#2654 = CARTESIAN_POINT ( 'NONE',  ( 4.248246898893026646, -2.821772188863608921, -43.35875473022499449 ) ) ;
#2655 = B_SPLINE_SURFACE_WITH_KNOTS ( 'NONE', 5, 1, ( 
 ( #19492, #26719 ),
 ( #30830, #18866 ),
 ( #28463, #26112 ),
 ( #6899, #16501 ),
 ( #4550, #14152 ),
 ( #30984, #3107 ),
 ( #17272, #7826 ),
 ( #24367, #29849 ),
 ( #29699, #17878 ) ),
 .UNSPECIFIED., .F., .F., .F.,
 ( 6, 3, 6 ),
 ( 2, 2 ),
 ( 72.29952875009999502, 84.34563975540000058, 88.66903727190000950 ),
 ( -3.307798128770000356E-15, 0.7016521142910000508 ),
 .UNSPECIFIED. ) ;
#2656 = CARTESIAN_POINT ( 'NONE',  ( 18.95046173579999760, -18.95046173579999760, 115.0000000000000000 ) ) ;
#2657 = CARTESIAN_POINT ( 'NONE',  ( -15.88249986683283232, 11.57137507597117754, -4.336808689942017243E-16 ) ) ;
#2658 = CARTESIAN_POINT ( 'NONE',  ( -4.861312627818040966, -19.47514616053552317, -31.31831154297147535 ) ) ;
#2659 = CARTESIAN_POINT ( 'NONE',  ( -24.49145440957854802, 14.57548795260905550, 5.680829343999993952 ) ) ;
#2660 = EDGE_CURVE ( 'NONE', #24695, #14421, #12575, .T. ) ;
#2661 = B_SPLINE_CURVE_WITH_KNOTS ( 'NONE', 3,
 ( #25590, #4025, #20545, #29978, #4340, #23395, #13622, #13459, #18173, #27774 ),
 .UNSPECIFIED., .F., .F.,
 ( 4, 2, 2, 2, 4 ),
 ( 0.000000000000000000, 0.2500000000000000000, 0.5000000000000000000, 0.7500000000000000000, 1.000000000000000000 ),
 .UNSPECIFIED. ) ;
#2662 = DIRECTION ( 'NONE',  ( 0.2815395311429191860, 0.9595496299847263710, 0.000000000000000000 ) ) ;
#2663 = ORIENTED_EDGE ( 'NONE', *, *, #7083, .F. ) ;
#2664 = CARTESIAN_POINT ( 'NONE',  ( 4.420334067734101424, -4.199682076162645217, -30.65126389020000985 ) ) ;
#2665 = CARTESIAN_POINT ( 'NONE',  ( 9.999999999970647480, -121.7869891337928010, -31.32664466927749558 ) ) ;
#2666 = ORIENTED_EDGE ( 'NONE', *, *, #22345, .T. ) ;
#2667 = CARTESIAN_POINT ( 'NONE',  ( -10.00000000001340617, -31.36353147789393958, -21.95991608827594987 ) ) ;
#2668 = CARTESIAN_POINT ( 'NONE',  ( 1.634888019277636051, 4.633891277622259608, -45.49079303332499791 ) ) ;
#2669 = ORIENTED_EDGE ( 'NONE', *, *, #30970, .T. ) ;
#2670 = ORIENTED_EDGE ( 'NONE', *, *, #30110, .T. ) ;
#2671 = DIRECTION ( 'NONE',  ( 1.000000000000000000, 0.000000000000000000, 0.000000000000000000 ) ) ;
#2672 = VERTEX_POINT ( 'NONE', #14752 ) ;
#2673 = CARTESIAN_POINT ( 'NONE',  ( -7.999999999729513256, -26.54727805893419657, -25.41789611383235226 ) ) ;
#2674 = ORIENTED_EDGE ( 'NONE', *, *, #14214, .T. ) ;
#2675 = AXIS2_PLACEMENT_3D ( 'NONE', #9937, #3151, #14511 ) ;
#2676 = DIRECTION ( 'NONE',  ( 0.000000000000000000, 0.000000000000000000, -1.000000000000000000 ) ) ;
#2677 = DIRECTION ( 'NONE',  ( 1.000000000000000000, 0.000000000000000000, 0.000000000000000000 ) ) ;
#2678 = EDGE_CURVE ( 'NONE', #6922, #23430, #23727, .T. ) ;
#2679 = CARTESIAN_POINT ( 'NONE',  ( -2.020725942109999895, 3.500000000090000007, 227.9588918784999976 ) ) ;
#2680 = CARTESIAN_POINT ( 'NONE',  ( 0.7542811793706193368, 4.720842771144411643, -35.70000000000000284 ) ) ;
#2681 = CARTESIAN_POINT ( 'NONE',  ( 18.79419193508953967, 19.99998513589524407, -0.5771770174943486875 ) ) ;
#2682 = CARTESIAN_POINT ( 'NONE',  ( -24.92013865347427171, 13.82966157970119525, 6.099998581000020792 ) ) ;
#2683 = CARTESIAN_POINT ( 'NONE',  ( -22.86188831003414634, -13.98516151716066069, 5.876648809228268711 ) ) ;
#2684 = CARTESIAN_POINT ( 'NONE',  ( -0.1113126277255015173, -0.6952657331094624915, -40.47787123679744070 ) ) ;
#2685 = CARTESIAN_POINT ( 'NONE',  ( -3.099128499470596321, -3.102542665468454253, -9.813991631000003935 ) ) ;
#2686 = CARTESIAN_POINT ( 'NONE',  ( 4.634019325638258024, 0.4639887426745141208, -29.13116556700001070 ) ) ;
#2687 = CARTESIAN_POINT ( 'NONE',  ( 3.350725639037565706, -1.107490566386527986, 0.000000000000000000 ) ) ;
#2688 = FACE_OUTER_BOUND ( 'NONE', #11071, .T. ) ;
#2689 = EDGE_CURVE ( 'NONE', #18386, #18002, #22877, .T. ) ;
#2690 = CARTESIAN_POINT ( 'NONE',  ( 24.75645985066559263, 14.12045945726143970, 5.901294549000013490 ) ) ;
#2691 = CARTESIAN_POINT ( 'NONE',  ( 12.74757277707238856, 25.48862485010116075, -59.60122879113606587 ) ) ;
#2692 = CARTESIAN_POINT ( 'NONE',  ( 11.20000000009999930, -21.99999999940999729, -31.28675134550999815 ) ) ;
#2693 = CARTESIAN_POINT ( 'NONE',  ( 4.354753084053725409, 0.1085053810021691101, -20.67661200060000226 ) ) ;
#2694 = AXIS2_PLACEMENT_3D ( 'NONE', #3038, #4942, #9822 ) ;
#2695 = EDGE_CURVE ( 'NONE', #22118, #18765, #4850, .T. ) ;
#2696 = TOROIDAL_SURFACE ( 'NONE', #29324, 3.176829268290000563, 0.2500000000000000000 ) ;
#2697 = CYLINDRICAL_SURFACE ( 'NONE', #5182, 2.100000000000000977 ) ;
#2698 = CARTESIAN_POINT ( 'NONE',  ( -2.744116393020877620, -4.299119443564640264, -68.10000000002500542 ) ) ;
#2699 = DIRECTION ( 'NONE',  ( 0.000000000000000000, 0.9624904629342537765, -0.2713155151490711514 ) ) ;
#2700 = ORIENTED_EDGE ( 'NONE', *, *, #8988, .T. ) ;
#2701 = EDGE_CURVE ( 'NONE', #29716, #25525, #15718, .T. ) ;
#2702 = CARTESIAN_POINT ( 'NONE',  ( 1.607747500013188446, -28.45491842328731025, 4.689797669000017599 ) ) ;
#2703 = CARTESIAN_POINT ( 'NONE',  ( 16.85920661257417663, 12.06595463936088208, -4.336808689942018722E-16 ) ) ;
#2704 = VERTEX_POINT ( 'NONE', #2337 ) ;
#2705 = CARTESIAN_POINT ( 'NONE',  ( -10.69999999930000101, -120.5233595624000174, -31.26042064949999855 ) ) ;
#2706 = CARTESIAN_POINT ( 'NONE',  ( -16.14314806408744118, 10.13116291470765162, -0.6999999999999784173 ) ) ;
#2707 = VERTEX_POINT ( 'NONE', #11920 ) ;
#2708 = CARTESIAN_POINT ( 'NONE',  ( 9.747572776401462136, -14.93176076027399901, -74.31304601088737627 ) ) ;
#2709 = VERTEX_POINT ( 'NONE', #21528 ) ;
#2710 = EDGE_LOOP ( 'NONE', ( #24883, #16294, #14538, #25977, #13641, #20747 ) ) ;
#2711 = FILL_AREA_STYLE ('',( #5071 ) ) ;
#2712 = SHAPE_REPRESENTATION ( 'MAS-156', ( #7812, #27407, #22391, #26409, #28916, #15350, #30929, #29902, #19876, #1798, #19377, #11830, #13322, #9829, #21378, #25403, #13850, #17848, #21901, #8296, #25919, #2780, #12343, #25903, #20357, #24385, #10815 ), #2796 ) ;
#2713 = VERTEX_POINT ( 'NONE', #29065 ) ;
#2714 = CARTESIAN_POINT ( 'NONE',  ( -4.861312627696710464, 6.462009008221268225, -40.63090155203819620 ) ) ;
#2715 = EDGE_CURVE ( 'NONE', #14751, #4997, #24380, .T. ) ;
#2717 = CARTESIAN_POINT ( 'NONE',  ( -7.999999999683915952, -16.84112630284391443, -33.19732204833458411 ) ) ;
#2716 = VECTOR ( 'NONE', #7230, 1000.000000000000000 ) ;
#2718 = VECTOR ( 'NONE', #4910, 1000.000000000000000 ) ;
#2719 = ORIENTED_EDGE ( 'NONE', *, *, #9384, .T. ) ;
#2720 = DIRECTION ( 'NONE',  ( 0.2815395311429191860, 0.9595496299847262600, 0.000000000000000000 ) ) ;
#2721 = VECTOR ( 'NONE', #18193, 1000.000000000000000 ) ;
#2722 = AXIS2_PLACEMENT_3D ( 'NONE', #8150, #17745, #22341 ) ;
#2723 = CARTESIAN_POINT ( 'NONE',  ( 24.34567703855588761, -13.42188430278006273, 225.9642891784011454 ) ) ;
#2724 = CARTESIAN_POINT ( 'NONE',  ( -17.04621913067799710, -32.00000000000000000, -31.28675134614999820 ) ) ;
#2725 = CARTESIAN_POINT ( 'NONE',  ( 8.999999999770000869, 20.99999999999999645, -53.60000000000000142 ) ) ;
#2726 = ORIENTED_EDGE ( 'NONE', *, *, #8710, .F. ) ;
#2727 = EDGE_CURVE ( 'NONE', #11580, #4569, #17252, .T. ) ;
#2728 = B_SPLINE_CURVE_WITH_KNOTS ( 'NONE', 3,
 ( #25200, #13227, #3804, #21110, #30554, #3957, #1914, #13555, #8983, #23163, #30706, #22844, #1292, #1603, #11193, #20792, #8823, #18426 ),
 .UNSPECIFIED., .F., .F.,
 ( 4, 2, 2, 2, 2, 2, 2, 2, 4 ),
 ( 0.000000000000000000, 0.1250000000000000278, 0.2500000000000000000, 0.3749999999999999445, 0.4999999999999999445, 0.6249999999999998890, 0.7499999999999998890, 0.8750000000000000000, 1.000000000000000000 ),
 .UNSPECIFIED. ) ;
#2729 = CARTESIAN_POINT ( 'NONE',  ( 2.326244606069572285, 3.379075471592549729, -16.71259163650000090 ) ) ;
#2730 = CARTESIAN_POINT ( 'NONE',  ( 18.13627780309760595, -9.538245302789915669, -0.6999999999999785283 ) ) ;
#2731 = FACE_OUTER_BOUND ( 'NONE', #20312, .T. ) ;
#2732 = COLOUR_RGB ( '', 0.09019608, 0.27058824, 0.51372549) ;
#2733 = CARTESIAN_POINT ( 'NONE',  ( -12.32161713220326327, -29.02784567618598999, -33.00245466908037884 ) ) ;
#2734 = CARTESIAN_POINT ( 'NONE',  ( 17.83928249680000278, 19.99999999999999645, -1.399999999299995856 ) ) ;
#2735 = CARTESIAN_POINT ( 'NONE',  ( -24.32472894358752313, 13.45989150749028873, 3.899998581000013509 ) ) ;
#2736 = CARTESIAN_POINT ( 'NONE',  ( -10.69999999999999929, -24.87867968679999819, -26.27867968680000033 ) ) ;
#2737 = CARTESIAN_POINT ( 'NONE',  ( -10.69999999999999929, -26.32120392050000035, -31.35200361700000471 ) ) ;
#2738 = EDGE_CURVE ( 'NONE', #19721, #12957, #16948, .T. ) ;
#2739 = CARTESIAN_POINT ( 'NONE',  ( 18.03440925470000167, 20.21871195210000138, 229.9751246720000211 ) ) ;
#2740 = CARTESIAN_POINT ( 'NONE',  ( -13.33996868140000025, 12.49968273260000018, 230.6999999999999886 ) ) ;
#2741 = ORIENTED_EDGE ( 'NONE', *, *, #981, .F. ) ;
#2742 = CARTESIAN_POINT ( 'NONE',  ( 3.599561039394925999, 4.779710538172339263, -54.14619010302499191 ) ) ;
#2743 = CARTESIAN_POINT ( 'NONE',  ( -12.60598845461798767, -26.55662275894602331, -22.88248127776499885 ) ) ;
#2744 = VECTOR ( 'NONE', #2556, 1000.000000000000000 ) ;
#2745 = VECTOR ( 'NONE', #24286, 1000.000000000000000 ) ;
#2746 = CARTESIAN_POINT ( 'NONE',  ( -27.17362711782706342, 4.180443856937215763, 0.02487529600000981667 ) ) ;
#2747 = CARTESIAN_POINT ( 'NONE',  ( -7.246551124551907641, 5.407433690575946805, -40.11655080252537431 ) ) ;
#2748 = EDGE_LOOP ( 'NONE', ( #26366, #21675, #28485, #19199, #18414 ) ) ;
#2749 = DIRECTION ( 'NONE',  ( 0.000000000000000000, 0.000000000000000000, -1.000000000000000000 ) ) ;
#2750 = SHAPE_REPRESENTATION_RELATIONSHIP ( 'NONE' , 'NONE' ,  #3523, #18548 ) ;
#2751 = VERTEX_POINT ( 'NONE', #10184 ) ;
#2752 = CARTESIAN_POINT ( 'NONE',  ( 3.790136060690228792, 1.782282071276910962, -38.34844621930091790 ) ) ;
#2753 = EDGE_CURVE ( 'NONE', #15244, #5752, #12004, .T. ) ;
#2754 =( GEOMETRIC_REPRESENTATION_CONTEXT ( 3 ) GLOBAL_UNCERTAINTY_ASSIGNED_CONTEXT ( ( #28883 ) ) GLOBAL_UNIT_ASSIGNED_CONTEXT ( ( #14838, #10569, #19707 ) ) REPRESENTATION_CONTEXT ( 'NONE', 'WORKASPACE' ) );
#2755 = CARTESIAN_POINT ( 'NONE',  ( -5.606848515966891711, 1.848691355091094835, -68.74019511502498858 ) ) ;
#2756 = VERTEX_POINT ( 'NONE', #10496 ) ;
#2757 = CARTESIAN_POINT ( 'NONE',  ( 0.09521150875769815447, -4.665041947735804939, -24.91888333260000721 ) ) ;
#2758 = FACE_OUTER_BOUND ( 'NONE', #6176, .T. ) ;
#2759 = ADVANCED_FACE ( 'NONE', ( #1053 ), #7242, .T. ) ;
#2760 = B_SPLINE_SURFACE_WITH_KNOTS ( 'NONE', 5, 1, ( 
 ( #19820, #9748 ),
 ( #19355, #16830 ),
 ( #14939, #5028 ),
 ( #11955, #24539 ),
 ( #7684, #29403 ),
 ( #28946, #21564 ),
 ( #10217, #17441 ),
 ( #13, #22031 ),
 ( #19661, #7542 ),
 ( #29245, #26735 ),
 ( #326, #16984 ),
 ( #17133, #9907 ),
 ( #9596, #2978 ),
 ( #2520, #7838 ),
 ( #4877, #19195 ) ),
 .UNSPECIFIED., .F., .F., .F.,
 ( 6, 3, 3, 3, 6 ),
 ( 2, 2 ),
 ( 0.000000000000000000, 0.5239049114710000454, 1.047809822950000136, 1.571714734409999981, 1.746349704900000077 ),
 ( -0.7000000000009999335, 2.557517314480000010E-06 ),
 .UNSPECIFIED. ) ;
#2761 = CARTESIAN_POINT ( 'NONE',  ( 3.357378826396556271, -2.722208303779470651, -55.40923804942499942 ) ) ;
#2762 = CARTESIAN_POINT ( 'NONE',  ( -11.00000000000000000, 25.22617105830878614, -61.82510970417090590 ) ) ;
#2763 = AXIS2_PLACEMENT_3D ( 'NONE', #1076, #19810, #3115 ) ;
#2764 = CARTESIAN_POINT ( 'NONE',  ( -15.73738422052369046, 11.17152825612159717, -1.400000000000001910 ) ) ;
#2765 = UNCERTAINTY_MEASURE_WITH_UNIT (LENGTH_MEASURE( 1.000000000000000082E-05 ), #7690, 'distance_accuracy_value', 'NONE');
#2766 = CARTESIAN_POINT ( 'NONE',  ( 17.18658402241074867, -10.09981795543446736, -1.000005633855494125E-09 ) ) ;
#2767 = CARTESIAN_POINT ( 'NONE',  ( -26.80000000000000071, -7.283063041539999493E-14, 230.0000000000000000 ) ) ;
#2768 = ORIENTED_EDGE ( 'NONE', *, *, #18659, .T. ) ;
#2769 = CARTESIAN_POINT ( 'NONE',  ( -12.30000000044999986, -30.20000000000000284, -28.40000000001083791 ) ) ;
#2770 = CYLINDRICAL_SURFACE ( 'NONE', #28345, 3.000000000000002220 ) ;
#2771 = CARTESIAN_POINT ( 'NONE',  ( -7.384740713219999364, -9.544372888970000801, 231.9999989789999972 ) ) ;
#2772 = CARTESIAN_POINT ( 'NONE',  ( -0.6731456008920000400, -3.434453875705480108, -72.25672407562892374 ) ) ;
#2773 = CARTESIAN_POINT ( 'NONE',  ( -24.36725163763869162, -13.38201776504303986, 4.999998581000003384 ) ) ;
#2774 = AXIS2_PLACEMENT_3D ( 'NONE', #27249, #27402, #20472 ) ;
#2775 = CARTESIAN_POINT ( 'NONE',  ( -11.69999999989999928, -24.11120071670000087, -0.6999999999999992895 ) ) ;
#2776 = CARTESIAN_POINT ( 'NONE',  ( -17.15915740090245123, -7.941754552259828515, 0.000000000000000000 ) ) ;
#2777 = CARTESIAN_POINT ( 'NONE',  ( -28.31737690039761901, -7.971550764210702411, 0.5017677510000262409 ) ) ;
#2778 = DIRECTION ( 'NONE',  ( -0.8660254037843289066, -0.5000000000001899592, 0.000000000000000000 ) ) ;
#2779 = CIRCLE ( 'NONE', #9807, 4.000000004070001225 ) ;
#2780 = AXIS2_PLACEMENT_3D ( 'NONE', #27205, #29564, #20129 ) ;
#2781 = CARTESIAN_POINT ( 'NONE',  ( -24.95427444319612675, 13.76797446832583560, 3.899998581000013509 ) ) ;
#2782 = CARTESIAN_POINT ( 'NONE',  ( 6.304462385800995605, 10.33059233208346406, 232.0000002394077114 ) ) ;
#2783 = FACE_OUTER_BOUND ( 'NONE', #321, .T. ) ;
#2784 = DIRECTION ( 'NONE',  ( 0.000000000000000000, 0.000000000000000000, -1.000000000000000000 ) ) ;
#2785 = VERTEX_POINT ( 'NONE', #21181 ) ;
#2786 = CARTESIAN_POINT ( 'NONE',  ( 27.69999999930000101, -3.392159599989999961E-15, 190.0000000000000000 ) ) ;
#2787 = CARTESIAN_POINT ( 'NONE',  ( 24.09856112909268688, -15.21545593799569751, 224.8524796740992144 ) ) ;
#2788 = EDGE_CURVE ( 'NONE', #16560, #17135, #2973, .T. ) ;
#2789 = CARTESIAN_POINT ( 'NONE',  ( -3.174852331340443534, -3.764700477890503549, -59.92407541852500685 ) ) ;
#2790 = ORIENTED_EDGE ( 'NONE', *, *, #7528, .F. ) ;
#2791 = ORIENTED_EDGE ( 'NONE', *, *, #5209, .F. ) ;
#2792 = EDGE_CURVE ( 'NONE', #6070, #11998, #10113, .T. ) ;
#2793 = CARTESIAN_POINT ( 'NONE',  ( -17.19683899163034724, -26.54814041842956840, -22.88737855935614007 ) ) ;
#2794 = EDGE_CURVE ( 'NONE', #5941, #1473, #21370, .T. ) ;
#2795 = ORIENTED_EDGE ( 'NONE', *, *, #598, .F. ) ;
#2796 =( GEOMETRIC_REPRESENTATION_CONTEXT ( 3 ) GLOBAL_UNCERTAINTY_ASSIGNED_CONTEXT ( ( #2765 ) ) GLOBAL_UNIT_ASSIGNED_CONTEXT ( ( #7690, #15398, #13034 ) ) REPRESENTATION_CONTEXT ( 'NONE', 'WORKASPACE' ) );
#2797 = FACE_OUTER_BOUND ( 'NONE', #26703, .T. ) ;
#2798 = DIRECTION ( 'NONE',  ( 0.000000000000000000, 0.000000000000000000, 1.000000000000000000 ) ) ;
#2799 = CARTESIAN_POINT ( 'NONE',  ( -2.449212707639999657E-16, 2.000000000000000000, 229.2412452703699728 ) ) ;
#2800 = LINE ( 'NONE', #26711, #25375 ) ;
#2801 = CARTESIAN_POINT ( 'NONE',  ( 8.700000000244115128, -26.99999999999395328, -28.39999999994493862 ) ) ;
#2802 = CARTESIAN_POINT ( 'NONE',  ( 4.294959833232216972, -2.194189917041240445, -10.97724735219999914 ) ) ;
#2803 = DIRECTION ( 'NONE',  ( 1.000000000000000000, 0.000000000000000000, 0.000000000000000000 ) ) ;
#2804 = EDGE_LOOP ( 'NONE', ( #26260, #13279, #6185, #18214 ) ) ;
#2805 = CARTESIAN_POINT ( 'NONE',  ( 2.868523387327241991, -3.581275371925169537, -44.10000000002499121 ) ) ;
#2806 = CARTESIAN_POINT ( 'NONE',  ( -24.41841039498785193, -14.69667350221323865, 3.899998581000013509 ) ) ;
#2807 = CARTESIAN_POINT ( 'NONE',  ( -3.117834729128555971, -4.866792379758847709, -19.30544088820000681 ) ) ;
#2808 = CARTESIAN_POINT ( 'NONE',  ( 17.95841148951064525, -9.763538383420391042, 0.000000000000000000 ) ) ;
#2809 = FACE_OUTER_BOUND ( 'NONE', #6045, .T. ) ;
#2810 = CARTESIAN_POINT ( 'NONE',  ( -11.93900533819999943, 2.124654348349999999, 230.6412452697800006 ) ) ;
#2811 = CARTESIAN_POINT ( 'NONE',  ( -16.01948174858000229, -8.256768211624056164, 0.000000000000000000 ) ) ;
#2812 = CARTESIAN_POINT ( 'NONE',  ( 1.970249664213433727, 5.584433078155761621, -44.69079303332500075 ) ) ;
#2813 = CYLINDRICAL_SURFACE ( 'NONE', #24284, 2.000000000000003553 ) ;
#2814 = LINE ( 'NONE', #22167, #18267 ) ;
#2815 = CARTESIAN_POINT ( 'NONE',  ( -4.861312627816293919, -19.12054368222343470, -31.49126272763050238 ) ) ;
#2816 = CARTESIAN_POINT ( 'NONE',  ( -24.59646680460000212, 13.64432696080000085, 229.7313261780000175 ) ) ;
#2817 = ADVANCED_FACE ( 'NONE', ( #24932 ), #22423, .F. ) ;
#2818 = FACE_OUTER_BOUND ( 'NONE', #1439, .T. ) ;
#2819 = EDGE_LOOP ( 'NONE', ( #21416, #11954, #26297, #20006 ) ) ;
#2820 = CARTESIAN_POINT ( 'NONE',  ( -6.085238278930475531, -0.01014600953121863602, -28.76856466009999735 ) ) ;
#2821 = ORIENTED_EDGE ( 'NONE', *, *, #9836, .F. ) ;
#2822 = CARTESIAN_POINT ( 'NONE',  ( 9.999999999970629716, -25.15635984103874279, -30.79900052789801990 ) ) ;
#2823 = CARTESIAN_POINT ( 'NONE',  ( 2.534862810676351330, -4.171999357468124003, -46.56669147672499065 ) ) ;
#2824 = VERTEX_POINT ( 'NONE', #570 ) ;
#2825 = ORIENTED_EDGE ( 'NONE', *, *, #24311, .F. ) ;
#2826 = SHAPE_DEFINITION_REPRESENTATION ( #18689, #19806 ) ;
#2827 = ORIENTED_EDGE ( 'NONE', *, *, #2972, .F. ) ;
#2828 = CARTESIAN_POINT ( 'NONE',  ( 20.05330963473244310, 19.99997410271232923, 229.7574610911009643 ) ) ;
#2829 = EDGE_LOOP ( 'NONE', ( #19362, #23310, #17776, #25400 ) ) ;
#2830 = CARTESIAN_POINT ( 'NONE',  ( -16.83342759582943060, -8.999999999996580513, -0.6999999999999784173 ) ) ;
#2831 = LINE ( 'NONE', #22041, #12259 ) ;
#2832 = CYLINDRICAL_SURFACE ( 'NONE', #24536, 26.80000000000002203 ) ;
#2833 = CARTESIAN_POINT ( 'NONE',  ( 0.3516186674615833230, 4.635787241539998327, -35.69999999999998863 ) ) ;
#2834 = CARTESIAN_POINT ( 'NONE',  ( -24.43008698341936835, 14.67811372381255630, 5.507121130000014020 ) ) ;
#2835 = FACE_OUTER_BOUND ( 'NONE', #10954, .T. ) ;
#2836 = CARTESIAN_POINT ( 'NONE',  ( -23.65375779729673056, -14.60692596462244985, 224.2670087215145998 ) ) ;
#2837 = CARTESIAN_POINT ( 'NONE',  ( 4.262818619062177738, -0.7545854518158033875, -9.271482634700010550 ) ) ;
#2838 = CARTESIAN_POINT ( 'NONE',  ( 1.723678405763061194, 4.474283509182772178, -25.15712237480000013 ) ) ;
#2839 = CARTESIAN_POINT ( 'NONE',  ( 0.2829221443748314302, -27.79908343203750576, 226.0728295493879614 ) ) ;
#2840 = B_SPLINE_CURVE_WITH_KNOTS ( 'NONE', 5,
 ( #7941, #733, #3225, #583, #12980, #12833 ),
 .UNSPECIFIED., .F., .F.,
 ( 6, 6 ),
 ( 0.000000000000000000, 2.319815200139999867 ),
 .UNSPECIFIED. ) ;
#2841 = B_SPLINE_CURVE_WITH_KNOTS ( 'NONE', 5,
 ( #7349, #4526, #4984, #24183, #9387, #2623, #18991, #12802, #28597, #26235, #282, #14283 ),
 .UNSPECIFIED., .F., .F.,
 ( 6, 3, 3, 6 ),
 ( 1.224410041430000096, 1.456395031030000009, 2.184590861730000277, 2.448622038789999955 ),
 .UNSPECIFIED. ) ;
#2842 = CARTESIAN_POINT ( 'NONE',  ( 24.37821946547973084, -14.76389286113969490, 5.208432824000020389 ) ) ;
#2843 = EDGE_CURVE ( 'NONE', #21789, #11577, #18355, .T. ) ;
#2844 = CARTESIAN_POINT ( 'NONE',  ( -20.22682926819999949, -26.99999999999973355, -28.39999999990017798 ) ) ;
#2845 = CARTESIAN_POINT ( 'NONE',  ( -23.34643930348659069, -14.53345043296637584, 225.6425104786826239 ) ) ;
#2846 = CARTESIAN_POINT ( 'NONE',  ( 18.95046173579999760, -18.95046173579999760, 36.78285841159999592 ) ) ;
#2847 = CARTESIAN_POINT ( 'NONE',  ( 3.082386449366550263, -3.056625787687238471, -15.06112212870000455 ) ) ;
#2848 = ADVANCED_FACE ( 'NONE', ( #20362 ), #16778, .F. ) ;
#2849 = B_SPLINE_SURFACE_WITH_KNOTS ( 'NONE', 5, 1, ( 
 ( #3454, #15271 ),
 ( #1424, #25339 ),
 ( #8481, #20767 ),
 ( #15567, #20296 ),
 ( #20452, #30049 ),
 ( #13056, #964 ) ),
 .UNSPECIFIED., .F., .F., .F.,
 ( 6, 6 ),
 ( 2, 2 ),
 ( 4.999999893120000038, 7.000000000120000010 ),
 ( -5.329070518200000398E-15, 0.7000000000219999130 ),
 .UNSPECIFIED. ) ;
#2850 = DIRECTION ( 'NONE',  ( 0.000000000000000000, 0.000000000000000000, 1.000000000000000000 ) ) ;
#2851 = CARTESIAN_POINT ( 'NONE',  ( -24.97472003774791816, -13.73006752753317450, 4.791638085000021974 ) ) ;
#2852 = LINE ( 'NONE', #24418, #13785 ) ;
#2853 = ORIENTED_EDGE ( 'NONE', *, *, #9275, .T. ) ;
#2854 = EDGE_CURVE ( 'NONE', #9948, #26056, #11611, .T. ) ;
#2855 = CARTESIAN_POINT ( 'NONE',  ( 8.699999999511655702, -24.19750589174882904, -27.32947359971288037 ) ) ;
#2856 = CARTESIAN_POINT ( 'NONE',  ( 10.69999999999658691, -24.37864083502648072, -26.88914305872019028 ) ) ;
#2857 = ORIENTED_EDGE ( 'NONE', *, *, #9107, .F. ) ;
#2858 = CARTESIAN_POINT ( 'NONE',  ( -10.14902473063359523, -26.01926976387844093, 142.0603150149999863 ) ) ;
#2859 = DIRECTION ( 'NONE',  ( 0.000000000000000000, 0.000000000000000000, -1.000000000000000000 ) ) ;
#2860 = VERTEX_POINT ( 'NONE', #10925 ) ;
#2861 = CARTESIAN_POINT ( 'NONE',  ( -4.797151926237309461, -1.386351552423990219, -44.10000000002498410 ) ) ;
#2862 = ORIENTED_EDGE ( 'NONE', *, *, #13335, .T. ) ;
#2863 = EDGE_LOOP ( 'NONE', ( #28361, #29445, #9175, #18503 ) ) ;
#2864 = ORIENTED_EDGE ( 'NONE', *, *, #11367, .T. ) ;
#2865 = LINE ( 'NONE', #9637, #8425 ) ;
#2866 = CARTESIAN_POINT ( 'NONE',  ( 8.700000000252410715, -24.26136093482726608, -29.62468611105379779 ) ) ;
#2867 = EDGE_CURVE ( 'NONE', #19078, #22879, #28065, .T. ) ;
#2868 = DIRECTION ( 'NONE',  ( -3.924189347185962345E-12, 0.4082287037029531107, 0.9128796883888953273 ) ) ;
#2869 = ORIENTED_EDGE ( 'NONE', *, *, #5232, .T. ) ;
#2870 = CARTESIAN_POINT ( 'NONE',  ( -25.25401215124432852, 13.21081861195569296, 5.901400367999992902 ) ) ;
#2871 = B_SPLINE_CURVE_WITH_KNOTS ( 'NONE', 3,
 ( #12471, #14543, #26490, #14388 ),
 .UNSPECIFIED., .F., .F.,
 ( 4, 4 ),
 ( 0.000000000000000000, 1.000000000000000000 ),
 .UNSPECIFIED. ) ;
#2872 = CARTESIAN_POINT ( 'NONE',  ( 28.49528339128749366, 0.5184828350247233653, 1.000000000000000888 ) ) ;
#2873 = CARTESIAN_POINT ( 'NONE',  ( -17.38654519918826935, -31.99979139472987200, -29.76988878280269901 ) ) ;
#2874 = CARTESIAN_POINT ( 'NONE',  ( 7.610733143571420278, -7.258930934320984463, -37.27655781773084698 ) ) ;
#2875 = ORIENTED_EDGE ( 'NONE', *, *, #24409, .T. ) ;
#2876 = VECTOR ( 'NONE', #20015, 1000.000000000000227 ) ;
#2877 = DIRECTION ( 'NONE',  ( -2.256480420250000087E-12, 0.000000000000000000, 1.000000000000000000 ) ) ;
#2878 = CARTESIAN_POINT ( 'NONE',  ( 0.7420639427752478978, -6.011517603930927045, -18.37054674910000429 ) ) ;
#2879 = LINE ( 'NONE', #28840, #12838 ) ;
#2880 = TOROIDAL_SURFACE ( 'NONE', #25505, 30.50000000000000000, 3.000000000000000000 ) ;
#2881 = CARTESIAN_POINT ( 'NONE',  ( -10.69999999989999928, -25.00000000000000000, -7.274962171499997687 ) ) ;
#2882 = CARTESIAN_POINT ( 'NONE',  ( -12.39067510638770209, -28.44925785771653182, -33.33672124906113510 ) ) ;
#2883 = CARTESIAN_POINT ( 'NONE',  ( 27.79999999470000205, -2.355808389319999976E-11, 222.0000000000000000 ) ) ;
#2884 = DIRECTION ( 'NONE',  ( -0.000000000000000000, 1.000000000000000000, -2.257145581549999994E-12 ) ) ;
#2885 = CARTESIAN_POINT ( 'NONE',  ( -16.83342759575507586, 10.99999999997565503, -0.6999999999999784173 ) ) ;
#2886 = CARTESIAN_POINT ( 'NONE',  ( -10.35000000039999968, -43.95328087560000085, -27.24755286599999948 ) ) ;
#2887 = CARTESIAN_POINT ( 'NONE',  ( 21.97405983070000346, 17.61876539540000053, 229.2930768050000268 ) ) ;
#2888 = CARTESIAN_POINT ( 'NONE',  ( -11.49999999969999998, -27.00000000000000000, -28.40000000000541647 ) ) ;
#2889 = ORIENTED_EDGE ( 'NONE', *, *, #6189, .F. ) ;
#2890 = CARTESIAN_POINT ( 'NONE',  ( 2.752605500610148859, 3.655072764496607007, -54.62619010302499589 ) ) ;
#2891 = LINE ( 'NONE', #17205, #10294 ) ;
#2892 = EDGE_CURVE ( 'NONE', #29947, #18419, #1860, .T. ) ;
#2893 = AXIS2_PLACEMENT_3D ( 'NONE', #22500, #9248, #18857 ) ;
#2894 = CARTESIAN_POINT ( 'NONE',  ( -22.04938731152978448, 17.55153357857029306, 0.7069229489999884208 ) ) ;
#2895 = CARTESIAN_POINT ( 'NONE',  ( -4.533384324195958825, 1.003679825387874924, -68.10000000002499121 ) ) ;
#2896 = ORIENTED_EDGE ( 'NONE', *, *, #3349, .F. ) ;
#2897 = CARTESIAN_POINT ( 'NONE',  ( 0.3673706385115332318, 2.353674647662223673, -95.59336531685248417 ) ) ;
#2898 = B_SPLINE_CURVE_WITH_KNOTS ( 'NONE', 3,
 ( #659, #19850, #5055, #14818, #10399, #194 ),
 .UNSPECIFIED., .F., .F.,
 ( 4, 2, 4 ),
 ( 0.000000000000000000, 0.5000000000000000000, 1.000000000000000000 ),
 .UNSPECIFIED. ) ;
#2899 = AXIS2_PLACEMENT_3D ( 'NONE', #14131, #18842, #4682 ) ;
#2900 = ORIENTED_EDGE ( 'NONE', *, *, #23789, .F. ) ;
#2901 = DIRECTION ( 'NONE',  ( 1.000000000000000000, 0.000000000000000000, 0.000000000000000000 ) ) ;
#2902 = CARTESIAN_POINT ( 'NONE',  ( -10.00000000021857183, -125.3357287863419458, -32.69504109500191902 ) ) ;
#2903 = EDGE_CURVE ( 'NONE', #27611, #12887, #8583, .T. ) ;
#2904 = ORIENTED_EDGE ( 'NONE', *, *, #10367, .T. ) ;
#2905 = CARTESIAN_POINT ( 'NONE',  ( 5.536217179945332134, 2.001767383715431503, -27.51249766020000465 ) ) ;
#2906 = DIRECTION ( 'NONE',  ( 0.000000000000000000, -0.7071067811870488384, -0.7071067811860461960 ) ) ;
#2907 = EDGE_CURVE ( 'NONE', #24188, #1593, #3843, .T. ) ;
#2908 = EDGE_CURVE ( 'NONE', #13888, #17663, #7099, .T. ) ;
#2909 = CARTESIAN_POINT ( 'NONE',  ( 1.634888019277636051, 4.633891277622259608, -45.49079303332499791 ) ) ;
#2910 = DIRECTION ( 'NONE',  ( -5.962915006522622422E-16, -0.4383711467890810676, -0.8987940462991651502 ) ) ;
#2911 = FACE_OUTER_BOUND ( 'NONE', #4815, .T. ) ;
#2912 = AXIS2_PLACEMENT_3D ( 'NONE', #8307, #25003, #27364 ) ;
#2913 = EDGE_CURVE ( 'NONE', #23040, #9577, #12648, .T. ) ;
#2914 = CARTESIAN_POINT ( 'NONE',  ( -7.999999999668208517, -9.149979920084513552, -35.02638174925785819 ) ) ;
#2915 = FACE_OUTER_BOUND ( 'NONE', #29872, .T. ) ;
#2916 = ORIENTED_EDGE ( 'NONE', *, *, #2351, .T. ) ;
#2917 = CARTESIAN_POINT ( 'NONE',  ( -11.50000000000000000, 22.40709319595134730, -62.85117013414870257 ) ) ;
#2918 = CARTESIAN_POINT ( 'NONE',  ( -1.836086644060000106, -11.92016782080000148, 231.9999989789999972 ) ) ;
#2919 = AXIS2_PLACEMENT_3D ( 'NONE', #27908, #26020, #23666 ) ;
#2920 = DIRECTION ( 'NONE',  ( 1.000000000000000000, -0.000000000000000000, 0.000000000000000000 ) ) ;
#2921 = DIRECTION ( 'NONE',  ( 0.000000000000000000, 0.000000000000000000, -1.000000000000000000 ) ) ;
#2922 = CARTESIAN_POINT ( 'NONE',  ( -3.664716979113584738, -26.54951320538905435, 209.8067551132096469 ) ) ;
#2923 = CARTESIAN_POINT ( 'NONE',  ( 3.056196190786856448, -2.814750735090191025, -0.6999999999999992895 ) ) ;
#2925 = EDGE_CURVE ( 'NONE', #17588, #2487, #13103, .T. ) ;
#2924 = AXIS2_PLACEMENT_3D ( 'NONE', #17301, #337, #492 ) ;
#2926 = CARTESIAN_POINT ( 'NONE',  ( -24.69211139838770208, -14.75429553128187798, -0.6577119969999878357 ) ) ;
#2927 = CARTESIAN_POINT ( 'NONE',  ( -17.83931601609999973, 20.00000000000000000, 230.0000000010000178 ) ) ;
#2928 = CARTESIAN_POINT ( 'NONE',  ( 24.37821946547973084, -14.76389286113969490, 4.791564337000009388 ) ) ;
#2929 = DIRECTION ( 'NONE',  ( -1.000000000000000000, 0.000000000000000000, -2.257144471330000330E-12 ) ) ;
#2930 = B_SPLINE_CURVE_WITH_KNOTS ( 'NONE', 3,
 ( #11893, #31094, #14885, #19443, #9537, #28725, #29034, #7628, #1027, #22729, #17534 ),
 .UNSPECIFIED., .F., .F.,
 ( 4, 1, 1, 1, 2, 2, 4 ),
 ( 0.000000000000000000, 0.2500000000000151545, 0.3750000000000210387, 0.4375000000000270894, 0.4687500000000269784, 0.5000000000000268674, 1.000000000000000000 ),
 .UNSPECIFIED. ) ;
#2931 = CARTESIAN_POINT ( 'NONE',  ( -3.378474373710000034, -11.51459555979999827, 232.0000000000000000 ) ) ;
#2932 = CARTESIAN_POINT ( 'NONE',  ( 15.69372571266449512, 10.97998838177520931, 0.5194763363741546902 ) ) ;
#2933 = ORIENTED_EDGE ( 'NONE', *, *, #11376, .T. ) ;
#2934 = EDGE_CURVE ( 'NONE', #4374, #6881, #14629, .T. ) ;
#2935 = DIRECTION ( 'NONE',  ( -1.180736691910036071E-13, -0.9986295347540310452, -0.05233595625330160483 ) ) ;
#2936 = CARTESIAN_POINT ( 'NONE',  ( -24.91946588839999777, -13.83134141909999926, 223.9971936000000028 ) ) ;
#2937 = CARTESIAN_POINT ( 'NONE',  ( 25.00924755590000004, -13.66774365989999929, 225.9012973829999851 ) ) ;
#2938 = CIRCLE ( 'NONE', #13495, 4.000000000000001776 ) ;
#2939 = CARTESIAN_POINT ( 'NONE',  ( 5.242919931573567283, -2.735361231296036699, -61.79790713612500497 ) ) ;
#2940 = ORIENTED_EDGE ( 'NONE', *, *, #29110, .T. ) ;
#2941 = ORIENTED_EDGE ( 'NONE', *, *, #26796, .T. ) ;
#2943 = CARTESIAN_POINT ( 'NONE',  ( -8.999999999299999942, 20.99999999999999645, -58.10000000000000142 ) ) ;
#2942 = VECTOR ( 'NONE', #8951, 1000.000000000000114 ) ;
#2944 = VERTEX_POINT ( 'NONE', #15796 ) ;
#2945 = ORIENTED_EDGE ( 'NONE', *, *, #23441, .T. ) ;
#2946 = DIRECTION ( 'NONE',  ( 1.000000000000000000, 0.000000000000000000, 0.000000000000000000 ) ) ;
#2947 = CARTESIAN_POINT ( 'NONE',  ( -24.20792486932886689, 13.66932879934886813, 3.920132063000014710 ) ) ;
#2948 = DIRECTION ( 'NONE',  ( -0.9595496299847263710, 0.2815395311429191305, 0.000000000000000000 ) ) ;
#2949 = CARTESIAN_POINT ( 'NONE',  ( 4.497730495419999919, 11.38816151149999989, 232.6627648150000027 ) ) ;
#2950 = APPLICATION_CONTEXT ( 'automotive_design' ) ;
#2951 = CARTESIAN_POINT ( 'NONE',  ( 24.44014313072642963, -13.24968496497942105, 6.079865069000017996 ) ) ;
#2952 = CARTESIAN_POINT ( 'NONE',  ( -3.099128499470596765, -3.102542665468459138, -9.313991631000007487 ) ) ;
#2953 = CARTESIAN_POINT ( 'NONE',  ( 27.56257419720000357, -7.220571643900000502, 230.5592437530000041 ) ) ;
#2954 = ORIENTED_EDGE ( 'NONE', *, *, #15780, .F. ) ;
#2955 = CARTESIAN_POINT ( 'NONE',  ( 2.594524747302418444, -3.974221016099061199, -44.10000000002499121 ) ) ;
#2956 = CARTESIAN_POINT ( 'NONE',  ( 24.45473033137484720, 14.63622297804190175, 3.901342939999996595 ) ) ;
#2957 = VECTOR ( 'NONE', #27758, 999.9999999999998863 ) ;
#2958 = CARTESIAN_POINT ( 'NONE',  ( -0.9576357401321299312, 5.433995450232204760, -20.83583244400000467 ) ) ;
#2959 = DIRECTION ( 'NONE',  ( 0.000000000000000000, -1.000000000000000000, 0.000000000000000000 ) ) ;
#2960 = DIRECTION ( 'NONE',  ( -0.7600087925169251024, -0.4151946956549595336, 0.4999999999969509945 ) ) ;
#2961 = EDGE_CURVE ( 'NONE', #8590, #22717, #30442, .T. ) ;
#2962 = FACE_OUTER_BOUND ( 'NONE', #28524, .T. ) ;
#2963 = FACE_OUTER_BOUND ( 'NONE', #28015, .T. ) ;
#2964 = CARTESIAN_POINT ( 'NONE',  ( -6.340437944841875506, 0.6332316896323284539, -47.62737393802499497 ) ) ;
#2965 = EDGE_CURVE ( 'NONE', #26221, #18457, #27720, .T. ) ;
#2966 = CARTESIAN_POINT ( 'NONE',  ( 10.69999999999900986, -25.58868802767188555, -25.72767439674187528 ) ) ;
#2967 = ADVANCED_FACE ( 'NONE', ( #20992 ), #9023, .F. ) ;
#2968 = CARTESIAN_POINT ( 'NONE',  ( 0.9003585010983619075, -26.78512143669438572, 224.3665129619594154 ) ) ;
#2969 = LINE ( 'NONE', #15231, #26882 ) ;
#2970 = AXIS2_PLACEMENT_3D ( 'NONE', #23758, #11788, #21394 ) ;
#2971 = CARTESIAN_POINT ( 'NONE',  ( -24.20493445730000204, 13.42713550600000083, 229.9751247330000012 ) ) ;
#2972 = EDGE_CURVE ( 'NONE', #28085, #1347, #19245, .T. ) ;
#2973 = B_SPLINE_CURVE_WITH_KNOTS ( 'NONE', 5,
 ( #11116, #27950, #13630, #1676, #27784, #16452, #13783, #6231, #11583, #15840, #20879, #18653, #18504, #28416, #30311 ),
 .UNSPECIFIED., .F., .F.,
 ( 6, 3, 3, 3, 6 ),
 ( 0.000000000000000000, 0.2999999999986154298, 0.6000000000006923129, 0.7999999999996538769, 1.000000000000000000 ),
 .UNSPECIFIED. ) ;
#2974 = DIRECTION ( 'NONE',  ( -1.000000000000000000, 0.000000000000000000, 0.000000000000000000 ) ) ;
#2975 = EDGE_LOOP ( 'NONE', ( #13463, #826, #26860, #5305, #15473, #13542, #20696, #23812, #24583, #29901 ) ) ;
#2976 = CARTESIAN_POINT ( 'NONE',  ( 2.039164074698236906, -5.746172002732055084, -30.25632401680000783 ) ) ;
#2977 = ORIENTED_EDGE ( 'NONE', *, *, #13679, .F. ) ;
#2978 = CARTESIAN_POINT ( 'NONE',  ( 24.35797964201644561, -13.39969403546014703, 3.901342130000013064 ) ) ;
#2979 = CARTESIAN_POINT ( 'NONE',  ( 4.085013927406620837, 4.246146200131522441, -49.49426496242500662 ) ) ;
#2980 = ORIENTED_EDGE ( 'NONE', *, *, #24318, .F. ) ;
#2981 = ORIENTED_EDGE ( 'NONE', *, *, #14905, .F. ) ;
#2982 = CARTESIAN_POINT ( 'NONE',  ( 0.000000000000000000, 0.000000000000000000, 0.000000000000000000 ) ) ;
#2983 = ORIENTED_EDGE ( 'NONE', *, *, #8777, .F. ) ;
#2984 = ORIENTED_EDGE ( 'NONE', *, *, #7926, .T. ) ;
#2985 = B_SPLINE_CURVE_WITH_KNOTS ( 'NONE', 3,
 ( #8256, #15503, #17398, #3080, #29356, #19774, #22445, #17548, #8101, #22133, #27159, #741, #15355, #7801, #8844, #24953, #29671, #10333, #27004, #15195, #25109, #15052, #6491, #24799, #3385, #5442 ),
 .UNSPECIFIED., .F., .F.,
 ( 4, 2, 2, 2, 2, 2, 2, 2, 2, 2, 2, 2, 4 ),
 ( 0.000000000000000000, 0.001576840078853145944, 0.002365260118279718590, 0.003153680157706291454, 0.004730520236559437181, 0.005518940275986006574, 0.006307360315412575101, 0.007884200394265702613, 0.008672620433692270273, 0.009461040473118836197, 0.01024946051254540386, 0.01103788055197197152, 0.01261472063082510336 ),
 .UNSPECIFIED. ) ;
#2986 = CARTESIAN_POINT ( 'NONE',  ( 24.34123158960000310, -14.82477075290000101, 225.9012998019999827 ) ) ;
#2987 = CARTESIAN_POINT ( 'NONE',  ( 24.36724935763797006, 13.38201651305720574, 4.999998581000003384 ) ) ;
#2988 = CARTESIAN_POINT ( 'NONE',  ( 19.80526555962148549, 19.50877392102342256, 1.000000000000000888 ) ) ;
#2989 = CARTESIAN_POINT ( 'NONE',  ( 5.797918472256613498, -5.490503403373238278, -26.84307236410781172 ) ) ;
#2990 = TOROIDAL_SURFACE ( 'NONE', #17049, 24.50000000000000000, 3.200000000000000178 ) ;
#2991 = CARTESIAN_POINT ( 'NONE',  ( 3.760007715734311251, -19.71206033701148996, -27.86495495698533986 ) ) ;
#2992 = CARTESIAN_POINT ( 'NONE',  ( -3.738201190122705686, 2.321745386530837063, -0.6999999999999992895 ) ) ;
#2993 = DIRECTION ( 'NONE',  ( -1.000000000000000000, 3.980999999999999294E-12, -1.940999999999999504E-12 ) ) ;
#2994 = CARTESIAN_POINT ( 'NONE',  ( -10.69999999995387263, -31.36675497167934523, -21.96261822718243550 ) ) ;
#2995 = ORIENTED_EDGE ( 'NONE', *, *, #4104, .T. ) ;
#2996 = CARTESIAN_POINT ( 'NONE',  ( -3.950034095761355335, 2.484763540022569384, -10.44547590280000371 ) ) ;
#2997 = CARTESIAN_POINT ( 'NONE',  ( 4.556810990865953315, -1.030009251744165688, -32.78377053309999667 ) ) ;
#2998 = CARTESIAN_POINT ( 'NONE',  ( -6.999999999884560786, -60.75400889059761766, -3.446705952697758590 ) ) ;
#2999 = CARTESIAN_POINT ( 'NONE',  ( -13.00000000000000000, 22.06507305262541863, -61.91147751336289673 ) ) ;
#3000 = CARTESIAN_POINT ( 'NONE',  ( 19.76603533419210734, 19.51852340513930173, 0.7754612589999931860 ) ) ;
#3001 = CARTESIAN_POINT ( 'NONE',  ( -23.70578532293623653, -13.93854223005088677, 226.0877068035740365 ) ) ;
#3002 = CARTESIAN_POINT ( 'NONE',  ( 0.3832430167449999980, -28.49789927060000139, 226.0423291289999952 ) ) ;
#3003 = CARTESIAN_POINT ( 'NONE',  ( -3.554763430470064822, 2.566410659217317924, -34.46696136359999940 ) ) ;
#3004 = LINE ( 'NONE', #355, #22263 ) ;
#3005 = CARTESIAN_POINT ( 'NONE',  ( -11.50000000044500048, -20.99999999999999645, -28.40000000000541647 ) ) ;
#3006 = CARTESIAN_POINT ( 'NONE',  ( 1.290941959522689864, -3.499733189061704053, 230.7123227554298239 ) ) ;
#3007 = EDGE_LOOP ( 'NONE', ( #29827, #3088, #16719, #9279 ) ) ;
#3008 = CARTESIAN_POINT ( 'NONE',  ( -4.861312627709997614, 3.765626869323773995, -39.31578811167095466 ) ) ;
#3009 = CARTESIAN_POINT ( 'NONE',  ( -3.791072893346491224, -19.87502547375133588, -27.78547154899721150 ) ) ;
#3010 = ORIENTED_EDGE ( 'NONE', *, *, #30863, .T. ) ;
#3011 = CARTESIAN_POINT ( 'NONE',  ( 28.43512364494067413, 3.824800618850225931, 8.000000000000007105 ) ) ;
#3012 = CYLINDRICAL_SURFACE ( 'NONE', #10224, 1.999999999999999778 ) ;
#3013 = ORIENTED_EDGE ( 'NONE', *, *, #8927, .F. ) ;
#3014 = CARTESIAN_POINT ( 'NONE',  ( -4.685889913869174528, 0.7077737262620402703, -44.10000000002499121 ) ) ;
#3015 = ORIENTED_EDGE ( 'NONE', *, *, #26276, .T. ) ;
#3016 = ORIENTED_EDGE ( 'NONE', *, *, #15574, .T. ) ;
#3017 = ORIENTED_EDGE ( 'NONE', *, *, #2577, .T. ) ;
#3018 = CARTESIAN_POINT ( 'NONE',  ( 25.41683733030000170, 14.11523383709999990, 229.4982322489999831 ) ) ;
#3019 = CARTESIAN_POINT ( 'NONE',  ( -16.56625540809453057, 12.07698932566918160, -0.6999999999999784173 ) ) ;
#3020 = EDGE_CURVE ( 'NONE', #31086, #17565, #15659, .T. ) ;
#3021 = CARTESIAN_POINT ( 'NONE',  ( -7.999999999659364924, -18.23057825131764531, -36.55854538514943641 ) ) ;
#3022 = ORIENTED_EDGE ( 'NONE', *, *, #2152, .T. ) ;
#3023 = CARTESIAN_POINT ( 'NONE',  ( -24.44014312407112399, 13.24968496200000523, 6.079865069000017996 ) ) ;
#3024 = AXIS2_PLACEMENT_3D ( 'NONE', #24862, #17303, #22189 ) ;
#3025 = CARTESIAN_POINT ( 'NONE',  ( 0.4125558677674681096, -28.49726274111934998, 6.095949245000009675 ) ) ;
#3026 = CARTESIAN_POINT ( 'NONE',  ( -13.99999999969999820, 20.99999999999999645, -67.09999999999999432 ) ) ;
#3027 = DIRECTION ( 'NONE',  ( 0.3633921898465291567, 0.9316362575375349842, 0.000000000000000000 ) ) ;
#3028 = EDGE_CURVE ( 'NONE', #21131, #24086, #21614, .T. ) ;
#3029 = CARTESIAN_POINT ( 'NONE',  ( 4.239428892460699881E-14, 6.006117008548172241E-13, 232.1412452697749984 ) ) ;
#3030 = CARTESIAN_POINT ( 'NONE',  ( -0.7560282158644084927, 4.289996408053712962, -19.83583244400000112 ) ) ;
#3031 = CARTESIAN_POINT ( 'NONE',  ( -16.83342759559999635, -9.000000000000001776, -0.6999999999999992895 ) ) ;
#3032 = CARTESIAN_POINT ( 'NONE',  ( -0.9895645760634798060, -27.48220350681653557, 5.485672168196345844 ) ) ;
#3033 = CARTESIAN_POINT ( 'NONE',  ( 3.941323043105160018, -19.53988727930733305, -27.94892936810068207 ) ) ;
#3034 = PLANE ( 'NONE',  #12724 ) ;
#3035 = AXIS2_PLACEMENT_3D ( 'NONE', #2028, #23438, #23591 ) ;
#3036 = CARTESIAN_POINT ( 'NONE',  ( -8.699999999786642846, -67.40749995144571471, -17.04319545400634084 ) ) ;
#3037 = CARTESIAN_POINT ( 'NONE',  ( 26.80000000000000071, -3.552713678799999608E-15, 193.2171415880000040 ) ) ;
#3038 = CARTESIAN_POINT ( 'NONE',  ( -27.50000000000000000, 3.367667473009999970E-15, 0.000000000000000000 ) ) ;
#3039 = CARTESIAN_POINT ( 'NONE',  ( -17.91346663230000047, 3.647998880369999863, 230.6999999999999886 ) ) ;
#3040 = ORIENTED_EDGE ( 'NONE', *, *, #20095, .F. ) ;
#3041 = CARTESIAN_POINT ( 'NONE',  ( 0.7192951553310067414, 4.518739695591652783, -54.01500058692499806 ) ) ;
#3042 = B_SPLINE_CURVE_WITH_KNOTS ( 'NONE', 5,
 ( #16125, #11870, #2287, #9346, #14086, #11567 ),
 .UNSPECIFIED., .F., .F.,
 ( 6, 6 ),
 ( 3.365644447000000206, 3.604192656009999940 ),
 .UNSPECIFIED. ) ;
#3043 = FACE_OUTER_BOUND ( 'NONE', #28369, .T. ) ;
#3044 = COLOUR_RGB ( '', 0.66274510, 0.83137255, 0.94901961) ;
#3045 = CARTESIAN_POINT ( 'NONE',  ( -18.03439342504434606, 20.21871256385842841, 0.02487531600001147147 ) ) ;
#3046 = CARTESIAN_POINT ( 'NONE',  ( -4.256836137300013867, 0.9512594216477614495, -68.10000000002500542 ) ) ;
#3047 = EDGE_CURVE ( 'NONE', #3834, #17179, #12007, .T. ) ;
#3048 = EDGE_LOOP ( 'NONE', ( #26864, #12144, #12878, #9117 ) ) ;
#3049 = CARTESIAN_POINT ( 'NONE',  ( 24.34131725955728598, -12.79741914641014411, 5.217924950592947475 ) ) ;
#3050 = ORIENTED_EDGE ( 'NONE', *, *, #8582, .F. ) ;
#3051 = CARTESIAN_POINT ( 'NONE',  ( -24.37165444408190851, 14.77472139917419369, 4.999998581000003384 ) ) ;
#3052 = CARTESIAN_POINT ( 'NONE',  ( -10.69999999999999929, 19.99999999999999645, -42.39999999999999858 ) ) ;
#3053 = ORIENTED_EDGE ( 'NONE', *, *, #10857, .T. ) ;
#3054 = CARTESIAN_POINT ( 'NONE',  ( -1.266353310550808464, -4.943458602710906646, -28.48632611460000419 ) ) ;
#3055 = DIRECTION ( 'NONE',  ( 0.000000000000000000, -0.9128796883888952163, 0.4082287037029533328 ) ) ;
#3056 = CARTESIAN_POINT ( 'NONE',  ( -28.45300238704230367, -0.5177135156027357077, 0.5017677510000262409 ) ) ;
#3057 = DIRECTION ( 'NONE',  ( 0.000000000000000000, 0.000000000000000000, 1.000000000000000000 ) ) ;
#3058 = DIRECTION ( 'NONE',  ( 0.000000000000000000, 0.000000000000000000, 1.000000000000000000 ) ) ;
#3059 = EDGE_CURVE ( 'NONE', #5518, #24435, #31054, .T. ) ;
#3060 = CARTESIAN_POINT ( 'NONE',  ( -27.79539923781770483, -0.5057481688778011630, 1.000000000000000888 ) ) ;
#3061 = ORIENTED_EDGE ( 'NONE', *, *, #15221, .T. ) ;
#3062 = UNCERTAINTY_MEASURE_WITH_UNIT (LENGTH_MEASURE( 1.000000000000000082E-05 ), #18882, 'distance_accuracy_value', 'NONE');
#3063 = CARTESIAN_POINT ( 'NONE',  ( -26.93395387809999875, 3.298349105260000080E-15, 42.24324102359999955 ) ) ;
#3064 = CARTESIAN_POINT ( 'NONE',  ( 23.24663841809999809, -14.69162354060000020, 5.000000000000000000 ) ) ;
#3065 = ORIENTED_EDGE ( 'NONE', *, *, #7121, .T. ) ;
#3066 = DIRECTION ( 'NONE',  ( -1.000000000000000000, 5.665498452320000818E-16, 0.000000000000000000 ) ) ;
#3067 = FACE_OUTER_BOUND ( 'NONE', #13010, .T. ) ;
#3068 = CARTESIAN_POINT ( 'NONE',  ( -11.53315104089999998, 3.551884179650000029, 231.9999989789999972 ) ) ;
#3069 = CARTESIAN_POINT ( 'NONE',  ( 4.638687372170419820, -20.50181238079150248, -27.47976714834732448 ) ) ;
#3070 = CARTESIAN_POINT ( 'NONE',  ( 9.999999999959999997, -25.00000000000000000, -26.16393202319999745 ) ) ;
#3071 = CARTESIAN_POINT ( 'NONE',  ( -5.395560604220499101, -26.25584002662961680, 209.2195618656424756 ) ) ;
#3072 = CARTESIAN_POINT ( 'NONE',  ( 2.746047774209056325, -3.024004467141764962, -0.6999999999999992895 ) ) ;
#3073 = CARTESIAN_POINT ( 'NONE',  ( -27.42665334337451455, -7.720805503521760649, -0.5592437529999827461 ) ) ;
#3074 = CARTESIAN_POINT ( 'NONE',  ( 1.100000000000000089, -27.47799119230000287, 5.000000000000000000 ) ) ;
#3075 = EDGE_CURVE ( 'NONE', #359, #15474, #7131, .T. ) ;
#3076 = CARTESIAN_POINT ( 'NONE',  ( -10.69999999997499351, -27.78484171395010804, -31.32227941850083397 ) ) ;
#3077 = CARTESIAN_POINT ( 'NONE',  ( -10.69999999999999929, -30.00000000000000000, -28.40000000000000213 ) ) ;
#3078 = ADVANCED_FACE ( 'NONE', ( #17186 ), #16042, .T. ) ;
#3079 = VECTOR ( 'NONE', #21701, 1000.000000000000000 ) ;
#3080 = CARTESIAN_POINT ( 'NONE',  ( -9.544994065185523624, -25.04267878452547080, 26.16927719407518538 ) ) ;
#3081 = CARTESIAN_POINT ( 'NONE',  ( 26.80000000069999899, -3.281945028320000125E-15, 65.00000000000000000 ) ) ;
#3082 = ORIENTED_EDGE ( 'NONE', *, *, #15426, .T. ) ;
#3083 = CARTESIAN_POINT ( 'NONE',  ( 3.458129700889219116, -0.5397582531354582214, 226.6412452697749984 ) ) ;
#3084 = EDGE_CURVE ( 'NONE', #8540, #29211, #2419, .T. ) ;
#3085 = CARTESIAN_POINT ( 'NONE',  ( -10.69999999895494192, -23.79999999999999716, -28.40000000000000213 ) ) ;
#3086 = CARTESIAN_POINT ( 'NONE',  ( 1.387947292976102087, 4.364053279572885025, -60.46492395752500215 ) ) ;
#3087 = ORIENTED_EDGE ( 'NONE', *, *, #6006, .T. ) ;
#3088 = ORIENTED_EDGE ( 'NONE', *, *, #24827, .T. ) ;
#3090 = EDGE_CURVE ( 'NONE', #18763, #3434, #12155, .T. ) ;
#3089 = CARTESIAN_POINT ( 'NONE',  ( 23.40723432809949855, -19.94412562524615140, 0.5514312830000311916 ) ) ;
#3091 = ORIENTED_EDGE ( 'NONE', *, *, #11250, .T. ) ;
#3092 = ORIENTED_EDGE ( 'NONE', *, *, #28090, .T. ) ;
#3093 = CARTESIAN_POINT ( 'NONE',  ( 17.00199035030329497, 12.09718743885649950, -0.6999999999999783062 ) ) ;
#3094 = CARTESIAN_POINT ( 'NONE',  ( -23.70218820198384080, -12.50899637883967053, 225.4229804101834986 ) ) ;
#3095 = DIRECTION ( 'NONE',  ( 1.000000000000000000, 0.000000000000000000, 0.000000000000000000 ) ) ;
#3096 = VECTOR ( 'NONE', #14509, 1000.000000000000000 ) ;
#3097 = UNCERTAINTY_MEASURE_WITH_UNIT (LENGTH_MEASURE( 1.000000000000000082E-05 ), #5843, 'distance_accuracy_value', 'NONE');
#3098 = CARTESIAN_POINT ( 'NONE',  ( 8.011542175009999767, -9.024668540559998675, 231.9999991140000191 ) ) ;
#3099 = CARTESIAN_POINT ( 'NONE',  ( 24.82162974202869421, -12.51998933900577349, 5.310645680000003921 ) ) ;
#3100 = CARTESIAN_POINT ( 'NONE',  ( -16.83342759575507586, 10.99999999997565503, -0.6999999999999784173 ) ) ;
#3101 = VERTEX_POINT ( 'NONE', #16878 ) ;
#3102 = CARTESIAN_POINT ( 'NONE',  ( 2.824297055372420040, -3.680463102343676240, -44.10000000002499121 ) ) ;
#3103 = AXIS2_PLACEMENT_3D ( 'NONE', #24128, #2106, #14381 ) ;
#3104 = CARTESIAN_POINT ( 'NONE',  ( -24.92639508767336309, -13.81781708088548122, 4.493023692000025271 ) ) ;
#3105 = EDGE_CURVE ( 'NONE', #8755, #29481, #4231, .T. ) ;
#3106 = CARTESIAN_POINT ( 'NONE',  ( -6.202057249109299342, 1.908294659314309305, -22.32289663399999924 ) ) ;
#3107 = CARTESIAN_POINT ( 'NONE',  ( 27.65104940643587383, 3.057637721010480814, 8.000000000000007105 ) ) ;
#3108 = CARTESIAN_POINT ( 'NONE',  ( -0.6094664100040195764, -28.49364619262437870, 4.999998581000003384 ) ) ;
#3109 = CARTESIAN_POINT ( 'NONE',  ( 25.94284618478187809, -6.948772836044536660, 86.78285841113334698 ) ) ;
#3110 = LINE ( 'NONE', #15079, #29240 ) ;
#3111 = CARTESIAN_POINT ( 'NONE',  ( 1.634888019277636051, 4.633891277622259608, -45.49079303332499791 ) ) ;
#3112 = DIRECTION ( 'NONE',  ( 0.000000000000000000, -2.257145581549999994E-12, -1.000000000000000000 ) ) ;
#3113 = CYLINDRICAL_SURFACE ( 'NONE', #30869, 2.500000000000001776 ) ;
#3114 = CARTESIAN_POINT ( 'NONE',  ( -10.69999999999999929, -29.06671945329999929, -26.22544931050000017 ) ) ;
#3115 = DIRECTION ( 'NONE',  ( -1.000000000000000000, 0.000000000000000000, 0.000000000000000000 ) ) ;
#3116 = VECTOR ( 'NONE', #15262, 1000.000000000000000 ) ;
#3117 = CARTESIAN_POINT ( 'NONE',  ( 9.738910687886866313, -24.96785170200598714, 27.46685764687258313 ) ) ;
#3118 = ORIENTED_EDGE ( 'NONE', *, *, #19072, .T. ) ;
#3119 = PRODUCT ( 'Washer', 'Washer', '', ( #13822 ) ) ;
#3120 = CARTESIAN_POINT ( 'NONE',  ( -4.702124758411583727, -0.9170245833456597273, -32.03402066320000330 ) ) ;
#3121 = VERTEX_POINT ( 'NONE', #9644 ) ;
#3122 = LINE ( 'NONE', #13178, #24819 ) ;
#3123 = CARTESIAN_POINT ( 'NONE',  ( -0.8137756071791968360, 4.795696781221863603, -52.00792092402499378 ) ) ;
#3124 = ORIENTED_EDGE ( 'NONE', *, *, #10955, .T. ) ;
#3125 = EDGE_LOOP ( 'NONE', ( #20310, #17564, #15234, #8392 ) ) ;
#3126 = CARTESIAN_POINT ( 'NONE',  ( -12.27456665182842244, -28.21308863598467553, -11.26611098211190587 ) ) ;
#3127 = EDGE_LOOP ( 'NONE', ( #7404, #13071, #30892, #11102, #5046, #28053 ) ) ;
#3128 = APPLICATION_CONTEXT ( 'automotive_design' ) ;
#3129 = EDGE_CURVE ( 'NONE', #4371, #5093, #26335, .T. ) ;
#3130 = ORIENTED_EDGE ( 'NONE', *, *, #25626, .F. ) ;
#3131 = CARTESIAN_POINT ( 'NONE',  ( 16.09014176772306826, -8.731615745635396664, -4.336808689942017243E-16 ) ) ;
#3132 = CARTESIAN_POINT ( 'NONE',  ( 24.86822223037987456, 13.92223202030449691, 4.319317656000021266 ) ) ;
#3133 = CARTESIAN_POINT ( 'NONE',  ( -1.033595436889999888E-13, -27.50000000069999828, 3.899999999999999911 ) ) ;
#3134 = LINE ( 'NONE', #19975, #24510 ) ;
#3135 = EDGE_CURVE ( 'NONE', #25355, #10318, #12027, .T. ) ;
#3136 = EDGE_CURVE ( 'NONE', #7840, #28202, #19405, .T. ) ;
#3137 = LINE ( 'NONE', #12736, #9564 ) ;
#3138 = CARTESIAN_POINT ( 'NONE',  ( -4.687286842521976027, -2.264969778146401769, -0.6999999999999992895 ) ) ;
#3139 = CARTESIAN_POINT ( 'NONE',  ( 9.000000000029999114, 21.35000000040000145, -60.10000000000000142 ) ) ;
#3140 = AXIS2_PLACEMENT_3D ( 'NONE', #14395, #21162, #18948 ) ;
#3141 = CARTESIAN_POINT ( 'NONE',  ( -9.993285220779425160, -25.61999708228226069, 86.39444872359999295 ) ) ;
#3142 = CARTESIAN_POINT ( 'NONE',  ( -21.81271764029508731, 17.27884132338922285, 6.000000042999998229 ) ) ;
#3143 = CARTESIAN_POINT ( 'NONE',  ( -4.363437395929419260, 0.1294788321584625090, -13.18304957890000573 ) ) ;
#3144 = CARTESIAN_POINT ( 'NONE',  ( -5.414567903583902719, -1.055967702048432599, -30.09652066319999975 ) ) ;
#3145 = DIRECTION ( 'NONE',  ( 0.000000000000000000, 0.000000000000000000, 1.000000000000000000 ) ) ;
#3146 = CARTESIAN_POINT ( 'NONE',  ( 24.32472894995379420, -13.45989151107506387, 6.099998581000020792 ) ) ;
#3147 = CARTESIAN_POINT ( 'NONE',  ( -24.49868928475705943, -13.14068576356688922, 225.6775953917510265 ) ) ;
#3148 = FACE_OUTER_BOUND ( 'NONE', #1111, .T. ) ;
#3149 = CARTESIAN_POINT ( 'NONE',  ( 11.69999999989999928, 19.99999999999999645, -2.399999999999999467 ) ) ;
#3150 = B_SPLINE_CURVE_WITH_KNOTS ( 'NONE', 3,
 ( #8507, #10890, #30082, #13559, #6001, #15915, #27875, #25370, #20639, #15600, #25051, #28026 ),
 .UNSPECIFIED., .F., .F.,
 ( 4, 2, 2, 2, 2, 4 ),
 ( 0.000000000000000000, 0.1250000000000004441, 0.2500000000000008882, 0.5000000000000005551, 0.7500000000000003331, 1.000000000000000000 ),
 .UNSPECIFIED. ) ;
#3151 = DIRECTION ( 'NONE',  ( 0.000000000000000000, 0.000000000000000000, 1.000000000000000000 ) ) ;
#3152 = CARTESIAN_POINT ( 'NONE',  ( -8.699999999674142614, -13.61360970150653316, -34.64062719139432289 ) ) ;
#3153 = CARTESIAN_POINT ( 'NONE',  ( 23.80322556508107112, 14.59355840047072661, 1.000000000000000888 ) ) ;
#3154 = EDGE_LOOP ( 'NONE', ( #4420, #4293, #16099, #4034, #3458, #24419 ) ) ;
#3155 = CARTESIAN_POINT ( 'NONE',  ( 8.000000000232340369, -25.77531388888444752, -25.66136093478154123 ) ) ;
#3156 = CARTESIAN_POINT ( 'NONE',  ( -5.226724280842381276, -31.46509748598739975, -80.33068845215250064 ) ) ;
#3157 = EDGE_LOOP ( 'NONE', ( #25969, #6804, #3794, #5773 ) ) ;
#3158 = CARTESIAN_POINT ( 'NONE',  ( 3.466821295769682159E-14, -2.890242878314739659E-13, 27.99999999999999645 ) ) ;
#3159 = FACE_OUTER_BOUND ( 'NONE', #2217, .T. ) ;
#3160 = ORIENTED_EDGE ( 'NONE', *, *, #845, .T. ) ;
#3161 = CARTESIAN_POINT ( 'NONE',  ( -9.944225187684255118, -25.63929276476996222, 26.94086061512460262 ) ) ;
#3162 = ORIENTED_EDGE ( 'NONE', *, *, #7689, .F. ) ;
#3163 = ORIENTED_EDGE ( 'NONE', *, *, #27536, .F. ) ;
#3164 =( NAMED_UNIT ( * ) PLANE_ANGLE_UNIT ( ) SI_UNIT ( $, .RADIAN. ) );
#3165 = B_SPLINE_CURVE_WITH_KNOTS ( 'NONE', 3,
 ( #28898, #2472, #11602, #120, #28435, #23885, #4981, #19457, #9700, #2324, #4522, #2621, #28593, #11753, #29050, #21360, #30955, #9382 ),
 .UNSPECIFIED., .F., .F.,
 ( 4, 2, 2, 2, 2, 2, 2, 2, 4 ),
 ( 0.000000000000000000, 0.1250000000000000000, 0.2500000000000000000, 0.3750000000000000000, 0.5000000000000000000, 0.6250000000000000000, 0.7500000000000000000, 0.8750000000000000000, 1.000000000000000000 ),
 .UNSPECIFIED. ) ;
#3166 = VERTEX_POINT ( 'NONE', #28993 ) ;
#3167 = DIRECTION ( 'NONE',  ( 1.000000000000000000, 0.000000000000000000, 0.000000000000000000 ) ) ;
#3168 = CARTESIAN_POINT ( 'NONE',  ( -24.49999999470000134, 3.000285566209999917E-15, 89.99999999930000172 ) ) ;
#3169 = DIRECTION ( 'NONE',  ( -1.000000000000000000, -8.816454510895967384E-12, 0.000000000000000000 ) ) ;
#3170 = CARTESIAN_POINT ( 'NONE',  ( 10.70000000009999930, -27.00000000000000000, -28.39999999989999679 ) ) ;
#3171 = CARTESIAN_POINT ( 'NONE',  ( -250010.8602219996974, -207625.5434020000102, -380034.9847440001322 ) ) ;
#3172 = EDGE_CURVE ( 'NONE', #17104, #4684, #4618, .T. ) ;
#3173 = CARTESIAN_POINT ( 'NONE',  ( 25.77914806503467560, 15.40383291000323318, 1.000000000000000888 ) ) ;
#3174 = ADVANCED_FACE ( 'NONE', ( #26638 ), #14686, .F. ) ;
#3175 = CARTESIAN_POINT ( 'NONE',  ( 8.416763499243900881, -26.18199973230927924, 206.9245629863210354 ) ) ;
#3176 = CARTESIAN_POINT ( 'NONE',  ( 10.00000000070000183, 19.99999999999999645, -42.39999999999999858 ) ) ;
#3177 = AXIS2_PLACEMENT_3D ( 'NONE', #3188, #24602, #22240 ) ;
#3178 = ORIENTED_EDGE ( 'NONE', *, *, #23303, .T. ) ;
#3179 = VECTOR ( 'NONE', #11020, 1000.000000000000000 ) ;
#3180 = CARTESIAN_POINT ( 'NONE',  ( 3.112737406813101515, -4.802415649948616583, -0.7659393883000034098 ) ) ;
#3181 = CARTESIAN_POINT ( 'NONE',  ( -3.664565019602479268, -2.682238183793479447, -17.93504627010000618 ) ) ;
#3182 = STYLED_ITEM ( 'NONE', ( #21246 ), #6893 ) ;
#3183 = CARTESIAN_POINT ( 'NONE',  ( 3.760007715734309475, -21.02717377737872795, -30.56133709588283409 ) ) ;
#3184 = CARTESIAN_POINT ( 'NONE',  ( -0.5621952391521564119, -27.49459032466129926, 5.956950222287991537 ) ) ;
#3185 = AXIS2_PLACEMENT_3D ( 'NONE', #21699, #12091, #24065 ) ;
#3186 = CARTESIAN_POINT ( 'NONE',  ( 23.53263993711012603, -14.22965940713208255, 225.9595466040883878 ) ) ;
#3187 = CARTESIAN_POINT ( 'NONE',  ( -25.46187654339999895, 14.12439703469999941, 229.2404163060000144 ) ) ;
#3188 = CARTESIAN_POINT ( 'NONE',  ( 13.99999999979999821, 20.99999999999999645, -51.10000000000000142 ) ) ;
#3189 = CARTESIAN_POINT ( 'NONE',  ( 26.84464183999999776, -3.287411896319999731E-15, 192.5624961750000068 ) ) ;
#3190 = CARTESIAN_POINT ( 'NONE',  ( 21.99374050320000151, 17.63454380079999950, 229.0000000010000178 ) ) ;
#3191 = CARTESIAN_POINT ( 'NONE',  ( 1.850829058368554492, -3.930924299794261056, -38.89973510835294235 ) ) ;
#3192 = EDGE_LOOP ( 'NONE', ( #5990, #23265, #16706, #1155 ) ) ;
#3193 = CARTESIAN_POINT ( 'NONE',  ( 4.569612387855602087, -0.08076758077263958280, -57.69793411332500455 ) ) ;
#3194 = CARTESIAN_POINT ( 'NONE',  ( -8.699999999677118012, -17.14683147485207471, -33.31409708255895907 ) ) ;
#3195 = B_SPLINE_CURVE_WITH_KNOTS ( 'NONE', 1,
 ( #25574, #11405 ),
 .UNSPECIFIED., .F., .F.,
 ( 2, 2 ),
 ( -2.557517314480000010E-06, 0.7000000000009999335 ),
 .UNSPECIFIED. ) ;
#3196 = CARTESIAN_POINT ( 'NONE',  ( -22.00340350502675690, 17.51493346882343261, 0.5514279790000131687 ) ) ;
#3197 = CARTESIAN_POINT ( 'NONE',  ( -4.293412589747293673, 1.066240861064407408, -68.10000000002500542 ) ) ;
#3198 = AXIS2_PLACEMENT_3D ( 'NONE', #4562, #14164, #7076 ) ;
#3199 = ORIENTED_EDGE ( 'NONE', *, *, #9216, .F. ) ;
#3201 = EDGE_CURVE ( 'NONE', #24684, #1347, #376, .T. ) ;
#3200 = AXIS2_PLACEMENT_3D ( 'NONE', #29742, #27384, #20150 ) ;
#3202 = ORIENTED_EDGE ( 'NONE', *, *, #23759, .F. ) ;
#3203 = CARTESIAN_POINT ( 'NONE',  ( 24.34663841808528417, -12.78636765232546146, 5.096459711759587563 ) ) ;
#3204 = AXIS2_PLACEMENT_3D ( 'NONE', #4144, #29948, #20830 ) ;
#3205 = ORIENTED_EDGE ( 'NONE', *, *, #22083, .F. ) ;
#3206 = DIRECTION ( 'NONE',  ( -0.9316362575375349842, 0.3633921898465292122, -0.000000000000000000 ) ) ;
#3207 = CARTESIAN_POINT ( 'NONE',  ( -8.000000000018781421, -117.3918542544958115, 16.08262865818876008 ) ) ;
#3208 = ORIENTED_EDGE ( 'NONE', *, *, #13945, .T. ) ;
#3209 = CARTESIAN_POINT ( 'NONE',  ( -4.892971904093138313, 0.02481116134537240947, -61.82122063472499462 ) ) ;
#3210 = FACE_OUTER_BOUND ( 'NONE', #21529, .T. ) ;
#3211 = CARTESIAN_POINT ( 'NONE',  ( -26.70575606321611062, 9.025857534248860503, -0.5592437529999827461 ) ) ;
#3212 = CARTESIAN_POINT ( 'NONE',  ( 10.93704958068320643, 20.99999999999893419, -55.10811739799955689 ) ) ;
#3213 =( NAMED_UNIT ( * ) PLANE_ANGLE_UNIT ( ) SI_UNIT ( $, .RADIAN. ) );
#3214 = CARTESIAN_POINT ( 'NONE',  ( -2.017871889752692383, -3.161030873707806332, -0.6999999999999992895 ) ) ;
#3215 = EDGE_LOOP ( 'NONE', ( #18346, #21716, #4956, #11760 ) ) ;
#3216 = CARTESIAN_POINT ( 'NONE',  ( 0.9560301513573733478, -26.78297054411803302, 5.548968163149520905 ) ) ;
#3217 = CARTESIAN_POINT ( 'NONE',  ( 19.29843289230000281, 19.63498672150000246, 229.6955567279999855 ) ) ;
#3218 = VERTEX_POINT ( 'NONE', #27404 ) ;
#3219 = CARTESIAN_POINT ( 'NONE',  ( 14.77468706462038561, -31.99974765295981882, -29.54175819371382872 ) ) ;
#3220 = CARTESIAN_POINT ( 'NONE',  ( -24.86822223968197321, -13.92223202027371975, 5.680679499000030219 ) ) ;
#3221 = AXIS2_PLACEMENT_3D ( 'NONE', #1823, #27612, #30296 ) ;
#3222 = VECTOR ( 'NONE', #15689, 1000.000000000000114 ) ;
#3223 = CARTESIAN_POINT ( 'NONE',  ( -23.57322167415998138, -14.73624932338542060, 6.002747143000003227 ) ) ;
#3224 = AXIS2_PLACEMENT_3D ( 'NONE', #12743, #22356, #803 ) ;
#3225 = CARTESIAN_POINT ( 'NONE',  ( 26.84464183999999776, -3.287411896319999731E-15, 142.5624961750000068 ) ) ;
#3226 = VECTOR ( 'NONE', #17718, 1000.000000000000114 ) ;
#3227 = CARTESIAN_POINT ( 'NONE',  ( -9.689804814931735066, -24.98716964724290435, 203.0596100955893633 ) ) ;
#3228 = FACE_OUTER_BOUND ( 'NONE', #5978, .T. ) ;
#3229 = CARTESIAN_POINT ( 'NONE',  ( -24.24144457387483698, -14.48500828217274439, -0.6999999999999784173 ) ) ;
#3230 = CARTESIAN_POINT ( 'NONE',  ( -23.94309786560000219, 13.28188914049999880, 230.0000000000000000 ) ) ;
#3231 = CARTESIAN_POINT ( 'NONE',  ( 23.81866167241657806, 14.33570040768432996, 6.099998581000020792 ) ) ;
#3232 = EDGE_CURVE ( 'NONE', #12806, #10592, #10253, .T. ) ;
#3233 = CARTESIAN_POINT ( 'NONE',  ( -25.38111185550166127, -8.615767840674495304, 93.21714158837185948 ) ) ;
#3234 = CARTESIAN_POINT ( 'NONE',  ( -2.098441946322436635, -3.287561928151557122, -68.10000000002500542 ) ) ;
#3235 = COLOUR_RGB ( '', 0.72549020, 0.75294118, 0.79215686) ;
#3236 = ORIENTED_EDGE ( 'NONE', *, *, #29708, .T. ) ;
#3237 = EDGE_CURVE ( 'NONE', #24657, #12069, #7987, .T. ) ;
#3238 = CARTESIAN_POINT ( 'NONE',  ( 11.02757639490000052, -24.42656466549999905, -0.8308236885000014338 ) ) ;
#3239 = CARTESIAN_POINT ( 'NONE',  ( 9.799999999993435296, -14.12326182050966139, -36.34918934884738206 ) ) ;
#3240 = CARTESIAN_POINT ( 'NONE',  ( -26.87372837451908580, 0.8705246371642829661, -0.6999999999999992895 ) ) ;
#3241 = CARTESIAN_POINT ( 'NONE',  ( -0.9941633020186212422, 5.428540911361258381, -61.05324387862498980 ) ) ;
#3242 = AXIS2_PLACEMENT_3D ( 'NONE', #13971, #16166, #14125 ) ;
#3243 = ORIENTED_EDGE ( 'NONE', *, *, #10470, .T. ) ;
#3244 = CIRCLE ( 'NONE', #8770, 27.92857142840000151 ) ;
#3245 = ORIENTED_EDGE ( 'NONE', *, *, #10974, .T. ) ;
#3246 = CARTESIAN_POINT ( 'NONE',  ( -19.86374233096328012, -20.73196311662712077, 0.08279834900001836751 ) ) ;
#3247 = ORIENTED_EDGE ( 'NONE', *, *, #11490, .F. ) ;
#3248 = ORIENTED_EDGE ( 'NONE', *, *, #9098, .T. ) ;
#3249 = ADVANCED_FACE ( 'NONE', ( #10274 ), #19718, .F. ) ;
#3250 = DIRECTION ( 'NONE',  ( 0.000000000000000000, 0.000000000000000000, 1.000000000000000000 ) ) ;
#3251 = CARTESIAN_POINT ( 'NONE',  ( -23.62009186240247161, -12.66256056379310202, 225.7119260798266396 ) ) ;
#3252 = CARTESIAN_POINT ( 'NONE',  ( -24.08872333959828893, -11.87645233066225714, 143.2171415880000040 ) ) ;
#3253 = LINE ( 'NONE', #29532, #5771 ) ;
#3254 = CARTESIAN_POINT ( 'NONE',  ( 24.37450210455010335, -13.36961646745188759, 6.095967861000000987 ) ) ;
#3255 = AXIS2_PLACEMENT_3D ( 'NONE', #28296, #8786, #11777 ) ;
#3256 = LINE ( 'NONE', #15849, #26592 ) ;
#3257 = ORIENTED_EDGE ( 'NONE', *, *, #27456, .F. ) ;
#3258 = CARTESIAN_POINT ( 'NONE',  ( 1.806849487525330922, -4.550967181663256866, -44.10000000002499121 ) ) ;
#3259 = DIRECTION ( 'NONE',  ( -1.000000000000000000, 5.687698019341907056E-16, -6.771501495046482653E-12 ) ) ;
#3260 = CARTESIAN_POINT ( 'NONE',  ( -4.430040892179083478, 1.363067613765873931, -22.32289663399999924 ) ) ;
#3261 = CARTESIAN_POINT ( 'NONE',  ( -12.59914306489271318, -22.46391341019676702, -31.55459187839498725 ) ) ;
#3262 = CARTESIAN_POINT ( 'NONE',  ( 24.68173674080000168, -14.25001227039999918, 226.1000014189999945 ) ) ;
#3263 = AXIS2_PLACEMENT_3D ( 'NONE', #28518, #9318, #18920 ) ;
#3264 = DIRECTION ( 'NONE',  ( -5.962915006522622422E-16, -0.4383711467890810676, -0.8987940462991651502 ) ) ;
#3265 = CARTESIAN_POINT ( 'NONE',  ( -2.571638601809290936, 3.775240214263654526, -48.05391720702499470 ) ) ;
#3266 = CARTESIAN_POINT ( 'NONE',  ( -23.73992238019999945, -12.43607998449999918, 5.000000000000000000 ) ) ;
#3267 = CARTESIAN_POINT ( 'NONE',  ( 5.393907605749510559, -26.25263145716209578, 209.2056843174096628 ) ) ;
#3268 = CARTESIAN_POINT ( 'NONE',  ( -19.37594187952227642, 20.00001632898912973, 230.3398175302317838 ) ) ;
#3269 = EDGE_CURVE ( 'NONE', #6914, #5911, #27101, .T. ) ;
#3270 = DIRECTION ( 'NONE',  ( 1.000000000000000000, 0.000000000000000000, 0.000000000000000000 ) ) ;
#3271 = ADVANCED_FACE ( 'NONE', ( #535, #1130 ), #26340, .F. ) ;
#3272 = CARTESIAN_POINT ( 'NONE',  ( 6.706468900734747329, -25.94814536837671071, 21.60853380882830166 ) ) ;
#3273 = ORIENTED_EDGE ( 'NONE', *, *, #22485, .T. ) ;
#3274 = CARTESIAN_POINT ( 'NONE',  ( -4.339197174995631734, 0.6278332542688225271, -34.25783976329999092 ) ) ;
#3275 = AXIS2_PLACEMENT_3D ( 'NONE', #21118, #18744, #1300 ) ;
#3276 = ORIENTED_EDGE ( 'NONE', *, *, #29739, .F. ) ;
#3277 = DIRECTION ( 'NONE',  ( 0.000000000000000000, -0.3420201433259318913, 0.9396926207858126157 ) ) ;
#3278 = CARTESIAN_POINT ( 'NONE',  ( 0.7122403016127445419, -5.223333760075516530, -50.51468436622500491 ) ) ;
#3279 = VERTEX_POINT ( 'NONE', #15296 ) ;
#3280 = ORIENTED_EDGE ( 'NONE', *, *, #21019, .F. ) ;
#3281 = CARTESIAN_POINT ( 'NONE',  ( -13.44431541207212533, -28.18634278623086331, 240.3134495158109587 ) ) ;
#3282 = ORIENTED_EDGE ( 'NONE', *, *, #13953, .F. ) ;
#3283 = ORIENTED_EDGE ( 'NONE', *, *, #7708, .F. ) ;
#3284 = ADVANCED_FACE ( 'NONE', ( #12463 ), #24900, .F. ) ;
#3285 = CARTESIAN_POINT ( 'NONE',  ( 16.06675444876397307, -9.020011618195203695, -1.000005633855494125E-09 ) ) ;
#3286 = CARTESIAN_POINT ( 'NONE',  ( 24.22405392119105016, 13.63981656816893739, 4.239871879999995485 ) ) ;
#3287 = CARTESIAN_POINT ( 'NONE',  ( -9.999999999559999964, 21.00000000069999473, -60.10000000000000142 ) ) ;
#3288 = CARTESIAN_POINT ( 'NONE',  ( 2.073932621141414412, 4.546060023457436650, -35.70000000000000284 ) ) ;
#3289 = PLANE ( 'NONE',  #2893 ) ;
#3290 = CARTESIAN_POINT ( 'NONE',  ( -12.30731012794911194, -29.11171768734218546, -23.84543095547712355 ) ) ;
#3291 = EDGE_CURVE ( 'NONE', #20382, #16822, #4991, .T. ) ;
#3292 = CARTESIAN_POINT ( 'NONE',  ( -4.376928212848416599, 1.994761680063780407, -0.6999999999999992895 ) ) ;
#3293 = LINE ( 'NONE', #24402, #27778 ) ;
#3294 = DIRECTION ( 'NONE',  ( -1.000000000000000000, 5.665498452320000818E-16, 0.000000000000000000 ) ) ;
#3295 = CYLINDRICAL_SURFACE ( 'NONE', #11976, 1.000000000000000666 ) ;
#3296 = PRODUCT_DEFINITION ( 'UNKNOWN', '', #24408, #25091 ) ;
#3297 = CARTESIAN_POINT ( 'NONE',  ( -3.941349475653395551, -1.876729865818549392, -12.97655742010000246 ) ) ;
#3298 = CARTESIAN_POINT ( 'NONE',  ( -5.864216825196034932, 1.669623860970033347, -30.70158078970000659 ) ) ;
#3299 = CARTESIAN_POINT ( 'NONE',  ( 23.20948082139999968, -13.40000000000000036, 6.099999999630000502 ) ) ;
#3300 = CARTESIAN_POINT ( 'NONE',  ( 1.841797396446240631, -26.73663745407121795, 210.0000000000000284 ) ) ;
#3301 = DIRECTION ( 'NONE',  ( 0.000000000000000000, 0.000000000000000000, 1.000000000000000000 ) ) ;
#3302 = CARTESIAN_POINT ( 'NONE',  ( -28.04325408110000240, 1.373251542630000035E-15, 230.2432540810000319 ) ) ;
#3303 = CARTESIAN_POINT ( 'NONE',  ( 2.499950477468926291, 3.566222500441432075, -29.21106724380000230 ) ) ;
#3304 = CARTESIAN_POINT ( 'NONE',  ( 22.88229166380642354, -13.95171381546676947, 225.9137588013241498 ) ) ;
#3305 = DIRECTION ( 'NONE',  ( 0.000000000000000000, 0.000000000000000000, 1.000000000000000000 ) ) ;
#3306 = DIRECTION ( 'NONE',  ( 0.000000000000000000, -0.5000000000001900702, 0.8660254037843290176 ) ) ;
#3307 = EDGE_CURVE ( 'NONE', #18124, #11650, #30139, .T. ) ;
#3308 = EDGE_LOOP ( 'NONE', ( #8149, #14807, #2940, #19782 ) ) ;
#3309 = EDGE_CURVE ( 'NONE', #18028, #9520, #10634, .T. ) ;
#3310 = CARTESIAN_POINT ( 'NONE',  ( 23.23955039760055641, 15.25661106415676471, 5.208368893000026034 ) ) ;
#3311 = CARTESIAN_POINT ( 'NONE',  ( 2.100000000000000089, -1.998401444330000344E-15, 227.6412452697800006 ) ) ;
#3312 = ORIENTED_EDGE ( 'NONE', *, *, #9351, .T. ) ;
#3313 = CARTESIAN_POINT ( 'NONE',  ( 1.386473476218618162, 1.583312407046600701, 226.6412452697799722 ) ) ;
#3314 = DIRECTION ( 'NONE',  ( -4.428977494234582379E-12, -0.8987940462991651502, 0.4383711467890810676 ) ) ;
#3315 = ORIENTED_EDGE ( 'NONE', *, *, #7267, .T. ) ;
#3316 = CARTESIAN_POINT ( 'NONE',  ( -0.9891024240349816088, -26.78175548724776434, 4.513394068097407619 ) ) ;
#3317 = ORIENTED_EDGE ( 'NONE', *, *, #28321, .F. ) ;
#3318 = ADVANCED_FACE ( 'NONE', ( #25366 ), #8504, .F. ) ;
#3319 = ORIENTED_EDGE ( 'NONE', *, *, #14351, .T. ) ;
#3320 = ORIENTED_EDGE ( 'NONE', *, *, #26123, .F. ) ;
#3321 = CARTESIAN_POINT ( 'NONE',  ( -17.10181184887932915, 9.923569363214987504, -0.6999999999999785283 ) ) ;
#3322 = FACE_OUTER_BOUND ( 'NONE', #15210, .T. ) ;
#3323 = CARTESIAN_POINT ( 'NONE',  ( -7.999999999655324601, -17.72367216628370556, -37.31664291223312091 ) ) ;
#3324 = LINE ( 'NONE', #9445, #7067 ) ;
#3325 = CARTESIAN_POINT ( 'NONE',  ( -24.50348397099046593, 13.13223627435659857, 6.042507865999996675 ) ) ;
#3326 = CARTESIAN_POINT ( 'NONE',  ( 0.000000000000000000, 0.000000000000000000, 187.9396849849999853 ) ) ;
#3327 = CARTESIAN_POINT ( 'NONE',  ( 0.000000000000000000, 0.000000000000000000, 190.0000000000000000 ) ) ;
#3328 = CARTESIAN_POINT ( 'NONE',  ( -10.14902473071754940, -26.01926976409365722, 37.93968498539999956 ) ) ;
#3329 = EDGE_LOOP ( 'NONE', ( #23056, #9288, #9756, #21374 ) ) ;
#3330 = CARTESIAN_POINT ( 'NONE',  ( 3.112737406813101515, -4.802415649948616583, -0.1659393883000001568 ) ) ;
#3331 = CARTESIAN_POINT ( 'NONE',  ( -2.618143654921863295, 3.481518582925488658, -19.63064294430000345 ) ) ;
#3332 = CARTESIAN_POINT ( 'NONE',  ( -17.80313298963281099, -8.461754685791088804, -0.6999999999999785283 ) ) ;
#3333 = CARTESIAN_POINT ( 'NONE',  ( 24.15903335124918527, 13.75473836089376434, 5.881930534969080249 ) ) ;
#3334 = CARTESIAN_POINT ( 'NONE',  ( 3.373344672752164985, -1.082959996301563477, -88.52261276311425320 ) ) ;
#3335 = LINE ( 'NONE', #29623, #28293 ) ;
#3336 = CARTESIAN_POINT ( 'NONE',  ( 3.466821295769682159E-14, -2.890242878314739659E-13, 202.0000000000000000 ) ) ;
#3338 = CARTESIAN_POINT ( 'NONE',  ( 27.23548386990000125, -3.335274659639999982E-15, 191.6604601740000078 ) ) ;
#3337 = B_SPLINE_CURVE_WITH_KNOTS ( 'NONE', 3,
 ( #14013, #16823, #11646, #26274, #23618, #4410 ),
 .UNSPECIFIED., .F., .F.,
 ( 4, 2, 4 ),
 ( 0.000000000000000000, 0.5000000000000000000, 1.000000000000000000 ),
 .UNSPECIFIED. ) ;
#3339 = CARTESIAN_POINT ( 'NONE',  ( 26.80000000000000071, -6.394884621839999216E-14, 230.6999999999999886 ) ) ;
#3340 = DIRECTION ( 'NONE',  ( 1.000000000000000000, 0.000000000000000000, 0.000000000000000000 ) ) ;
#3341 = EDGE_CURVE ( 'NONE', #3626, #3424, #23423, .T. ) ;
#3342 = ORIENTED_EDGE ( 'NONE', *, *, #29821, .F. ) ;
#3343 = CARTESIAN_POINT ( 'NONE',  ( 1.169850847344618083, -6.301966510834352775, -58.26125695792499926 ) ) ;
#3344 = CARTESIAN_POINT ( 'NONE',  ( 23.82458380820737531, 13.44211522811278314, 0.000000000000000000 ) ) ;
#3345 = CYLINDRICAL_SURFACE ( 'NONE', #8263, 2.299999999999999822 ) ;
#3346 = EDGE_CURVE ( 'NONE', #24961, #5834, #13024, .T. ) ;
#3347 = CARTESIAN_POINT ( 'NONE',  ( -26.93580492059415121, 9.103810007694223216, 0.8585786479999857335 ) ) ;
#3348 = CARTESIAN_POINT ( 'NONE',  ( -4.626447879532794794, 0.8429120229185599333, -68.10000000002501963 ) ) ;
#3349 = EDGE_CURVE ( 'NONE', #11650, #24241, #8732, .T. ) ;
#3350 = ORIENTED_EDGE ( 'NONE', *, *, #26240, .T. ) ;
#3351 = ORIENTED_EDGE ( 'NONE', *, *, #19785, .F. ) ;
#3352 = CARTESIAN_POINT ( 'NONE',  ( 1.909260192367527864, 1.720838445342875778, -95.37004441182592984 ) ) ;
#3353 = FILL_AREA_STYLE_COLOUR ( '', #10763 ) ;
#3354 = ORIENTED_EDGE ( 'NONE', *, *, #4559, .F. ) ;
#3355 = CARTESIAN_POINT ( 'NONE',  ( 12.12499559729999810, 20.99999999999999645, -55.73512174120000395 ) ) ;
#3356 = CARTESIAN_POINT ( 'NONE',  ( -7.999999999988746779, -117.0548398251480364, 11.89578701954164686 ) ) ;
#3357 = CARTESIAN_POINT ( 'NONE',  ( 0.8372177269581546621, 4.490875019823945991, -63.42744533512499316 ) ) ;
#3358 = DIRECTION ( 'NONE',  ( -1.000000000000000000, 1.224606353819999829E-16, 0.000000000000000000 ) ) ;
#3359 = AXIS2_PLACEMENT_3D ( 'NONE', #4958, #12652, #2453 ) ;
#3360 = CARTESIAN_POINT ( 'NONE',  ( -26.79556473285982321, -0.4875557887250224209, -0.6999999999999784173 ) ) ;
#3361 = DIRECTION ( 'NONE',  ( -1.000000000000000000, 5.665498452320000818E-16, 0.000000000000000000 ) ) ;
#3362 = CIRCLE ( 'NONE', #22472, 3.000000000000001332 ) ;
#3363 = CARTESIAN_POINT ( 'NONE',  ( 0.000000000000000000, 0.000000000000000000, 227.6412452697800006 ) ) ;
#3364 = DIRECTION ( 'NONE',  ( 0.000000000000000000, -0.9396926207858125046, -0.3420201433259318358 ) ) ;
#3365 = EDGE_LOOP ( 'NONE', ( #23151, #1317, #5964, #18332 ) ) ;
#3366 = UNCERTAINTY_MEASURE_WITH_UNIT (LENGTH_MEASURE( 1.000000000000000082E-05 ), #11960, 'distance_accuracy_value', 'NONE');
#3367 = CARTESIAN_POINT ( 'NONE',  ( 0.8355090702542746772, -26.78702287552522066, 5.719315397085198427 ) ) ;
#3368 = CARTESIAN_POINT ( 'NONE',  ( 14.40197535836999876, -32.00000000000000000, -31.28675134584999640 ) ) ;
#3369 = ORIENTED_EDGE ( 'NONE', *, *, #14073, .T. ) ;
#3370 = EDGE_CURVE ( 'NONE', #13120, #12690, #2728, .T. ) ;
#3371 = CARTESIAN_POINT ( 'NONE',  ( 14.78499923084528866, -31.99972756340226709, -29.45768886394915143 ) ) ;
#3372 = CARTESIAN_POINT ( 'NONE',  ( -23.81866173682177390, -14.33570044646243247, 6.099998581000020792 ) ) ;
#3373 = CARTESIAN_POINT ( 'NONE',  ( -24.21906834513991313, -15.02342241408235068, 6.042470790000031400 ) ) ;
#3374 = CARTESIAN_POINT ( 'NONE',  ( 9.999999999961632469, -26.63382382736001119, -25.40000000000000568 ) ) ;
#3375 = CARTESIAN_POINT ( 'NONE',  ( -9.335826947264916242, -25.12147279754469764, 204.6049336590874077 ) ) ;
#3376 = PRODUCT_DEFINITION_SHAPE ( 'NONE', 'NONE',  #31126 ) ;
#3377 = CARTESIAN_POINT ( 'NONE',  ( -16.85343921422224156, -7.900182044607009679, 0.000000000000000000 ) ) ;
#3378 = CARTESIAN_POINT ( 'NONE',  ( -23.80092421055088892, -14.36517094966330710, 6.099998581000020792 ) ) ;
#3379 = CARTESIAN_POINT ( 'NONE',  ( 23.20948082139999968, -13.40000000000000036, 223.8999999999999773 ) ) ;
#3380 = ORIENTED_EDGE ( 'NONE', *, *, #19127, .T. ) ;
#3381 = DIRECTION ( 'NONE',  ( 0.000000000000000000, 0.3420201433259318913, -0.9396926207858126157 ) ) ;
#3382 = CARTESIAN_POINT ( 'NONE',  ( 28.49999999970000175, 10.47094317839999889, 222.0000000000000000 ) ) ;
#3383 =( GEOMETRIC_REPRESENTATION_CONTEXT ( 3 ) GLOBAL_UNCERTAINTY_ASSIGNED_CONTEXT ( ( #3097 ) ) GLOBAL_UNIT_ASSIGNED_CONTEXT ( ( #5843, #20791, #6619 ) ) REPRESENTATION_CONTEXT ( 'NONE', 'WORKASPACE' ) );
#3384 = TOROIDAL_SURFACE ( 'NONE', #5875, 30.50000000000000000, 3.000000000000000000 ) ;
#3385 = CARTESIAN_POINT ( 'NONE',  ( -2.373622499810734698, -26.70000180411621216, 20.00000000000000711 ) ) ;
#3386 = CARTESIAN_POINT ( 'NONE',  ( 0.2655682516138271887, -27.79918151443131791, 6.079792140000011891 ) ) ;
#3387 = EDGE_LOOP ( 'NONE', ( #2559, #25724, #23401, #3625, #5181 ) ) ;
#3388 = CARTESIAN_POINT ( 'NONE',  ( 11.16922184919999950, -24.52928866599999935, -1.544021042100003571 ) ) ;
#3389 = CARTESIAN_POINT ( 'NONE',  ( 14.67158610511051364, -22.90305194238077036, -31.80764456536135043 ) ) ;
#3390 = DIRECTION ( 'NONE',  ( 2.764840495839172918E-12, 0.9128796883888953273, -0.4082287037029531107 ) ) ;
#3391 = CARTESIAN_POINT ( 'NONE',  ( -1.078772944755383767, 5.890544393200768170, -60.25324387862499975 ) ) ;
#3392 = ORIENTED_EDGE ( 'NONE', *, *, #13273, .T. ) ;
#3393 = CARTESIAN_POINT ( 'NONE',  ( 19.32095615188756810, 19.99999286268905507, 230.3717215823191964 ) ) ;
#3394 = AXIS2_PLACEMENT_3D ( 'NONE', #25319, #29569, #8151 ) ;
#3395 = ORIENTED_EDGE ( 'NONE', *, *, #1563, .F. ) ;
#3396 = AXIS2_PLACEMENT_3D ( 'NONE', #10919, #6031, #8542 ) ;
#3397 = CARTESIAN_POINT ( 'NONE',  ( 27.08859402333790101, 0.4928875713652628443, 0.02487529600000981667 ) ) ;
#3398 = ORIENTED_EDGE ( 'NONE', *, *, #17876, .F. ) ;
#3399 = EDGE_CURVE ( 'NONE', #29694, #1748, #3493, .T. ) ;
#3400 = CARTESIAN_POINT ( 'NONE',  ( -3.378474373710000034, -11.51459555979999827, 232.0000000000000000 ) ) ;
#3401 = CARTESIAN_POINT ( 'NONE',  ( -12.29999999980791614, -28.84364015992473895, -30.79900052739454708 ) ) ;
#3402 = CARTESIAN_POINT ( 'NONE',  ( -13.99999999969999820, 20.99999999999999645, -67.09999999999999432 ) ) ;
#3403 = CIRCLE ( 'NONE', #29530, 4.987531172950001590 ) ;
#3404 = CARTESIAN_POINT ( 'NONE',  ( -24.16205483806062304, 15.15351638958479086, 8.000000000000007105 ) ) ;
#3405 = CIRCLE ( 'NONE', #5921, 3.200000000000000178 ) ;
#3406 = CARTESIAN_POINT ( 'NONE',  ( 25.44662323365202639, -12.83524168329857318, 5.310645680000003921 ) ) ;
#3407 = CARTESIAN_POINT ( 'NONE',  ( -0.2402207101440000103, -27.79943747540000132, 223.9202095490000204 ) ) ;
#3408 = EDGE_LOOP ( 'NONE', ( #7245, #6022, #18456, #25716 ) ) ;
#3409 = CARTESIAN_POINT ( 'NONE',  ( 2.609296296073386756, -3.958891508797615977, -44.10000000002499831 ) ) ;
#3410 = CARTESIAN_POINT ( 'NONE',  ( 27.76135143710000008, -3.399672736040000081E-15, 137.6614141009999912 ) ) ;
#3411 = EDGE_CURVE ( 'NONE', #27268, #15558, #21084, .T. ) ;
#3412 = CARTESIAN_POINT ( 'NONE',  ( 1.602378319964792297, -5.640493390528545703, -22.29535708920000303 ) ) ;
#3413 = CARTESIAN_POINT ( 'NONE',  ( 23.65805500388735183, -12.59178324494503265, 4.402070808934393398 ) ) ;
#3414 = DIRECTION ( 'NONE',  ( 0.000000000000000000, 0.3420201433259318913, -0.9396926207858126157 ) ) ;
#3415 = CARTESIAN_POINT ( 'NONE',  ( 1.776356839399999804E-15, -5.329070518200000398E-15, 224.6412452697800290 ) ) ;
#3416 = CARTESIAN_POINT ( 'NONE',  ( -23.79701075229709772, -14.37290030440138544, 225.9645151989870158 ) ) ;
#3417 = CARTESIAN_POINT ( 'NONE',  ( -0.5163256777700186984, 4.538631023554798638, -48.26410749632499630 ) ) ;
#3418 = AXIS2_PLACEMENT_3D ( 'NONE', #27826, #8003, #17603 ) ;
#3419 = DIRECTION ( 'NONE',  ( 0.000000000000000000, -1.000000000000000000, 0.000000000000000000 ) ) ;
#3420 = CARTESIAN_POINT ( 'NONE',  ( 0.000000000000000000, 0.000000000000000000, 90.00000000000000000 ) ) ;
#3421 = CARTESIAN_POINT ( 'NONE',  ( -10.69999999999940599, -28.79128384712763022, -25.96367195638410763 ) ) ;
#3422 = FACE_BOUND ( 'NONE', #21721, .T. ) ;
#3423 = LINE ( 'NONE', #7990, #20269 ) ;
#3424 = VERTEX_POINT ( 'NONE', #9450 ) ;
#3425 = CARTESIAN_POINT ( 'NONE',  ( 5.012492089925147276, -1.133010176909191591, -33.72127053310000377 ) ) ;
#3426 = AXIS2_PLACEMENT_3D ( 'NONE', #4392, #11934, #2646 ) ;
#3427 = ORIENTED_EDGE ( 'NONE', *, *, #16208, .F. ) ;
#3428 = ADVANCED_FACE ( 'NONE', ( #21893 ), #21580, .F. ) ;
#3429 = CARTESIAN_POINT ( 'NONE',  ( 13.62125039882827160, 21.69999999994467998, -68.61132621245515395 ) ) ;
#3430 = CARTESIAN_POINT ( 'NONE',  ( -5.206543681532186163, -1.819677770405741413, -51.20743646232500623 ) ) ;
#3431 = ORIENTED_EDGE ( 'NONE', *, *, #12893, .T. ) ;
#3432 = ORIENTED_EDGE ( 'NONE', *, *, #18671, .F. ) ;
#3433 = ORIENTED_EDGE ( 'NONE', *, *, #20089, .T. ) ;
#3434 = VERTEX_POINT ( 'NONE', #23785 ) ;
#3435 = CARTESIAN_POINT ( 'NONE',  ( -10.99999999969999998, 20.99999999999999645, -67.09999999999999432 ) ) ;
#3436 = CARTESIAN_POINT ( 'NONE',  ( -2.664535259099999568E-14, -26.80000000000000071, 115.0000000000000000 ) ) ;
#3437 = CARTESIAN_POINT ( 'NONE',  ( 5.273012595518953738, 0.3921573701267448420, -35.69999999999999574 ) ) ;
#3438 = VECTOR ( 'NONE', #1296, 1000.000000000000000 ) ;
#3439 = LINE ( 'NONE', #3763, #23515 ) ;
#3440 = CARTESIAN_POINT ( 'NONE',  ( -12.34110296562657894, -28.73347875151786113, -23.62742633845895668 ) ) ;
#3441 = CARTESIAN_POINT ( 'NONE',  ( -4.820115942865387915, 1.170356313244571345, -0.6999999999999992895 ) ) ;
#3442 = CARTESIAN_POINT ( 'NONE',  ( 3.112737406813101515, -4.802415649948616583, 0.4340606116999962127 ) ) ;
#3443 = CARTESIAN_POINT ( 'NONE',  ( 10.69999999997499884, -27.78485145323708494, -31.32209366266220485 ) ) ;
#3444 = CARTESIAN_POINT ( 'NONE',  ( -18.52981556209221381, 19.99998962372823996, -0.6359626486881121421 ) ) ;
#3445 = EDGE_CURVE ( 'NONE', #23857, #30391, #9133, .T. ) ;
#3446 = CARTESIAN_POINT ( 'NONE',  ( 1.888485499342153151, 5.773790730162923879, -11.67047964830000062 ) ) ;
#3447 = CARTESIAN_POINT ( 'NONE',  ( -5.984522419796141079, -1.167122196978044535, -30.49652066320000898 ) ) ;
#3448 = VECTOR ( 'NONE', #19022, 1000.000000000000114 ) ;
#3449 = DIRECTION ( 'NONE',  ( 0.000000000000000000, 0.3420201433259318913, -0.9396926207858126157 ) ) ;
#3450 = LINE ( 'NONE', #27072, #6193 ) ;
#3451 = CARTESIAN_POINT ( 'NONE',  ( -4.785279987099964494, -31.71089578132184883, 8.000000000000007105 ) ) ;
#3452 = CARTESIAN_POINT ( 'NONE',  ( 9.499999999662559702, -18.29892258314324494, -35.53590567821694890 ) ) ;
#3453 = CARTESIAN_POINT ( 'NONE',  ( 2.315582734148106780, 3.377836756897303783, -35.21970670790000923 ) ) ;
#3454 = CARTESIAN_POINT ( 'NONE',  ( 20.30405755279999980, 20.00000000000000000, 226.9999998930000231 ) ) ;
#3455 = DIRECTION ( 'NONE',  ( -0.000000000000000000, 1.000000000000000000, -2.257145581549999994E-12 ) ) ;
#3456 = CARTESIAN_POINT ( 'NONE',  ( 9.414213562409999625, -15.31419272936388687, -74.45223986426802298 ) ) ;
#3457 = VERTEX_POINT ( 'NONE', #14497 ) ;
#3458 = ORIENTED_EDGE ( 'NONE', *, *, #18856, .T. ) ;
#3459 = EDGE_CURVE ( 'NONE', #4259, #25869, #27510, .T. ) ;
#3460 = ADVANCED_FACE ( 'NONE', ( #7400 ), #19305, .F. ) ;
#3461 = CARTESIAN_POINT ( 'NONE',  ( -7.999999999728557576, -25.41682687375232064, -25.82167197182654661 ) ) ;
#3462 = CARTESIAN_POINT ( 'NONE',  ( -4.000000000000000000, -31.83942647549183746, -80.46693306215520636 ) ) ;
#3463 = ORIENTED_EDGE ( 'NONE', *, *, #18343, .T. ) ;
#3464 = CARTESIAN_POINT ( 'NONE',  ( -11.00000000000000000, 27.10555629988041204, -61.14106941751904856 ) ) ;
#3465 = FACE_OUTER_BOUND ( 'NONE', #10035, .T. ) ;
#3466 = ORIENTED_EDGE ( 'NONE', *, *, #9897, .T. ) ;
#3467 = CARTESIAN_POINT ( 'NONE',  ( -9.590600648852301902, -25.77356060526425097, 25.39622571667640472 ) ) ;
#3468 = ORIENTED_EDGE ( 'NONE', *, *, #19054, .T. ) ;
#3469 = ORIENTED_EDGE ( 'NONE', *, *, #6228, .T. ) ;
#3470 = EDGE_CURVE ( 'NONE', #29399, #17667, #20609, .T. ) ;
#3471 = AXIS2_PLACEMENT_3D ( 'NONE', #22262, #26521, #24015 ) ;
#3472 = ORIENTED_EDGE ( 'NONE', *, *, #15387, .T. ) ;
#3473 = CARTESIAN_POINT ( 'NONE',  ( 28.49999999979999998, 4.812685681769999668, 229.0000000000000000 ) ) ;
#3474 = AXIS2_PLACEMENT_3D ( 'NONE', #27872, #6153, #4112 ) ;
#3475 = CARTESIAN_POINT ( 'NONE',  ( -17.43796590508231503, -30.34944427540625611, -32.23970959347593634 ) ) ;
#3476 = DIRECTION ( 'NONE',  ( -0.5000000000001899592, 0.8660254037843289066, 0.000000000000000000 ) ) ;
#3477 = ORIENTED_EDGE ( 'NONE', *, *, #3647, .T. ) ;
#3478 = PRESENTATION_STYLE_ASSIGNMENT (( #17793 ) ) ;
#3479 = B_SPLINE_CURVE_WITH_KNOTS ( 'NONE', 5,
 ( #19332, #24516, #14763, #12696, #7663, #16960, #19943, #22153, #21695 ),
 .UNSPECIFIED., .F., .F.,
 ( 6, 3, 6 ),
 ( 0.000000000000000000, 53.95537973340000093, 92.42745556099998794 ),
 .UNSPECIFIED. ) ;
#3480 = CARTESIAN_POINT ( 'NONE',  ( -28.49528339128749366, -0.5184828350247786544, 8.000000000000007105 ) ) ;
#3481 = EDGE_CURVE ( 'NONE', #2258, #24119, #10233, .T. ) ;
#3482 = DIRECTION ( 'NONE',  ( 0.000000000000000000, 0.000000000000000000, -1.000000000000000000 ) ) ;
#3483 = CARTESIAN_POINT ( 'NONE',  ( 26.84464185210000053, -3.287411897800000213E-15, 187.4375040470000044 ) ) ;
#3484 = ORIENTED_EDGE ( 'NONE', *, *, #21630, .T. ) ;
#3485 = CARTESIAN_POINT ( 'NONE',  ( -1.392415278799822298, -4.107851135794777342, -1.075630512700001651 ) ) ;
#3486 = CARTESIAN_POINT ( 'NONE',  ( -6.228182343209494043, 0.8662545139425728014, -19.25159460730001371 ) ) ;
#3487 = CARTESIAN_POINT ( 'NONE',  ( -17.04621913067799710, -27.00000000059169736, -22.62649730796000114 ) ) ;
#3488 = CARTESIAN_POINT ( 'NONE',  ( 10.69999999999999929, -24.87867965640000278, -26.27867965640000136 ) ) ;
#3489 = CARTESIAN_POINT ( 'NONE',  ( 24.91921101730000032, -13.83103916679999834, 223.9972514410000031 ) ) ;
#3490 = CARTESIAN_POINT ( 'NONE',  ( -18.94276560960000211, 21.23709850699999890, 229.4982322489999831 ) ) ;
#3491 = CARTESIAN_POINT ( 'NONE',  ( -23.24663841809999809, -14.69162354060000020, 225.0000000000000000 ) ) ;
#3492 = EDGE_CURVE ( 'NONE', #11151, #13582, #23142, .T. ) ;
#3493 = B_SPLINE_CURVE_WITH_KNOTS ( 'NONE', 3,
 ( #6468, #14181, #18736, #17000, #14346, #12276 ),
 .UNSPECIFIED., .F., .F.,
 ( 4, 2, 4 ),
 ( 0.000000000000000000, 0.5000000000000000000, 1.000000000000000000 ),
 .UNSPECIFIED. ) ;
#3494 = VECTOR ( 'NONE', #22040, 1000.000000000000114 ) ;
#3495 = B_SPLINE_CURVE_WITH_KNOTS ( 'NONE', 3,
 ( #19220, #21591, #2691, #7107, #26304, #28969 ),
 .UNSPECIFIED., .F., .F.,
 ( 4, 2, 4 ),
 ( 0.000000000000000000, 0.5000000000000000000, 1.000000000000000000 ),
 .UNSPECIFIED. ) ;
#3496 = CARTESIAN_POINT ( 'NONE',  ( 10.00000000000000000, 20.99999999999999645, -62.10000000019999788 ) ) ;
#3497 = CARTESIAN_POINT ( 'NONE',  ( -15.84710441079999832, -21.98318857509999802, 230.6999999999999886 ) ) ;
#3498 = CARTESIAN_POINT ( 'NONE',  ( 3.466622106789775337, -2.539914255570844936, -39.57817603794315886 ) ) ;
#3499 = ORIENTED_EDGE ( 'NONE', *, *, #19706, .F. ) ;
#3500 = CARTESIAN_POINT ( 'NONE',  ( -5.325262776967106149, 2.643762325382013945, -56.31877225282499211 ) ) ;
#3501 = FACE_OUTER_BOUND ( 'NONE', #30433, .T. ) ;
#3502 = CARTESIAN_POINT ( 'NONE',  ( -5.990533020055879732, -1.129328118392731950, -16.09949426530000238 ) ) ;
#3503 = ORIENTED_EDGE ( 'NONE', *, *, #17876, .T. ) ;
#3504 = CARTESIAN_POINT ( 'NONE',  ( -26.66783967069105898, -7.507193849635574345, -0.6999999999999784173 ) ) ;
#3505 = CARTESIAN_POINT ( 'NONE',  ( -4.251069959271740473, 0.9221155341078968171, -68.10000000002500542 ) ) ;
#3506 = ORIENTED_EDGE ( 'NONE', *, *, #17090, .T. ) ;
#3507 = VERTEX_POINT ( 'NONE', #2991 ) ;
#3508 = EDGE_LOOP ( 'NONE', ( #29210, #24154, #17679, #13545 ) ) ;
#3509 = CARTESIAN_POINT ( 'NONE',  ( 2.899787796512155680, -2.016313622456245014, -96.83838116384302452 ) ) ;
#3510 = ORIENTED_EDGE ( 'NONE', *, *, #26633, .F. ) ;
#3511 = DIRECTION ( 'NONE',  ( 0.3633921898465292122, 0.9316362575375348731, -6.938893903907226800E-15 ) ) ;
#3512 = CARTESIAN_POINT ( 'NONE',  ( 3.552713678799999608E-15, -3.552713678799999608E-15, 186.7828584120000244 ) ) ;
#3513 = CARTESIAN_POINT ( 'NONE',  ( -5.941465883516308999, 0.03012783874251079297, -62.57122063482501062 ) ) ;
#3514 = CARTESIAN_POINT ( 'NONE',  ( 1.199983934731101209, -28.47518316922301196, 5.888828386639105794 ) ) ;
#3515 = AXIS2_PLACEMENT_3D ( 'NONE', #22889, #11551, #13433 ) ;
#3516 = CARTESIAN_POINT ( 'NONE',  ( -27.61404081990094994, 9.332834367751024374, 1.000000000000000888 ) ) ;
#3517 = EDGE_CURVE ( 'NONE', #11838, #3686, #5653, .T. ) ;
#3518 = DIRECTION ( 'NONE',  ( 0.000000000000000000, 0.000000000000000000, 1.000000000000000000 ) ) ;
#3519 = FILL_AREA_STYLE_COLOUR ( '', #8895 ) ;
#3520 = DIRECTION ( 'NONE',  ( 0.7730139489027949562, -0.6343890248118320141, 0.000000000000000000 ) ) ;
#3521 = ORIENTED_EDGE ( 'NONE', *, *, #29385, .F. ) ;
#3522 = EDGE_CURVE ( 'NONE', #1475, #1865, #13243, .T. ) ;
#3524 = CARTESIAN_POINT ( 'NONE',  ( -5.003376521275985311, 3.147367150682292447, -9.445475902800000156 ) ) ;
#3523 = SHAPE_REPRESENTATION ( 'Rear Frame Plate', ( #17722 ), #16292 ) ;
#3525 = DIRECTION ( 'NONE',  ( 1.224606353819999829E-16, 1.000000000000000000, 0.000000000000000000 ) ) ;
#3526 = PRODUCT ( 'Pivot Pin', 'Pivot Pin', '', ( #20272 ) ) ;
#3527 = ADVANCED_FACE ( 'NONE', ( #10081 ), #4040, .T. ) ;
#3528 = CARTESIAN_POINT ( 'NONE',  ( 7.000000000108768994, -60.06002009431549737, -1.894810482370685278 ) ) ;
#3529 = VERTEX_POINT ( 'NONE', #29416 ) ;
#3530 = CARTESIAN_POINT ( 'NONE',  ( -10.69999999999999929, -30.00000000000000000, -28.40000000000000213 ) ) ;
#3531 = DIRECTION ( 'NONE',  ( 0.3633921898465272138, -0.9316362575375356503, 2.312964634635741872E-15 ) ) ;
#3532 = CARTESIAN_POINT ( 'NONE',  ( 5.361384718760000112, -31.61859215249999977, 229.0000000000000000 ) ) ;
#3533 = FACE_OUTER_BOUND ( 'NONE', #23808, .T. ) ;
#3534 = CARTESIAN_POINT ( 'NONE',  ( -8.964607010186835367, -25.25702356185616537, 205.5800510650676927 ) ) ;
#3535 = CARTESIAN_POINT ( 'NONE',  ( 6.136659917679837761, 0.6935318534637759935, -55.01771407622499765 ) ) ;
#3536 = CARTESIAN_POINT ( 'NONE',  ( -10.93755790490000024, -24.69832375660000423, -1.748184584100004324 ) ) ;
#3537 = CYLINDRICAL_SURFACE ( 'NONE', #29338, 1.100000000000002309 ) ;
#3538 = ORIENTED_EDGE ( 'NONE', *, *, #15143, .F. ) ;
#3539 = CARTESIAN_POINT ( 'NONE',  ( -10.69999999997431672, -28.51136270451570454, -31.02111648946564415 ) ) ;
#3540 = CARTESIAN_POINT ( 'NONE',  ( 25.26809617039999978, 12.77001320649999982, 222.0000000000000000 ) ) ;
#3541 = B_SPLINE_CURVE_WITH_KNOTS ( 'NONE', 5,
 ( #1998, #28258, #1681, #13790, #21035, #11433, #30782, #9210, #18815, #9685, #2309, #3176 ),
 .UNSPECIFIED., .F., .F.,
 ( 6, 3, 3, 6 ),
 ( 1.118801870760000039, 1.395630273020000089, 2.093431498840000238, 2.237519762620000296 ),
 .UNSPECIFIED. ) ;
#3543 = CARTESIAN_POINT ( 'NONE',  ( -27.23548387180000319, 3.335274659879999868E-15, 88.33953982590000464 ) ) ;
#3542 =( REPRESENTATION_RELATIONSHIP ('NONE','NONE', #2712, #527 ) REPRESENTATION_RELATIONSHIP_WITH_TRANSFORMATION ( #10030 )SHAPE_REPRESENTATION_RELATIONSHIP( ) );
#3544 = CARTESIAN_POINT ( 'NONE',  ( 0.6518654482653677418, -3.960075354149236393, -68.10000000002500542 ) ) ;
#3545 = CARTESIAN_POINT ( 'NONE',  ( 11.32877539780000120, -24.28840541759999994, -0.7339858088999950958 ) ) ;
#3546 = AXIS2_PLACEMENT_3D ( 'NONE', #7557, #4738, #19370 ) ;
#3547 =( NAMED_UNIT ( * ) PLANE_ANGLE_UNIT ( ) SI_UNIT ( $, .RADIAN. ) );
#3548 = CARTESIAN_POINT ( 'NONE',  ( -2.098441946322436635, -3.287561928151557122, -68.10000000002500542 ) ) ;
#3549 = CARTESIAN_POINT ( 'NONE',  ( 3.565893352360864466, 0.9842897974745647982, -41.29704520336932916 ) ) ;
#3550 = B_SPLINE_CURVE_WITH_KNOTS ( 'NONE', 5,
 ( #29442, #22375, #22215, #820, #14831, #10410, #17480, #17778, #27391, #5830, #21918, #19549 ),
 .UNSPECIFIED., .F., .F.,
 ( 6, 3, 3, 6 ),
 ( 1.117931991990000151, 1.394586747660000015, 2.091870620439999939, 2.235835859519999858 ),
 .UNSPECIFIED. ) ;
#3551 = CARTESIAN_POINT ( 'NONE',  ( -5.475468559288758641, 0.02776487098956707464, -63.37122063482500067 ) ) ;
#3552 = ORIENTED_EDGE ( 'NONE', *, *, #643, .T. ) ;
#3553 = CARTESIAN_POINT ( 'NONE',  ( 19.73226377590565050, 20.00031052610880877, 230.1021219667221089 ) ) ;
#3554 = ORIENTED_EDGE ( 'NONE', *, *, #26182, .T. ) ;
#3555 = B_SPLINE_CURVE_WITH_KNOTS ( 'NONE', 5,
 ( #5361, #24248, #5053, #17157, #4481, #7713, #28970, #23381, #21738, #26764, #21007, #26925 ),
 .UNSPECIFIED., .F., .F.,
 ( 6, 3, 3, 6 ),
 ( 3.339306056609999906, 4.810258468679999844, 6.613963843700000567, 6.678484287649999018 ),
 .UNSPECIFIED. ) ;
#3556 = CARTESIAN_POINT ( 'NONE',  ( 8.700000000294906499, -15.59658250094199161, -40.60120179151234510 ) ) ;
#3557 = ORIENTED_EDGE ( 'NONE', *, *, #7133, .T. ) ;
#3558 = CARTESIAN_POINT ( 'NONE',  ( -3.790556161138087354, 0.9809627197493214767, -41.29542247913801845 ) ) ;
#3559 = CARTESIAN_POINT ( 'NONE',  ( -23.73992238018677980, -12.43607998452291774, 225.0964353478398436 ) ) ;
#3560 = CARTESIAN_POINT ( 'NONE',  ( -3.483928249568471358, -0.9656592618177964882, 230.7696496080388329 ) ) ;
#3561 = CARTESIAN_POINT ( 'NONE',  ( -26.80000000069999899, 3.281945028329999726E-15, 65.00000000000000000 ) ) ;
#3562 = CARTESIAN_POINT ( 'NONE',  ( -8.699999999715885224, -26.99999999997790923, -28.40000000002690683 ) ) ;
#3563 = EDGE_CURVE ( 'NONE', #8967, #11921, #26751, .T. ) ;
#3564 = CARTESIAN_POINT ( 'NONE',  ( 10.69999999999999929, -27.00000000000000000, -28.40000000000000213 ) ) ;
#3565 = ORIENTED_EDGE ( 'NONE', *, *, #24311, .T. ) ;
#3566 = CARTESIAN_POINT ( 'NONE',  ( -28.68577477009351995, 9.950727454193893706, 8.000000000000007105 ) ) ;
#3567 = CARTESIAN_POINT ( 'NONE',  ( 28.45771199730000234, -1.659298224529999796E-14, 229.4982322489999831 ) ) ;
#3568 = DIRECTION ( 'NONE',  ( 0.000000000000000000, 0.000000000000000000, 1.000000000000000000 ) ) ;
#3569 = CARTESIAN_POINT ( 'NONE',  ( 0.1332961122732720383, -6.531058726825651028, -24.41888333260000365 ) ) ;
#3570 = DIRECTION ( 'NONE',  ( 0.7071067811865467956, 0.6644630243886068266, 0.2418447626481644297 ) ) ;
#3571 = DIRECTION ( 'NONE',  ( 0.6087614290090099800, -0.7933533402910131205, 4.134191582186808379E-12 ) ) ;
#3572 = CARTESIAN_POINT ( 'NONE',  ( -27.50000000000000000, 3.367667473009999970E-15, 186.7190980919999959 ) ) ;
#3573 = CARTESIAN_POINT ( 'NONE',  ( 0.5500237538654858538, -27.79507126796909944, 224.0359736129612145 ) ) ;
#3574 = CARTESIAN_POINT ( 'NONE',  ( 4.432674687120906398, 4.607520344841867121, -48.21426496242499837 ) ) ;
#3575 = CARTESIAN_POINT ( 'NONE',  ( -17.63560569383767529, 11.76631802938718430, -1.400000000000001910 ) ) ;
#3576 = CARTESIAN_POINT ( 'NONE',  ( 9.738910687886868089, -24.96785170200598358, 202.0000000000000000 ) ) ;
#3577 = CARTESIAN_POINT ( 'NONE',  ( -20.04376857943106316, 19.99997512704260316, 229.7707830521836172 ) ) ;
#3578 = CARTESIAN_POINT ( 'NONE',  ( -26.11394584979203870, -6.088596733047853427, 43.21714158835001030 ) ) ;
#3579 = CARTESIAN_POINT ( 'NONE',  ( 18.24300304086109747, -9.268384253839881737, -4.336808689942017243E-16 ) ) ;
#3580 = VERTEX_POINT ( 'NONE', #5499 ) ;
#3581 = CARTESIAN_POINT ( 'NONE',  ( -6.074876045044606876, 0.8789665559579967757, -34.85783976329999234 ) ) ;
#3582 = VERTEX_POINT ( 'NONE', #24700 ) ;
#3583 = FACE_OUTER_BOUND ( 'NONE', #5563, .T. ) ;
#3584 = CARTESIAN_POINT ( 'NONE',  ( 4.669144396295984656, -2.892150817486062397, -50.13324460762500223 ) ) ;
#3585 = ORIENTED_EDGE ( 'NONE', *, *, #14607, .F. ) ;
#3586 = EDGE_CURVE ( 'NONE', #30810, #24995, #3137, .T. ) ;
#3587 = ITEM_DEFINED_TRANSFORMATION ( 'NONE', 'NONE', #27407,  #17722 ) ;
#3588 = AXIS2_PLACEMENT_3D ( 'NONE', #22123, #15345, #17083 ) ;
#3589 = VERTEX_POINT ( 'NONE', #10850 ) ;
#3590 = ORIENTED_EDGE ( 'NONE', *, *, #805, .F. ) ;
#3591 = CARTESIAN_POINT ( 'NONE',  ( -17.70061747236281491, 10.30810785442435495, -0.6999999999999783062 ) ) ;
#3592 = CYLINDRICAL_SURFACE ( 'NONE', #25544, 3.000000000000003997 ) ;
#3593 = DIRECTION ( 'NONE',  ( 1.000000000000000000, -6.668066630619518976E-24, -2.257150022442225012E-12 ) ) ;
#3594 = CARTESIAN_POINT ( 'NONE',  ( -14.89999999913999851, -32.00000000000000000, -25.51324865424999899 ) ) ;
#3595 = CARTESIAN_POINT ( 'NONE',  ( -0.9007122707567293274, -27.48548889902986048, 4.367019785660003706 ) ) ;
#3596 = CARTESIAN_POINT ( 'NONE',  ( -3.745457574878203300, 2.149009913884074141, -0.6999999999999994005 ) ) ;
#3597 = CARTESIAN_POINT ( 'NONE',  ( 4.797053106898050423, -0.1656196055093784036, -1.747909721200001210 ) ) ;
#3598 = DIRECTION ( 'NONE',  ( -0.3633921898465273803, 0.9316362575375355393, 0.000000000000000000 ) ) ;
#3599 = CARTESIAN_POINT ( 'NONE',  ( 25.40918998824096420, -12.90916337733692920, 5.498574324082793119 ) ) ;
#3600 = ORIENTED_EDGE ( 'NONE', *, *, #18462, .F. ) ;
#3601 = CARTESIAN_POINT ( 'NONE',  ( -4.335484423225056005, -2.064402852395420318, -13.91405742009999358 ) ) ;
#3602 = CARTESIAN_POINT ( 'NONE',  ( -4.188726303739433554, 1.192588472141202560, -31.30158078970000801 ) ) ;
#3603 = LINE ( 'NONE', #29582, #30262 ) ;
#3604 = FACE_OUTER_BOUND ( 'NONE', #7873, .T. ) ;
#3605 = CARTESIAN_POINT ( 'NONE',  ( 28.49528339128749366, 0.5184828350247823181, 8.000000000000007105 ) ) ;
#3606 = LINE ( 'NONE', #29737, #24715 ) ;
#3607 = CARTESIAN_POINT ( 'NONE',  ( 0.2309929099465271585, 4.358477053493584386, -22.94418644579999977 ) ) ;
#3608 = AXIS2_PLACEMENT_3D ( 'NONE', #22628, #770, #24676 ) ;
#3610 = CARTESIAN_POINT ( 'NONE',  ( 21.73669719418043300, 17.54549339080899273, -0.5592437529999827461 ) ) ;
#3609 = B_SPLINE_CURVE_WITH_KNOTS ( 'NONE', 3,
 ( #17171, #14827, #17477, #12446, #27084, #22065 ),
 .UNSPECIFIED., .F., .F.,
 ( 4, 2, 4 ),
 ( 0.000000000000000000, 0.5000000000000000000, 1.000000000000000000 ),
 .UNSPECIFIED. ) ;
#3611 = DIRECTION ( 'NONE',  ( -1.000000000000000000, 0.000000000000000000, 0.000000000000000000 ) ) ;
#3612 = CARTESIAN_POINT ( 'NONE',  ( 3.861721477338983632, 0.2146938849234697466, -40.92168819634601107 ) ) ;
#3613 = EDGE_LOOP ( 'NONE', ( #6859, #10343, #6323, #8305 ) ) ;
#3614 = ORIENTED_EDGE ( 'NONE', *, *, #26586, .F. ) ;
#3615 = EDGE_CURVE ( 'NONE', #15176, #14782, #18064, .T. ) ;
#3616 = CARTESIAN_POINT ( 'NONE',  ( 24.06750537016302971, 15.26514225575640360, 5.901296968999991677 ) ) ;
#3617 = CARTESIAN_POINT ( 'NONE',  ( 2.990544846595957651, 1.820224383385054212, 230.8378734041668565 ) ) ;
#3618 = ORIENTED_EDGE ( 'NONE', *, *, #30018, .T. ) ;
#3619 = CARTESIAN_POINT ( 'NONE',  ( 0.3874847876441021577, -3.500000000000000888, 227.6554536018038561 ) ) ;
#3620 = CARTESIAN_POINT ( 'NONE',  ( -10.46446609379999870, 20.99999999999999645, -54.63553390589999736 ) ) ;
#3621 = ORIENTED_EDGE ( 'NONE', *, *, #7436, .T. ) ;
#3622 = LINE ( 'NONE', #12921, #23058 ) ;
#3623 = VERTEX_POINT ( 'NONE', #1570 ) ;
#3624 = ADVANCED_FACE ( 'NONE', ( #6115 ), #16104, .F. ) ;
#3625 = ORIENTED_EDGE ( 'NONE', *, *, #23068, .T. ) ;
#3626 = VERTEX_POINT ( 'NONE', #8787 ) ;
#3627 = CARTESIAN_POINT ( 'NONE',  ( 24.61735023129999789, 13.67123892250000061, 230.5592437530000041 ) ) ;
#3628 = VECTOR ( 'NONE', #19062, 1000.000000000000114 ) ;
#3629 = FACE_OUTER_BOUND ( 'NONE', #2710, .T. ) ;
#3630 = CARTESIAN_POINT ( 'NONE',  ( -3.015466128627334985, 1.304460199876133819, -68.40354486441854931 ) ) ;
#3631 = ORIENTED_EDGE ( 'NONE', *, *, #21369, .T. ) ;
#3632 = FILL_AREA_STYLE ('',( #20473 ) ) ;
#3633 = CARTESIAN_POINT ( 'NONE',  ( -5.665412366707123226, 6.378525563588088865, -40.59018395548486069 ) ) ;
#3634 = PLANE ( 'NONE',  #23108 ) ;
#3635 = CARTESIAN_POINT ( 'NONE',  ( -8.699999999642283655, -16.96959321760381556, -37.81493174590716677 ) ) ;
#3636 = CARTESIAN_POINT ( 'NONE',  ( -12.41421356240000051, 25.87105682045942245, -59.46203493729375822 ) ) ;
#3637 = EDGE_CURVE ( 'NONE', #10144, #15285, #6113, .T. ) ;
#3638 = ADVANCED_FACE ( 'NONE', ( #13356 ), #4077, .F. ) ;
#3639 = CARTESIAN_POINT ( 'NONE',  ( 3.436082050571401147, -2.282315740991585962, -0.8962547302000020144 ) ) ;
#3640 = CARTESIAN_POINT ( 'NONE',  ( 2.949882002856666130, 3.605460750137340131, -19.75622222230000702 ) ) ;
#3641 = CARTESIAN_POINT ( 'NONE',  ( 25.41516571979999739, -14.56554164990000011, 228.9999999990000106 ) ) ;
#3642 = CARTESIAN_POINT ( 'NONE',  ( 24.10026512741646698, 13.85771999287294598, 5.960845917926949511 ) ) ;
#3643 = CARTESIAN_POINT ( 'NONE',  ( 2.983143093411794400, -3.582908191650746588, -95.30338155897700858 ) ) ;
#3644 = CARTESIAN_POINT ( 'NONE',  ( -26.80000000000000071, 4.518892556970000030, 230.6999999999999886 ) ) ;
#3645 = CARTESIAN_POINT ( 'NONE',  ( -28.57800709146147256, 4.027926662255243428, 1.000000000000000888 ) ) ;
#3646 = CARTESIAN_POINT ( 'NONE',  ( 10.69999999996564810, -42.68493023230600159, -27.18108142580972952 ) ) ;
#3647 = EDGE_CURVE ( 'NONE', #11688, #27946, #24520, .T. ) ;
#3648 = LINE ( 'NONE', #3496, #5158 ) ;
#3649 = CARTESIAN_POINT ( 'NONE',  ( 4.440892098500000496E-16, -0.1455297029551360921, -71.05965357398815740 ) ) ;
#3650 = CARTESIAN_POINT ( 'NONE',  ( 4.706785070836938090, -9.032362236610094186, -33.07379175659606574 ) ) ;
#3651 = VERTEX_POINT ( 'NONE', #30193 ) ;
#3652 = CARTESIAN_POINT ( 'NONE',  ( -3.855177830964256813, -4.571422008809257420, -58.69407541852499577 ) ) ;
#3653 = AXIS2_PLACEMENT_3D ( 'NONE', #28552, #7308, #19108 ) ;
#3654 = CARTESIAN_POINT ( 'NONE',  ( -8.699999999662093586, -15.94902145834643115, -35.53273252493492862 ) ) ;
#3655 = ORIENTED_EDGE ( 'NONE', *, *, #20172, .T. ) ;
#3656 = CARTESIAN_POINT ( 'NONE',  ( -0.8919388126321509125, 6.008950160842678301, -10.86772091660000150 ) ) ;
#3657 = ORIENTED_EDGE ( 'NONE', *, *, #18560, .F. ) ;
#3658 = CARTESIAN_POINT ( 'NONE',  ( -25.11765555659999904, -13.46780168200000105, 225.6808342349999918 ) ) ;
#3659 = EDGE_CURVE ( 'NONE', #15429, #30761, #24134, .T. ) ;
#3660 = CARTESIAN_POINT ( 'NONE',  ( 26.62724484483131349, -3.508068424019962883, 186.7828584120000244 ) ) ;
#3661 = ORIENTED_EDGE ( 'NONE', *, *, #12031, .F. ) ;
#3662 = CARTESIAN_POINT ( 'NONE',  ( -16.04158851053540857, -9.763538383445707680, -0.6999999999999784173 ) ) ;
#3663 = ORIENTED_EDGE ( 'NONE', *, *, #21563, .F. ) ;
#3664 = ORIENTED_EDGE ( 'NONE', *, *, #22554, .F. ) ;
#3665 = CARTESIAN_POINT ( 'NONE',  ( -26.62724484483131704, -3.508068424019966880, 186.7828584128332920 ) ) ;
#3666 = VERTEX_POINT ( 'NONE', #18221 ) ;
#3667 = DIRECTION ( 'NONE',  ( 0.000000000000000000, 0.000000000000000000, 1.000000000000000000 ) ) ;
#3668 = CARTESIAN_POINT ( 'NONE',  ( 0.5496705564632800023, -2.045342621171242659, 226.6412452697799438 ) ) ;
#3669 = CARTESIAN_POINT ( 'NONE',  ( -5.475468559288758641, 0.02776487098956707464, -61.77122063472499036 ) ) ;
#3670 = ADVANCED_FACE ( 'NONE', ( #25799 ), #27829, .T. ) ;
#3671 = VECTOR ( 'NONE', #21163, 1000.000000000000114 ) ;
#3672 = CARTESIAN_POINT ( 'NONE',  ( -27.09307779339999911, 1.442401753589999799E-12, 229.9751247039999953 ) ) ;
#3673 = B_SPLINE_CURVE_WITH_KNOTS ( 'NONE', 5,
 ( #12336, #12173, #17200, #19420, #26807, #24292, #21783, #552, #2740, #14863, #26352, #23997, #3039, #29010, #14552, #24454, #9662, #7607, #7310, #84, #2436, #19732, #12632, #19265 ),
 .UNSPECIFIED., .F., .F.,
 ( 6, 3, 3, 3, 3, 3, 3, 6 ),
 ( 0.000000000000000000, 11.88805610990000083, 23.77581053719999815, 35.66412908880000288, 47.55143447889999919, 59.43964105460000269, 71.32790799789999880, 81.23067401939999854 ),
 .UNSPECIFIED. ) ;
#3674 = CARTESIAN_POINT ( 'NONE',  ( 6.000000000000000000, -23.16799891216055940, -79.43914708545641190 ) ) ;
#3675 = DIRECTION ( 'NONE',  ( -3.103340825716225161E-16, 1.008336558399225884E-16, 1.000000000000000000 ) ) ;
#3676 = CONICAL_SURFACE ( 'NONE', #18756, 0.9999999999991029398, 0.7853981633970000820 ) ;
#3677 = EDGE_CURVE ( 'NONE', #15540, #27013, #17374, .T. ) ;
#3678 = CARTESIAN_POINT ( 'NONE',  ( -23.62133197417733754, -12.66014020671418372, 5.703642737970564092 ) ) ;
#3679 = DIRECTION ( 'NONE',  ( 0.000000000000000000, 0.000000000000000000, 1.000000000000000000 ) ) ;
#3680 = EDGE_LOOP ( 'NONE', ( #20350, #14514, #29906, #25706 ) ) ;
#3681 = PRODUCT_DEFINITION_CONTEXT ( 'detailed design', #12597, 'design' ) ;
#3682 = CARTESIAN_POINT ( 'NONE',  ( -0.8919388126321509125, 6.008950160842678301, -10.26772091660000541 ) ) ;
#3683 = CARTESIAN_POINT ( 'NONE',  ( 18.95046173579999760, -18.95046173579999760, 186.7828584120000244 ) ) ;
#3684 = EDGE_CURVE ( 'NONE', #14251, #3529, #27152, .T. ) ;
#3685 = LINE ( 'NONE', #8391, #465 ) ;
#3686 = VERTEX_POINT ( 'NONE', #30519 ) ;
#3687 = CARTESIAN_POINT ( 'NONE',  ( 24.46818569879999927, -13.19686604630000026, 224.2398747240000034 ) ) ;
#3688 = CARTESIAN_POINT ( 'NONE',  ( -23.16094352436829240, -13.48406906362809998, 3.900000000003496670 ) ) ;
#3689 = FACE_OUTER_BOUND ( 'NONE', #23976, .T. ) ;
#3690 = CARTESIAN_POINT ( 'NONE',  ( 21.71205242481305930, 17.52560354592457870, 0.2686741030000217023 ) ) ;
#3691 = DIRECTION ( 'NONE',  ( 0.000000000000000000, 0.000000000000000000, 1.000000000000000000 ) ) ;
#3692 = CARTESIAN_POINT ( 'NONE',  ( -0.9881560945370695404, 5.823346091562972227, -51.25792092402499378 ) ) ;
#3693 = CARTESIAN_POINT ( 'NONE',  ( -11.32877539260000077, -24.28840542069999842, -0.7339858089999984347 ) ) ;
#3694 = CARTESIAN_POINT ( 'NONE',  ( 23.13685276771313326, -13.52579547908016622, 223.9000000000000057 ) ) ;
#3695 = VERTEX_POINT ( 'NONE', #4233 ) ;
#3696 = CARTESIAN_POINT ( 'NONE',  ( 27.79999999990000248, 4.333901782529999025, 229.0000000000000000 ) ) ;
#3697 = VECTOR ( 'NONE', #8029, 1000.000000000000000 ) ;
#3698 = VECTOR ( 'NONE', #19691, 1000.000000000000114 ) ;
#3699 = CARTESIAN_POINT ( 'NONE',  ( 2.723675539006792157, -3.828301447610997332, -68.10000000002499121 ) ) ;
#3700 = ADVANCED_FACE ( 'NONE', ( #22803 ), #22650, .F. ) ;
#3701 = B_SPLINE_CURVE_WITH_KNOTS ( 'NONE', 3,
 ( #30163, #10975, #20566, #23100, #8595, #1380, #11131, #11290, #18367, #18034, #20729, #1222, #20894, #13645, #8434, #28270, #11445, #30000, #8916, #10821 ),
 .UNSPECIFIED., .F., .F.,
 ( 4, 1, 1, 1, 2, 2, 2, 1, 1, 1, 2, 2, 4 ),
 ( 0.000000000000000000, 0.1250000000000162925, 0.1875000000000264511, 0.2187500000000315026, 0.2343750000000323075, 0.2500000000000330846, 0.5000000000000234257, 0.6250000000000184297, 0.6875000000000157652, 0.7187500000000145439, 0.7343750000000153211, 0.7500000000000160982, 1.000000000000000000 ),
 .UNSPECIFIED. ) ;
#3702 = CARTESIAN_POINT ( 'NONE',  ( 24.96433005672375316, 10.36502315879739022, -0.6999999999999784173 ) ) ;
#3703 = CARTESIAN_POINT ( 'NONE',  ( -4.216405105086598049, 0.6620460458895751632, -44.10000000002499121 ) ) ;
#3704 = EDGE_CURVE ( 'NONE', #18212, #13864, #19114, .T. ) ;
#3705 =( LENGTH_UNIT ( ) NAMED_UNIT ( * ) SI_UNIT ( .MILLI., .METRE. ) );
#3706 = DIRECTION ( 'NONE',  ( -1.000000000000000000, 0.000000000000000000, 0.000000000000000000 ) ) ;
#3707 = LINE ( 'NONE', #745, #23520 ) ;
#3708 = CARTESIAN_POINT ( 'NONE',  ( -1.219854050253890598, 4.750520449216602437, -66.20876360982499875 ) ) ;
#3709 = VERTEX_POINT ( 'NONE', #11623 ) ;
#3710 = CARTESIAN_POINT ( 'NONE',  ( 19.53679696397345822, 20.00007140946951623, 230.2446877367954130 ) ) ;
#3711 = ORIENTED_EDGE ( 'NONE', *, *, #10079, .T. ) ;
#3712 = CARTESIAN_POINT ( 'NONE',  ( -4.667733413672338294, -30.93201666653739323, 0.8585780189999947520 ) ) ;
#3713 = ORIENTED_EDGE ( 'NONE', *, *, #26507, .T. ) ;
#3714 = VECTOR ( 'NONE', #13963, 1000.000000000000000 ) ;
#3715 = TOROIDAL_SURFACE ( 'NONE', #9237, 30.50000000000000000, 3.000000000000000000 ) ;
#3716 = CARTESIAN_POINT ( 'NONE',  ( -23.23277126416379801, -15.26692729116844482, 4.999998581000003384 ) ) ;
#3717 = AXIS2_PLACEMENT_3D ( 'NONE', #5298, #2326, #14899 ) ;
#3718 = CARTESIAN_POINT ( 'NONE',  ( 28.49999999970000175, -7.466149220240000162, 229.0000000000000000 ) ) ;
#3719 = DIRECTION ( 'NONE',  ( 0.000000000000000000, 0.000000000000000000, 1.000000000000000000 ) ) ;
#3720 = B_SPLINE_CURVE_WITH_KNOTS ( 'NONE', 3,
 ( #29824, #29980, #25115, #27166, #5600, #27464, #15833, #3549, #29679, #898 ),
 .UNSPECIFIED., .F., .F.,
 ( 4, 2, 2, 2, 4 ),
 ( 0.000000000000000000, 0.2500000000000000000, 0.5000000000000000000, 0.7500000000000000000, 1.000000000000000000 ),
 .UNSPECIFIED. ) ;
#3721 = AXIS2_PLACEMENT_3D ( 'NONE', #2917, #877, #425 ) ;
#3722 = CARTESIAN_POINT ( 'NONE',  ( -17.49999999965344344, -27.00000000000000000, -28.40000000020000215 ) ) ;
#3723 = CARTESIAN_POINT ( 'NONE',  ( -12.57202792198699370, -22.00000000000000711, -26.18683049397497342 ) ) ;
#3724 = CARTESIAN_POINT ( 'NONE',  ( -1.063084826889999945, -27.77996807399999923, 224.6898005070000011 ) ) ;
#3725 = ORIENTED_EDGE ( 'NONE', *, *, #25276, .F. ) ;
#3726 = LINE ( 'NONE', #30323, #10479 ) ;
#3727 = CARTESIAN_POINT ( 'NONE',  ( 3.690858198475444940, -2.451543251927155165, -0.7069547853999700315 ) ) ;
#3728 = CARTESIAN_POINT ( 'NONE',  ( 3.766879923516746942, -0.5905747970024824989, -69.09328119617570962 ) ) ;
#3729 = CARTESIAN_POINT ( 'NONE',  ( -2.594691348381471308, -2.505853015390347771, 230.7743357003607230 ) ) ;
#3730 = CARTESIAN_POINT ( 'NONE',  ( -7.999999999710018628, -24.10104989765104833, -29.26619909559191157 ) ) ;
#3731 = CARTESIAN_POINT ( 'NONE',  ( -9.000000000000000000, -54.99999999999998579, -42.39999999999999858 ) ) ;
#3732 =( GEOMETRIC_REPRESENTATION_CONTEXT ( 3 ) GLOBAL_UNCERTAINTY_ASSIGNED_CONTEXT ( ( #30785 ) ) GLOBAL_UNIT_ASSIGNED_CONTEXT ( ( #28244, #6845, #25592 ) ) REPRESENTATION_CONTEXT ( 'NONE', 'WORKASPACE' ) );
#3733 = CARTESIAN_POINT ( 'NONE',  ( 9.999999999974161113, -24.60099947350716576, -30.24364016088963325 ) ) ;
#3734 = CARTESIAN_POINT ( 'NONE',  ( 27.79539923781684507, 0.5057481689249130330, 1.000000000000000888 ) ) ;
#3735 = CARTESIAN_POINT ( 'NONE',  ( 4.172426907288941500, -2.584475198598515266, -48.58324460762500507 ) ) ;
#3736 = CARTESIAN_POINT ( 'NONE',  ( 21.17691543559999801, 18.05241775060000009, 224.9999999359999947 ) ) ;
#3737 = CARTESIAN_POINT ( 'NONE',  ( -4.861312627696711353, 5.804452288037651009, -41.97909262148694154 ) ) ;
#3738 = B_SPLINE_CURVE_WITH_KNOTS ( 'NONE', 3,
 ( #19763, #12513, #20648, #29347, #30246, #6010, #19916, #10898, #7789, #1464, #10323, #13241, #26837, #29503, #5433, #17082, #8359, #26682 ),
 .UNSPECIFIED., .F., .F.,
 ( 4, 2, 2, 2, 2, 2, 2, 2, 4 ),
 ( 0.000000000000000000, 0.1250000000000000000, 0.2500000000000000000, 0.3750000000000000000, 0.5000000000000000000, 0.6250000000000000000, 0.7500000000000000000, 0.8750000000000000000, 1.000000000000000000 ),
 .UNSPECIFIED. ) ;
#3739 = CARTESIAN_POINT ( 'NONE',  ( 14.84775334008999970, -24.60220466919999893, -24.01086508770000094 ) ) ;
#3740 = CARTESIAN_POINT ( 'NONE',  ( -7.508028841131164199, -6.618005260559139735, -34.25135233424746417 ) ) ;
#3741 = CARTESIAN_POINT ( 'NONE',  ( -1.421085471519999843E-14, -1.421085471519999843E-14, 86.39444872449999480 ) ) ;
#3742 = EDGE_CURVE ( 'NONE', #20431, #27935, #4542, .T. ) ;
#3743 = TOROIDAL_SURFACE ( 'NONE', #17786, 3.176829268290000563, 0.2500000000000000000 ) ;
#3744 = AXIS2_PLACEMENT_3D ( 'NONE', #31113, #5131, #14744 ) ;
#3745 = AXIS2_PLACEMENT_3D ( 'NONE', #22899, #24788, #12978 ) ;
#3746 = CARTESIAN_POINT ( 'NONE',  ( 9.335826947264928677, -25.12147279754469764, 25.39506634091258164 ) ) ;
#3747 = ORIENTED_EDGE ( 'NONE', *, *, #19281, .T. ) ;
#3748 = CIRCLE ( 'NONE', #22283, 1.100000000390000787 ) ;
#3749 = EDGE_CURVE ( 'NONE', #24996, #28749, #1616, .T. ) ;
#3750 = CARTESIAN_POINT ( 'NONE',  ( 4.556810990865953315, -1.030009251744165688, -32.78377053309999667 ) ) ;
#3751 = ADVANCED_FACE ( 'NONE', ( #25950, #21384, #14457, #13833 ), #2475, .T. ) ;
#3752 = EDGE_LOOP ( 'NONE', ( #7079, #285, #12350, #11072 ) ) ;
#3753 = B_SPLINE_CURVE_WITH_KNOTS ( 'NONE', 3,
 ( #19400, #5074, #2102, #28378, #9329, #9639 ),
 .UNSPECIFIED., .F., .F.,
 ( 4, 2, 4 ),
 ( 0.000000000000000000, 0.5000000000000000000, 1.000000000000000000 ),
 .UNSPECIFIED. ) ;
#3754 = LINE ( 'NONE', #10374, #21323 ) ;
#3755 = CARTESIAN_POINT ( 'NONE',  ( -4.320323480314920417, -1.509945384023513082, -50.40743646232499486 ) ) ;
#3756 = ORIENTED_EDGE ( 'NONE', *, *, #27121, .F. ) ;
#3757 = CONTEXT_DEPENDENT_SHAPE_REPRESENTATION ( #20644, #22482 ) ;
#3758 = VERTEX_POINT ( 'NONE', #9408 ) ;
#3759 = ORIENTED_EDGE ( 'NONE', *, *, #16635, .F. ) ;
#3760 = CARTESIAN_POINT ( 'NONE',  ( 28.49528339128749366, 0.5184828350247212558, 1.000000000000000888 ) ) ;
#3761 = CARTESIAN_POINT ( 'NONE',  ( -0.5653960855887967263, -27.79447351536211741, 5.289252711543936947 ) ) ;
#3762 = CARTESIAN_POINT ( 'NONE',  ( -8.881784197000000993E-16, -8.881784197000000993E-16, 227.6412452697800006 ) ) ;
#3763 = CARTESIAN_POINT ( 'NONE',  ( 11.20000000009999930, -32.00000000000000000, -28.39999999989999679 ) ) ;
#3764 = CARTESIAN_POINT ( 'NONE',  ( -0.2195863013093272698, -27.49906791309031462, 3.912356533825281257 ) ) ;
#3765 = CARTESIAN_POINT ( 'NONE',  ( 27.63177371540000138, -3.383804565919999808E-15, 92.63947604839999883 ) ) ;
#3766 = CARTESIAN_POINT ( 'NONE',  ( 6.105340317846409626, -0.2107885887935728730, -2.085409721200005784 ) ) ;
#3767 = CARTESIAN_POINT ( 'NONE',  ( -3.484101657925389173, -0.9653352591375119474, 227.7128614111470597 ) ) ;
#3768 = FACE_OUTER_BOUND ( 'NONE', #23895, .T. ) ;
#3769 = AXIS2_PLACEMENT_3D ( 'NONE', #819, #7576, #10409 ) ;
#3770 = ORIENTED_EDGE ( 'NONE', *, *, #17978, .F. ) ;
#3771 = CARTESIAN_POINT ( 'NONE',  ( 1.086829820489895848, 5.988658659452708477, -14.02400681850000197 ) ) ;
#3772 = CARTESIAN_POINT ( 'NONE',  ( 4.457006042266220547, -0.7452897422089094226, -34.80767599850000238 ) ) ;
#3773 = CARTESIAN_POINT ( 'NONE',  ( -16.04158851053540857, -9.763538383445707680, -0.6999999999999784173 ) ) ;
#3774 = CARTESIAN_POINT ( 'NONE',  ( 18.15349680648220954, 19.92137135063213549, 0.007031429000020628095 ) ) ;
#3775 = CARTESIAN_POINT ( 'NONE',  ( -2.219613442066195930, -3.155516745172294080, 227.8440641264227793 ) ) ;
#3776 = CARTESIAN_POINT ( 'NONE',  ( -7.999999999627967817, -15.63018644032419857, -40.59129444282516630 ) ) ;
#3777 = DIRECTION ( 'NONE',  ( 0.000000000000000000, -2.259525899719999991E-12, -1.000000000000000000 ) ) ;
#3778 = EDGE_CURVE ( 'NONE', #17932, #15300, #24638, .T. ) ;
#3779 = B_SPLINE_CURVE_WITH_KNOTS ( 'NONE', 1,
 ( #10412, #22530 ),
 .UNSPECIFIED., .F., .F.,
 ( 2, 2 ),
 ( -2.555897717360000054E-06, 0.7000000000009999335 ),
 .UNSPECIFIED. ) ;
#3780 = CARTESIAN_POINT ( 'NONE',  ( 23.82458380820737531, 13.44211522811278314, -0.6999999999999784173 ) ) ;
#3781 = CARTESIAN_POINT ( 'NONE',  ( 17.95841148948556310, 10.23646161652002817, -0.6999999989999727834 ) ) ;
#3782 = DIRECTION ( 'NONE',  ( -0.7071067811865475727, -0.7071067811865475727, 0.000000000000000000 ) ) ;
#3783 = VECTOR ( 'NONE', #2539, 1000.000000000000114 ) ;
#3784 = ORIENTED_EDGE ( 'NONE', *, *, #14756, .T. ) ;
#3785 = FACE_OUTER_BOUND ( 'NONE', #14012, .T. ) ;
#3786 = CARTESIAN_POINT ( 'NONE',  ( 2.594691348412234255, 2.505853015323757038, 230.7743357003746496 ) ) ;
#3787 = B_SPLINE_CURVE_WITH_KNOTS ( 'NONE', 3,
 ( #6551, #25286, #3723, #25763, #23567, #4193, #15847, #22931, #20721, #15675, #13795, #13320, #23410, #1840, #25451, #28262, #11438, #8752, #18360, #29992 ),
 .UNSPECIFIED., .F., .F.,
 ( 4, 1, 1, 1, 2, 2, 2, 1, 1, 1, 2, 2, 4 ),
 ( 0.000000000000000000, 0.1249999999999970302, 0.1874999999999956146, 0.2187499999999950318, 0.2343749999999946432, 0.2499999999999942824, 0.4999999999999947820, 0.6249999999999950040, 0.6874999999999952260, 0.7187499999999952260, 0.7343749999999943379, 0.7499999999999933387, 1.000000000000000000 ),
 .UNSPECIFIED. ) ;
#3788 = ORIENTED_EDGE ( 'NONE', *, *, #4297, .T. ) ;
#3789 = CARTESIAN_POINT ( 'NONE',  ( -22.64684861875350563, -14.33122899593499611, 224.7819332085316830 ) ) ;
#3790 = CYLINDRICAL_SURFACE ( 'NONE', #2186, 3.500000000000000444 ) ;
#3791 = CARTESIAN_POINT ( 'NONE',  ( 9.999999999957283947, -34.37899275736651106, -24.26894200096920073 ) ) ;
#3792 = ORIENTED_EDGE ( 'NONE', *, *, #25781, .F. ) ;
#3793 = CARTESIAN_POINT ( 'NONE',  ( -26.57440914490000239, -3.469982507400000582, -0.6999999995999997005 ) ) ;
#3794 = ORIENTED_EDGE ( 'NONE', *, *, #26245, .F. ) ;
#3795 = VERTEX_POINT ( 'NONE', #19012 ) ;
#3796 =( NAMED_UNIT ( * ) PLANE_ANGLE_UNIT ( ) SI_UNIT ( $, .RADIAN. ) );
#3797 = ORIENTED_EDGE ( 'NONE', *, *, #23034, .T. ) ;
#3798 = CARTESIAN_POINT ( 'NONE',  ( -0.8958568848479999680, -28.48628573779999940, 224.3198333100000070 ) ) ;
#3799 = PRODUCT ( 'Nut M6', 'Nut M6', '', ( #25788 ) ) ;
#3800 = ORIENTED_EDGE ( 'NONE', *, *, #10791, .T. ) ;
#3801 = DIRECTION ( 'NONE',  ( 1.000000000000000000, -1.843431230200084908E-12, 2.650498504963248473E-12 ) ) ;
#3802 = CARTESIAN_POINT ( 'NONE',  ( -16.83342759579999637, -9.000000000000001776, -0.8000000000000020428 ) ) ;
#3803 = CARTESIAN_POINT ( 'NONE',  ( 2.456693329403278447, 3.027921411505207328, -35.69999999999999574 ) ) ;
#3804 = CARTESIAN_POINT ( 'NONE',  ( 2.853188778929502512, -3.824801971133652945, -95.04434131334036806 ) ) ;
#3805 = CARTESIAN_POINT ( 'NONE',  ( 9.506387914194320388, -25.80482363264563972, 204.8513626972847135 ) ) ;
#3806 = CARTESIAN_POINT ( 'NONE',  ( 3.460344806775433657, -1.006506982961865582, 227.7058346192795852 ) ) ;
#3807 = CARTESIAN_POINT ( 'NONE',  ( 26.80000000069999899, -3.281945028320000125E-15, 186.7828584129999854 ) ) ;
#3808 = EDGE_CURVE ( 'NONE', #7280, #9797, #18494, .T. ) ;
#3809 = VERTEX_POINT ( 'NONE', #26105 ) ;
#3810 = EDGE_CURVE ( 'NONE', #359, #7467, #16800, .T. ) ;
#3811 = CARTESIAN_POINT ( 'NONE',  ( 4.360957369889326252, -0.1505632777267507105, -2.685409721200002320 ) ) ;
#3812 = CARTESIAN_POINT ( 'NONE',  ( 3.713067847428462631, -3.043557113396612390, -23.05924734060000603 ) ) ;
#3813 = CARTESIAN_POINT ( 'NONE',  ( 26.57440914490000239, -3.469982507400000582, -1.399999999999998579 ) ) ;
#3814 = CARTESIAN_POINT ( 'NONE',  ( 1.976074114793839431, -0.3084332875059760948, 231.1412452697749984 ) ) ;
#3815 = CARTESIAN_POINT ( 'NONE',  ( 24.69936741169999905, -14.21947533890000059, 223.9000014189999774 ) ) ;
#3816 = CARTESIAN_POINT ( 'NONE',  ( -17.83931601680000156, 20.00000000000000000, 230.6999999999999886 ) ) ;
#3817 = CARTESIAN_POINT ( 'NONE',  ( 17.85685193732696519, 10.13116291529594371, -0.6999999999999784173 ) ) ;
#3818 = CARTESIAN_POINT ( 'NONE',  ( 9.999999999979998222, -127.2537437101000108, -34.36317024011000143 ) ) ;
#3819 = EDGE_CURVE ( 'NONE', #1522, #24923, #19473, .T. ) ;
#3820 = CARTESIAN_POINT ( 'NONE',  ( -17.89998469250338431, 10.69382497388279063, -0.000000000000000000 ) ) ;
#3821 = CARTESIAN_POINT ( 'NONE',  ( 12.06200471259999851, -24.13482272330000100, 230.6999999999999886 ) ) ;
#3822 = CARTESIAN_POINT ( 'NONE',  ( 10.99289321870000080, -24.65831413369999936, -1.692893218799999877 ) ) ;
#3823 = ORIENTED_EDGE ( 'NONE', *, *, #14624, .T. ) ;
#3824 = CARTESIAN_POINT ( 'NONE',  ( 5.975646968830259809, -0.1056191442178888718, -57.61793411332499915 ) ) ;
#3825 = CARTESIAN_POINT ( 'NONE',  ( -17.64448518804790567, -20.25643828355106990, 36.78285841153859081 ) ) ;
#3826 = VERTEX_POINT ( 'NONE', #7211 ) ;
#3827 = CARTESIAN_POINT ( 'NONE',  ( -5.857861475075242019, -1.837656413297739766, -10.02323088899999881 ) ) ;
#3828 = ORIENTED_EDGE ( 'NONE', *, *, #3749, .F. ) ;
#3829 = FACE_OUTER_BOUND ( 'NONE', #29994, .T. ) ;
#3830 = CARTESIAN_POINT ( 'NONE',  ( -3.194602321395983768, -2.288596850062932564, -68.10000000002500542 ) ) ;
#3831 = VERTEX_POINT ( 'NONE', #14302 ) ;
#3832 = ADVANCED_FACE ( 'NONE', ( #4856 ), #17943, .T. ) ;
#3833 = ORIENTED_EDGE ( 'NONE', *, *, #13547, .T. ) ;
#3834 = VERTEX_POINT ( 'NONE', #21075 ) ;
#3835 = CARTESIAN_POINT ( 'NONE',  ( 3.402386003322844132, -0.8968976485441944035, -94.01209571138487320 ) ) ;
#3836 = ORIENTED_EDGE ( 'NONE', *, *, #3920, .F. ) ;
#3837 = CARTESIAN_POINT ( 'NONE',  ( 0.000000000000000000, 0.000000000000000000, 190.0000000000000000 ) ) ;
#3838 = PLANE ( 'NONE',  #26526 ) ;
#3839 = CARTESIAN_POINT ( 'NONE',  ( 2.994727039187461415, -3.426347720743794234, -64.49605006312501132 ) ) ;
#3840 = CARTESIAN_POINT ( 'NONE',  ( -26.80000000000000071, -9.846360514330001479, 230.0000000000000000 ) ) ;
#3841 = B_SPLINE_CURVE_WITH_KNOTS ( 'NONE', 3,
 ( #22458, #10807, #24966, #10499, #18021, #29687 ),
 .UNSPECIFIED., .F., .F.,
 ( 4, 2, 4 ),
 ( 0.000000000000000000, 0.5000000000000000000, 1.000000000000000000 ),
 .UNSPECIFIED. ) ;
#3842 = B_SPLINE_CURVE_WITH_KNOTS ( 'NONE', 3,
 ( #14661, #14508, #12593, #2544, #2845, #24104, #26461, #3001, #12130, #31025 ),
 .UNSPECIFIED., .F., .F.,
 ( 4, 2, 2, 2, 4 ),
 ( 0.000000000000000000, 0.2500000000000000000, 0.5000000000000000000, 0.7500000000000000000, 1.000000000000000000 ),
 .UNSPECIFIED. ) ;
#3843 = LINE ( 'NONE', #25561, #24720 ) ;
#3844 = CARTESIAN_POINT ( 'NONE',  ( 0.000000000000000000, 0.000000000000000000, 229.6412452697800006 ) ) ;
#3845 = CARTESIAN_POINT ( 'NONE',  ( -17.47798013194186950, -24.05818843344536972, -24.32488866329982358 ) ) ;
#3846 = ORIENTED_EDGE ( 'NONE', *, *, #29825, .F. ) ;
#3847 = CARTESIAN_POINT ( 'NONE',  ( -25.46368746804859740, 12.80129684245613575, 4.999998581000003384 ) ) ;
#3848 = CARTESIAN_POINT ( 'NONE',  ( 4.741512700999319208, 1.965332957690412385, -10.55511350020000094 ) ) ;
#3849 = CYLINDRICAL_SURFACE ( 'NONE', #5264, 3.000000000000000444 ) ;
#3850 = ORIENTED_EDGE ( 'NONE', *, *, #27186, .F. ) ;
#3851 = CARTESIAN_POINT ( 'NONE',  ( 24.68173674080000168, -14.25001227039999918, 223.9000014189999774 ) ) ;
#3852 = CARTESIAN_POINT ( 'NONE',  ( -23.09885119212171389, -13.58970608817446823, 3.912379060515961626 ) ) ;
#3853 = CARTESIAN_POINT ( 'NONE',  ( -24.29089620838935204, -14.90695587844356673, 6.079851352000009257 ) ) ;
#3854 = EDGE_CURVE ( 'NONE', #14604, #25327, #26740, .T. ) ;
#3855 = CARTESIAN_POINT ( 'NONE',  ( 9.993285220779439371, -25.61999708228226424, 27.46709065302605168 ) ) ;
#3856 = CARTESIAN_POINT ( 'NONE',  ( 16.37473331892315542, -8.236461616552139375, -0.6999999989999727834 ) ) ;
#3857 = CARTESIAN_POINT ( 'NONE',  ( -17.57665938409742523, -8.186054152995293265, 0.000000000000000000 ) ) ;
#3858 = CARTESIAN_POINT ( 'NONE',  ( -11.66358246699999945, -24.14124255240000139, -1.399999999999998579 ) ) ;
#3859 = FACE_OUTER_BOUND ( 'NONE', #27204, .T. ) ;
#3860 = ORIENTED_EDGE ( 'NONE', *, *, #14976, .T. ) ;
#3861 = CARTESIAN_POINT ( 'NONE',  ( 6.999999999814658480, -5.287238791122498505, -26.38853270481357072 ) ) ;
#3862 = CARTESIAN_POINT ( 'NONE',  ( 27.79999999990000248, 4.333901782529999025, 222.0000000000000000 ) ) ;
#3863 = CARTESIAN_POINT ( 'NONE',  ( 2.384187449509611589, -3.542147544710181339, -68.10000000002500542 ) ) ;
#3864 = EDGE_CURVE ( 'NONE', #6498, #29484, #25242, .T. ) ;
#3865 = ADVANCED_FACE ( 'NONE', ( #5808 ), #15707, .T. ) ;
#3866 = CARTESIAN_POINT ( 'NONE',  ( 3.454291557259786316, 0.6014336072404916633, -68.65942561803572630 ) ) ;
#3867 = CARTESIAN_POINT ( 'NONE',  ( -4.054871305269121429, -0.4479528304393000093, -44.10000000002499121 ) ) ;
#3868 =( LENGTH_UNIT ( ) NAMED_UNIT ( * ) SI_UNIT ( .MILLI., .METRE. ) );
#3869 = DIRECTION ( 'NONE',  ( -2.415891560877031462E-12, 0.9341647027306021478, 0.3568421334038983650 ) ) ;
#3870 = CARTESIAN_POINT ( 'NONE',  ( -10.94971440929931106, -24.68950648801511605, -1.737779038943164212 ) ) ;
#3871 = EDGE_CURVE ( 'NONE', #7336, #27477, #26021, .T. ) ;
#3872 = CARTESIAN_POINT ( 'NONE',  ( 3.916181512753878824, -4.480608557854155904, -64.49605006312501132 ) ) ;
#3873 = ORIENTED_EDGE ( 'NONE', *, *, #3445, .T. ) ;
#3874 = DIRECTION ( 'NONE',  ( 0.000000000000000000, 0.000000000000000000, -1.000000000000000000 ) ) ;
#3875 = EDGE_CURVE ( 'NONE', #25571, #9871, #3439, .T. ) ;
#3876 = EDGE_LOOP ( 'NONE', ( #30607, #14615, #9443, #30664 ) ) ;
#3877 = CARTESIAN_POINT ( 'NONE',  ( 2.888061030912462801, -2.091444806055747563, -88.52261276308685467 ) ) ;
#3878 = ORIENTED_EDGE ( 'NONE', *, *, #10373, .F. ) ;
#3879 = CARTESIAN_POINT ( 'NONE',  ( 16.06413493411159976, -8.876045783929967570, -4.336808689942017736E-16 ) ) ;
#3880 =( NAMED_UNIT ( * ) PLANE_ANGLE_UNIT ( ) SI_UNIT ( $, .RADIAN. ) );
#3881 = DIRECTION ( 'NONE',  ( 0.000000000000000000, 0.000000000000000000, -1.000000000000000000 ) ) ;
#3882 = CARTESIAN_POINT ( 'NONE',  ( -3.685684228003564655, -0.6162076564376223198, 230.7072465799074905 ) ) ;
#3883 = CARTESIAN_POINT ( 'NONE',  ( 0.1319790757220171973, -27.80015609199433158, 3.957670871000018575 ) ) ;
#3884 = EDGE_CURVE ( 'NONE', #9121, #31008, #331, .T. ) ;
#3885 = DIRECTION ( 'NONE',  ( -0.5000000000001894040, 0.8660254037843291286, 0.000000000000000000 ) ) ;
#3886 = CARTESIAN_POINT ( 'NONE',  ( 0.000000000000000000, -1.776356839399999804E-15, 227.6412452697800006 ) ) ;
#3887 = ORIENTED_EDGE ( 'NONE', *, *, #1625, .T. ) ;
#3888 = CARTESIAN_POINT ( 'NONE',  ( 20.77600629922060449, 21.68409807857484140, 1.000000000000000888 ) ) ;
#3889 = LINE ( 'NONE', #16003, #28859 ) ;
#3890 = CARTESIAN_POINT ( 'NONE',  ( -8.699999999662093586, -15.94902145834643115, -35.53273252493492862 ) ) ;
#3891 = CIRCLE ( 'NONE', #17446, 2.999999999999999556 ) ;
#3892 = CARTESIAN_POINT ( 'NONE',  ( -17.93392337644938905, -8.982759033125498505, 0.000000000000000000 ) ) ;
#3893 = CARTESIAN_POINT ( 'NONE',  ( 0.000000000000000000, -50.49316738903675628, -44.10000000000000142 ) ) ;
#3894 = DIRECTION ( 'NONE',  ( -1.000000000000000000, 0.000000000000000000, 0.000000000000000000 ) ) ;
#3895 = CARTESIAN_POINT ( 'NONE',  ( 7.105427357599999217E-15, 3.552713678799999608E-15, 143.6055512749999821 ) ) ;
#3896 = CARTESIAN_POINT ( 'NONE',  ( 22.63260994176697238, -19.28417101125922883, 0.000000000000000000 ) ) ;
#3897 = CARTESIAN_POINT ( 'NONE',  ( 3.874396413951474827, -2.399869827310081583, -48.93324460762499939 ) ) ;
#3898 = ADVANCED_FACE ( 'NONE', ( #5958 ), #15880, .F. ) ;
#3899 = B_SPLINE_CURVE_WITH_KNOTS ( 'NONE', 3,
 ( #7160, #3203, #3049, #1158, #22252, #22569, #12641, #15019, #22715, #709 ),
 .UNSPECIFIED., .F., .F.,
 ( 4, 2, 2, 2, 4 ),
 ( 0.000000000000000000, 0.2500000000000000000, 0.5000000000000000000, 0.7500000000000000000, 1.000000000000000000 ),
 .UNSPECIFIED. ) ;
#3900 = CARTESIAN_POINT ( 'NONE',  ( 14.84171152945961047, -24.10535842370141424, -24.29771940128471996 ) ) ;
#3901 = CARTESIAN_POINT ( 'NONE',  ( 7.040872694808040677, 5.396991261850427435, -40.11145768973216974 ) ) ;
#3902 = CARTESIAN_POINT ( 'NONE',  ( 3.489756073974365602, -0.9552379302931907068, 230.7680100055977732 ) ) ;
#3903 = CARTESIAN_POINT ( 'NONE',  ( -24.29812717103635933, -12.87956648275837779, 224.5094458564340698 ) ) ;
#3904 = ORIENTED_EDGE ( 'NONE', *, *, #22187, .F. ) ;
#3905 = CARTESIAN_POINT ( 'NONE',  ( 5.877945039781666381, 1.734296231098907182, -35.53159726780000227 ) ) ;
#3906 = VERTEX_POINT ( 'NONE', #25005 ) ;
#3907 = CARTESIAN_POINT ( 'NONE',  ( -4.535753307212162078, -3.367775055652930227, -56.27895058492499913 ) ) ;
#3908 = ORIENTED_EDGE ( 'NONE', *, *, #13956, .T. ) ;
#3909 = AXIS2_PLACEMENT_3D ( 'NONE', #19589, #22105, #9834 ) ;
#3910 = APPLICATION_PROTOCOL_DEFINITION ( 'draft international standard', 'automotive_design', 1998, #6577 ) ;
#3911 = VERTEX_POINT ( 'NONE', #17905 ) ;
#3912 = VECTOR ( 'NONE', #30304, 1000.000000000000114 ) ;
#3913 = VECTOR ( 'NONE', #4734, 1000.000000000000114 ) ;
#3914 = ORIENTED_EDGE ( 'NONE', *, *, #8898, .T. ) ;
#3915 = CARTESIAN_POINT ( 'NONE',  ( 14.75521759265642707, -30.61078560332397913, -24.71147133353610315 ) ) ;
#3916 = DIRECTION ( 'NONE',  ( 0.9316362575375356503, 0.3633921898465274913, 0.000000000000000000 ) ) ;
#3917 = FILL_AREA_STYLE ('',( #30189 ) ) ;
#3918 = CARTESIAN_POINT ( 'NONE',  ( 0.000000000000000000, 0.000000000000000000, 115.0000000000000000 ) ) ;
#3919 = CARTESIAN_POINT ( 'NONE',  ( -0.9877995808046760029, -27.48272658602412477, 4.509012502174277515 ) ) ;
#3920 = EDGE_CURVE ( 'NONE', #6451, #1635, #13513, .T. ) ;
#3921 = FACE_OUTER_BOUND ( 'NONE', #27237, .T. ) ;
#3922 = CARTESIAN_POINT ( 'NONE',  ( -0.7873752056533345201, -4.273814420472608511, -3.525234013000005717 ) ) ;
#3923 = CARTESIAN_POINT ( 'NONE',  ( 0.2653940490574222544, -2.000000000000000444, 230.8412452700000301 ) ) ;
#3924 = CARTESIAN_POINT ( 'NONE',  ( 8.000000000000000000, -15.86465192213301556, -74.65259062561435144 ) ) ;
#3925 = VECTOR ( 'NONE', #20505, 1000.000000000000227 ) ;
#3926 = EDGE_CURVE ( 'NONE', #9909, #1865, #22962, .T. ) ;
#3927 = CARTESIAN_POINT ( 'NONE',  ( 3.082386449366550263, -3.056625787687238471, -15.06112212870000455 ) ) ;
#3928 = CARTESIAN_POINT ( 'NONE',  ( -0.3280975466111932248, 4.681158999438244983, -34.89518930510001127 ) ) ;
#3929 = EDGE_CURVE ( 'NONE', #5428, #14489, #25321, .T. ) ;
#3930 = EDGE_CURVE ( 'NONE', #3949, #20395, #20436, .T. ) ;
#3931 = CARTESIAN_POINT ( 'NONE',  ( -13.99999999969999820, 21.69999999929999390, -58.51619611000000276 ) ) ;
#3932 = CARTESIAN_POINT ( 'NONE',  ( -0.8178280313492310993, -26.78758467680351174, 5.737227010353648460 ) ) ;
#3933 = CARTESIAN_POINT ( 'NONE',  ( 0.8057459562559999844, -27.78864806999999715, 224.2403730839999980 ) ) ;
#3934 = CARTESIAN_POINT ( 'NONE',  ( 22.55330502899744616, -17.67890025412993182, 8.000000000000007105 ) ) ;
#3935 = CARTESIAN_POINT ( 'NONE',  ( -27.98978497850000124, 6.821407819560000085, 222.0000000000000000 ) ) ;
#3936 = AXIS2_PLACEMENT_3D ( 'NONE', #19516, #16526, #24231 ) ;
#3937 = CARTESIAN_POINT ( 'NONE',  ( 23.09961856918545919, -13.58841269902310778, 226.0876905688013494 ) ) ;
#3938 = CYLINDRICAL_SURFACE ( 'NONE', #14271, 3.000000000000002220 ) ;
#3939 = DIRECTION ( 'NONE',  ( 0.000000000000000000, 0.4794255386042043932, 0.8775825618903719816 ) ) ;
#3940 = ORIENTED_EDGE ( 'NONE', *, *, #14083, .F. ) ;
#3941 = CARTESIAN_POINT ( 'NONE',  ( -18.95046173579999760, -18.95046173579999760, 93.21714158839999698 ) ) ;
#3942 = ORIENTED_EDGE ( 'NONE', *, *, #2689, .F. ) ;
#3943 = CARTESIAN_POINT ( 'NONE',  ( -1.238178402523181232, -3.500000000000000000, 227.7677604876802491 ) ) ;
#3944 = LINE ( 'NONE', #30541, #7209 ) ;
#3945 = CARTESIAN_POINT ( 'NONE',  ( -0.8162763503540674259, -5.159721775937600619, -0.7000226544067725820 ) ) ;
#3946 = VERTEX_POINT ( 'NONE', #30192 ) ;
#3947 = CARTESIAN_POINT ( 'NONE',  ( 3.248659393266399409, -2.157825791482659294, -43.35875473022499449 ) ) ;
#3948 = VERTEX_POINT ( 'NONE', #13188 ) ;
#3949 = VERTEX_POINT ( 'NONE', #11157 ) ;
#3950 = ORIENTED_EDGE ( 'NONE', *, *, #2701, .F. ) ;
#3951 = CARTESIAN_POINT ( 'NONE',  ( 22.51404573909999840, 18.05178744050000006, 229.4982322489999831 ) ) ;
#3952 = B_SPLINE_CURVE_WITH_KNOTS ( 'NONE', 1,
 ( #12918, #19700 ),
 .UNSPECIFIED., .F., .F.,
 ( 2, 2 ),
 ( -2.556819966299999618E-06, 0.7000000000009999335 ),
 .UNSPECIFIED. ) ;
#3953 = ORIENTED_EDGE ( 'NONE', *, *, #24379, .T. ) ;
#3954 = AXIS2_PLACEMENT_3D ( 'NONE', #3512, #17370, #564 ) ;
#3955 = CARTESIAN_POINT ( 'NONE',  ( 6.818289962769999768, 16.85315611420000081, 230.6999999999999886 ) ) ;
#3956 = CARTESIAN_POINT ( 'NONE',  ( 8.000000000465679051, -16.38256976572606405, -33.02215629541608877 ) ) ;
#3957 = CARTESIAN_POINT ( 'NONE',  ( 1.404941437947275551, -4.946154300792606762, -93.71305981298847598 ) ) ;
#3958 = CIRCLE ( 'NONE', #17030, 2.999999999999999556 ) ;
#3959 = CARTESIAN_POINT ( 'NONE',  ( 14.67495062122367599, -22.00000000000000000, -26.63047724528842153 ) ) ;
#3960 = CARTESIAN_POINT ( 'NONE',  ( 23.54244930488480136, -12.80639529643277008, 5.876648809236738380 ) ) ;
#3961 = CARTESIAN_POINT ( 'NONE',  ( -12.22909343913021551, 26.04501283399531530, -59.39872012629501086 ) ) ;
#3962 = ORIENTED_EDGE ( 'NONE', *, *, #7255, .F. ) ;
#3963 = CARTESIAN_POINT ( 'NONE',  ( 6.086077541567210147, 0.7980478301550381071, -6.226979598400003368 ) ) ;
#3964 = CARTESIAN_POINT ( 'NONE',  ( 0.3233900739386466605, 6.101867874933233793, -22.34418644579999480 ) ) ;
#3965 = CARTESIAN_POINT ( 'NONE',  ( -9.739400760072916441, -25.71769950840797847, 204.0853438175687984 ) ) ;
#3966 = APPLICATION_CONTEXT ( 'automotive_design' ) ;
#3967 = ADVANCED_FACE ( 'NONE', ( #1253 ), #18220, .T. ) ;
#3968 = CARTESIAN_POINT ( 'NONE',  ( 7.999999999944494178, -116.0414483704652042, 19.89613934358488123 ) ) ;
#3969 = CARTESIAN_POINT ( 'NONE',  ( 25.08428924680000094, -13.52916357279999993, 224.2398747240000034 ) ) ;
#3970 = CARTESIAN_POINT ( 'NONE',  ( -1.092383470327443540, -2.615810859415299117, -36.20335296946116443 ) ) ;
#3971 = DIRECTION ( 'NONE',  ( 1.000000000000000000, 0.000000000000000000, 0.000000000000000000 ) ) ;
#3972 = CARTESIAN_POINT ( 'NONE',  ( -3.044741706671135084, -2.260426224203013312, -0.8737437980999990250 ) ) ;
#3973 = VECTOR ( 'NONE', #20105, 1000.000000000000000 ) ;
#3974 = CARTESIAN_POINT ( 'NONE',  ( 23.81569860410000317, -13.75000000000000000, 223.8999999999999773 ) ) ;
#3975 = CARTESIAN_POINT ( 'NONE',  ( -19.80526803560000104, 19.50877411510000314, 228.5999999999999943 ) ) ;
#3976 = DIRECTION ( 'NONE',  ( -2.257102469710000208E-12, 0.000000000000000000, 1.000000000000000000 ) ) ;
#3977 = EDGE_LOOP ( 'NONE', ( #24352, #599, #11382, #10107 ) ) ;
#3978 = CARTESIAN_POINT ( 'NONE',  ( 2.840551633548176191, -3.955783487875848881, -60.77197827312500067 ) ) ;
#3979 = DIRECTION ( 'NONE',  ( 1.000000000000000000, 0.000000000000000000, 0.000000000000000000 ) ) ;
#3980 = ORIENTED_EDGE ( 'NONE', *, *, #985, .F. ) ;
#3981 = CARTESIAN_POINT ( 'NONE',  ( 2.246931792487971702, -6.149078805931920577, -6.260585232200001293 ) ) ;
#3982 = ORIENTED_EDGE ( 'NONE', *, *, #15869, .T. ) ;
#3983 = CARTESIAN_POINT ( 'NONE',  ( 0.000000000000000000, 0.000000000000000000, 192.0603150150000147 ) ) ;
#3984 = VECTOR ( 'NONE', #20531, 1000.000000000000000 ) ;
#3985 = FACE_OUTER_BOUND ( 'NONE', #22993, .T. ) ;
#3986 = ORIENTED_EDGE ( 'NONE', *, *, #18675, .T. ) ;
#3987 = EDGE_CURVE ( 'NONE', #5609, #30396, #9930, .T. ) ;
#3988 = ORIENTED_EDGE ( 'NONE', *, *, #4851, .T. ) ;
#3989 = VERTEX_POINT ( 'NONE', #17605 ) ;
#3990 = FACE_OUTER_BOUND ( 'NONE', #21797, .T. ) ;
#3991 =( LENGTH_UNIT ( ) NAMED_UNIT ( * ) SI_UNIT ( .MILLI., .METRE. ) );
#3992 = ORIENTED_EDGE ( 'NONE', *, *, #908, .F. ) ;
#3993 = DIRECTION ( 'NONE',  ( 0.000000000000000000, 0.000000000000000000, 1.000000000000000000 ) ) ;
#3994 = LINE ( 'NONE', #20834, #11459 ) ;
#3995 = CARTESIAN_POINT ( 'NONE',  ( 3.542472921321142110, 4.818407451951889797, -66.64226422552501106 ) ) ;
#3996 = ADVANCED_FACE ( 'NONE', ( #27213, #15251 ), #3289, .F. ) ;
#3997 = CARTESIAN_POINT ( 'NONE',  ( 27.09307779339999911, 1.385558334729999981E-12, 229.9751247039999953 ) ) ;
#3998 = CARTESIAN_POINT ( 'NONE',  ( -10.99289321870000080, -2.500000000000002220, -1.692893218799999877 ) ) ;
#3999 = CARTESIAN_POINT ( 'NONE',  ( 9.000000000000000000, -55.00000000000001421, -42.39999999999999858 ) ) ;
#4000 = CARTESIAN_POINT ( 'NONE',  ( -23.68794489818531446, -12.53584098786471479, 5.491373161348172438 ) ) ;
#4001 = VERTEX_POINT ( 'NONE', #2344 ) ;
#4002 = CARTESIAN_POINT ( 'NONE',  ( -26.38145030669853952, 5.195434873298933276, -1.399999999999998579 ) ) ;
#4003 = AXIS2_PLACEMENT_3D ( 'NONE', #754, #10646, #20238 ) ;
#4004 = VECTOR ( 'NONE', #18311, 1000.000000000000000 ) ;
#4005 = CARTESIAN_POINT ( 'NONE',  ( 2.536150288113629081, -3.576595042060319862, -11.62388893670000733 ) ) ;
#4006 = LINE ( 'NONE', #27922, #12813 ) ;
#4007 = ORIENTED_EDGE ( 'NONE', *, *, #4030, .T. ) ;
#4008 = CARTESIAN_POINT ( 'NONE',  ( 24.73445225629999911, -14.15837998019999944, 223.9040346120000038 ) ) ;
#4009 = CARTESIAN_POINT ( 'NONE',  ( 17.83928249670000099, 20.00000000010000178, -0.6999999999999992895 ) ) ;
#4010 = DIRECTION ( 'NONE',  ( 0.9316362575375356503, 0.3633921898465274913, 0.000000000000000000 ) ) ;
#4011 = CARTESIAN_POINT ( 'NONE',  ( 27.62942886422533917, 5.076074465521874579, 0.5514269430000329208 ) ) ;
#4012 = CARTESIAN_POINT ( 'NONE',  ( 18.00000000000000000, 0.000000000000000000, 229.6412452697800006 ) ) ;
#4013 = CLOSED_SHELL ( 'NONE', ( #25105, #21530, #17356, #7305, #29201, #22181, #11554, #12812, #287, #11912 ) ) ;
#4014 = CARTESIAN_POINT ( 'NONE',  ( -5.473571180597741836, 3.247285761689575168, -50.83267869292499341 ) ) ;
#4015 = CARTESIAN_POINT ( 'NONE',  ( 8.000000000270995670, -18.23122067931581114, -34.51216076560703527 ) ) ;
#4016 = DIRECTION ( 'NONE',  ( -0.000000000000000000, -0.000000000000000000, -1.000000000000000000 ) ) ;
#4017 = ORIENTED_EDGE ( 'NONE', *, *, #7464, .F. ) ;
#4018 = EDGE_CURVE ( 'NONE', #11678, #29420, #20476, .T. ) ;
#4019 = SURFACE_SIDE_STYLE ('',( #21015 ) ) ;
#4020 = CARTESIAN_POINT ( 'NONE',  ( -28.50000000000000000, -5.472165930259999123E-14, 229.0000000000000000 ) ) ;
#4021 = B_SPLINE_CURVE_WITH_KNOTS ( 'NONE', 5,
 ( #3060, #12656, #19907, #573, #26524, #417 ),
 .UNSPECIFIED., .F., .F.,
 ( 6, 6 ),
 ( 0.000000000000000000, 22.42544452799999988 ),
 .UNSPECIFIED. ) ;
#4022 = B_SPLINE_CURVE_WITH_KNOTS ( 'NONE', 3,
 ( #4404, #6297, #14007, #13690 ),
 .UNSPECIFIED., .F., .F.,
 ( 4, 4 ),
 ( 0.000000000000000000, 1.000000000000000000 ),
 .UNSPECIFIED. ) ;
#4023 = CARTESIAN_POINT ( 'NONE',  ( 2.875741676304124361, -3.508796633370238283, -68.10000000002500542 ) ) ;
#4024 = CARTESIAN_POINT ( 'NONE',  ( 0.8593139071816520147, 2.606839092805549818, -67.92951771365525815 ) ) ;
#4025 = CARTESIAN_POINT ( 'NONE',  ( -24.25455085227292784, 13.58673930470784796, 6.099998580999935527 ) ) ;
#4026 = CARTESIAN_POINT ( 'NONE',  ( 14.74927456580481966, -23.35383567438356778, -32.06809451559220747 ) ) ;
#4027 = CARTESIAN_POINT ( 'NONE',  ( 1.071322544592021586, 4.175463484545726800, -39.51567878490223507 ) ) ;
#4028 = CARTESIAN_POINT ( 'NONE',  ( 2.708949881112989289, 3.684664522020659305, -67.04226422542501496 ) ) ;
#4029 = ORIENTED_EDGE ( 'NONE', *, *, #28216, .T. ) ;
#4030 = EDGE_CURVE ( 'NONE', #19354, #4261, #24504, .T. ) ;
#4031 = CARTESIAN_POINT ( 'NONE',  ( 24.46020335245677657, -13.21278628519231546, 3.926747916559686136 ) ) ;
#4032 = ORIENTED_EDGE ( 'NONE', *, *, #27, .T. ) ;
#4033 = CARTESIAN_POINT ( 'NONE',  ( -27.52676963214412353, -0.5008603480660347440, 0.2686740700000300741 ) ) ;
#4034 = ORIENTED_EDGE ( 'NONE', *, *, #27403, .F. ) ;
#4035 = CARTESIAN_POINT ( 'NONE',  ( -10.00000000001209344, -15.94902145808038618, -35.53273252466679111 ) ) ;
#4036 = CARTESIAN_POINT ( 'NONE',  ( -9.993285220779425160, -25.61999708228226069, 115.0000000000000000 ) ) ;
#4037 = CARTESIAN_POINT ( 'NONE',  ( 9.738910687886932038, -24.96785170200595161, 143.2171415880000040 ) ) ;
#4038 = CARTESIAN_POINT ( 'NONE',  ( -3.040504021322313122, -1.733590290792417887, 0.000000000000000000 ) ) ;
#4039 = CARTESIAN_POINT ( 'NONE',  ( 0.1352650258312465548, -28.50015511220833986, 3.957670871000018575 ) ) ;
#4040 = TOROIDAL_SURFACE ( 'NONE', #11077, 29.80000000000000071, 3.000000000000000000 ) ;
#4041 = DIRECTION ( 'NONE',  ( 0.000000000000000000, 0.000000000000000000, 1.000000000000000000 ) ) ;
#4042 = FACE_OUTER_BOUND ( 'NONE', #18444, .T. ) ;
#4043 = VERTEX_POINT ( 'NONE', #11318 ) ;
#4044 = DIRECTION ( 'NONE',  ( 3.092054264588954770E-24, -1.000000000000000000, 2.257145581552149937E-12 ) ) ;
#4045 = EDGE_CURVE ( 'NONE', #1904, #17421, #22788, .T. ) ;
#4046 = CARTESIAN_POINT ( 'NONE',  ( 27.56257419730000180, -5.215693983959999454E-14, 230.5592437530000041 ) ) ;
#4047 = CARTESIAN_POINT ( 'NONE',  ( -1.809764279169999934, 12.20622105729999873, 232.6627643349999914 ) ) ;
#4048 = EDGE_CURVE ( 'NONE', #22923, #2058, #13991, .T. ) ;
#4049 = CARTESIAN_POINT ( 'NONE',  ( -9.707106781189999367, -130.0000000000000000, -43.10710678118599759 ) ) ;
#4050 = DIRECTION ( 'NONE',  ( 1.000000000000000000, 0.000000000000000000, 0.000000000000000000 ) ) ;
#4051 = CARTESIAN_POINT ( 'NONE',  ( 19.80538212960000166, 19.50875458629999670, 229.0000000010000178 ) ) ;
#4052 = CARTESIAN_POINT ( 'NONE',  ( -0.6750190883921094454, -27.49190635772141889, 225.8804910023025343 ) ) ;
#4053 = AXIS2_PLACEMENT_3D ( 'NONE', #13984, #11311, #14138 ) ;
#4054 = CARTESIAN_POINT ( 'NONE',  ( -15.73360964037622622, -8.979988381802643360, -0.6999999999999784173 ) ) ;
#4055 = CARTESIAN_POINT ( 'NONE',  ( 0.6613659943794023555, -4.850238491497668392, -49.76468436622499780 ) ) ;
#4056 = ADVANCED_FACE ( 'NONE', ( #18544 ), #18336, .T. ) ;
#4057 = CARTESIAN_POINT ( 'NONE',  ( 14.76039189739984359, -23.42146364767391375, -24.69256623432178088 ) ) ;
#4058 = CARTESIAN_POINT ( 'NONE',  ( 18.03376228222516886, 11.69189214368329743, -4.336808689942017736E-16 ) ) ;
#4059 = CARTESIAN_POINT ( 'NONE',  ( 3.494141269252792448, -0.9476394297810019074, 230.7667222917565937 ) ) ;
#4060 = CARTESIAN_POINT ( 'NONE',  ( -8.699999999642283655, -16.96959321760381556, -37.81493174590716677 ) ) ;
#4061 = B_SPLINE_CURVE_WITH_KNOTS ( 'NONE', 3,
 ( #5073, #21609, #4606, #19087, #12001, #24123 ),
 .UNSPECIFIED., .F., .F.,
 ( 4, 2, 4 ),
 ( 0.000000000000000000, 0.5000000000000000000, 1.000000000000000000 ),
 .UNSPECIFIED. ) ;
#4062 = ORIENTED_EDGE ( 'NONE', *, *, #14447, .F. ) ;
#4063 = CARTESIAN_POINT ( 'NONE',  ( -24.09883371379999772, -15.21565466309999870, 224.8957841300000098 ) ) ;
#4064 = EDGE_CURVE ( 'NONE', #10995, #18419, #18695, .T. ) ;
#4065 = VERTEX_POINT ( 'NONE', #4386 ) ;
#4066 = CARTESIAN_POINT ( 'NONE',  ( -3.469775141979342337, 3.953596984337869547, -54.73587006832500634 ) ) ;
#4067 = ORIENTED_EDGE ( 'NONE', *, *, #15423, .T. ) ;
#4068 = SHAPE_DEFINITION_REPRESENTATION ( #22894, #22833 ) ;
#4069 = ORIENTED_EDGE ( 'NONE', *, *, #12913, .F. ) ;
#4070 = ORIENTED_EDGE ( 'NONE', *, *, #10913, .F. ) ;
#4071 = CARTESIAN_POINT ( 'NONE',  ( -8.699999999957434227, -114.1237136948164306, 7.129097339259313770 ) ) ;
#4072 = EDGE_CURVE ( 'NONE', #3826, #21635, #28454, .T. ) ;
#4073 = CARTESIAN_POINT ( 'NONE',  ( -8.699999999664235872, -9.427153351153990002, -35.64619606679892883 ) ) ;
#4074 = FACE_BOUND ( 'NONE', #26241, .T. ) ;
#4075 = AXIS2_PLACEMENT_3D ( 'NONE', #11971, #14183, #30865 ) ;
#4076 = CARTESIAN_POINT ( 'NONE',  ( 7.199615913319999727, -9.684780895279999413, 231.9999991140000191 ) ) ;
#4077 = PLANE ( 'NONE',  #25661 ) ;
#4078 = CARTESIAN_POINT ( 'NONE',  ( -16.85343921394901301, 12.09981795542885585, -1.000005633855494125E-09 ) ) ;
#4079 = CARTESIAN_POINT ( 'NONE',  ( -6.055223678858003389, -2.441925613954294860, -0.3971974345000003903 ) ) ;
#4080 = CARTESIAN_POINT ( 'NONE',  ( -27.29823224880000154, 7.105427357599999217E-15, 230.6577119970000069 ) ) ;
#4081 = ORIENTED_EDGE ( 'NONE', *, *, #13374, .F. ) ;
#4082 = DIRECTION ( 'NONE',  ( 0.5882352941176968164, 0.000000000000000000, -0.8086898285215826654 ) ) ;
#4083 = CARTESIAN_POINT ( 'NONE',  ( -4.278952157217901231, -0.8066629416743145153, -16.09949426530000238 ) ) ;
#4084 = LINE ( 'NONE', #22971, #8706 ) ;
#4085 = CARTESIAN_POINT ( 'NONE',  ( 1.630907767950000142, 5.558498091389999729, 226.6412452697800006 ) ) ;
#4086 = CARTESIAN_POINT ( 'NONE',  ( 4.175165894169885483, -50.49316738903675628, -63.39999999999999858 ) ) ;
#4087 = FACE_OUTER_BOUND ( 'NONE', #12239, .T. ) ;
#4088 = CARTESIAN_POINT ( 'NONE',  ( 27.83860951759415059, -1.869044369023509899, 8.000000000000007105 ) ) ;
#4089 = CARTESIAN_POINT ( 'NONE',  ( -2.874794789347344892, 2.020489689856069582, 227.6523062920440736 ) ) ;
#4090 = PLANE ( 'NONE',  #1172 ) ;
#4091 = CYLINDRICAL_SURFACE ( 'NONE', #11230, 1.099999999999999201 ) ;
#4092 = DIRECTION ( 'NONE',  ( 0.000000000000000000, 1.000000000000000000, 0.000000000000000000 ) ) ;
#4093 = DIRECTION ( 'NONE',  ( 0.000000000000000000, 0.9986295347545772749, 0.05233595624287791515 ) ) ;
#4094 = MECHANICAL_DESIGN_GEOMETRIC_PRESENTATION_REPRESENTATION (  '', ( #2084 ), #8744 ) ;
#4095 = ORIENTED_EDGE ( 'NONE', *, *, #25331, .F. ) ;
#4096 = FACE_OUTER_BOUND ( 'NONE', #20301, .T. ) ;
#4097 = CARTESIAN_POINT ( 'NONE',  ( 3.391070341234815988, -1.345564551309325063, -36.82289348942992291 ) ) ;
#4098 = EDGE_CURVE ( 'NONE', #4224, #97, #14158, .T. ) ;
#4099 = DIRECTION ( 'NONE',  ( 0.000000000000000000, 0.000000000000000000, 1.000000000000000000 ) ) ;
#4100 = ORIENTED_EDGE ( 'NONE', *, *, #13851, .F. ) ;
#4101 = CARTESIAN_POINT ( 'NONE',  ( 0.000000000000000000, 0.000000000000000000, 227.6412452697800006 ) ) ;
#4102 = EDGE_LOOP ( 'NONE', ( #533, #28019, #19197, #15165, #11526, #3521, #18884, #25233, #20427, #3466 ) ) ;
#4103 = VERTEX_POINT ( 'NONE', #6889 ) ;
#4104 = EDGE_CURVE ( 'NONE', #3529, #10318, #17323, .T. ) ;
#4105 = EDGE_LOOP ( 'NONE', ( #7579, #7353, #19430 ) ) ;
#4106 = DIRECTION ( 'NONE',  ( 1.000000000000000000, -3.981000000000000101E-12, 1.940999999999999908E-12 ) ) ;
#4107 = ORIENTED_EDGE ( 'NONE', *, *, #27923, .T. ) ;
#4108 = CARTESIAN_POINT ( 'NONE',  ( -10.69999999999999929, -25.00000000000000000, -26.16393202249999916 ) ) ;
#4109 = CARTESIAN_POINT ( 'NONE',  ( 23.23955039760055641, 15.25661106415676471, 4.791628269000009155 ) ) ;
#4110 = CARTESIAN_POINT ( 'NONE',  ( -23.83861932771936765, -15.61961844720760340, 4.689445057000002137 ) ) ;
#4111 = PLANE ( 'NONE',  #11444 ) ;
#4112 = DIRECTION ( 'NONE',  ( 0.7071067811865475727, 0.7071067811865475727, 0.000000000000000000 ) ) ;
#4113 = CARTESIAN_POINT ( 'NONE',  ( 14.75185518689595376, -21.99999999999999645, -29.70934853584909874 ) ) ;
#4114 = CARTESIAN_POINT ( 'NONE',  ( 23.67274795607547233, -12.56353887348194220, 5.548968161597096937 ) ) ;
#4115 = CARTESIAN_POINT ( 'NONE',  ( 27.50000000000000000, 1.776356839399999804E-15, 186.3944487249999895 ) ) ;
#4116 = ORIENTED_EDGE ( 'NONE', *, *, #29891, .T. ) ;
#4117 = TOROIDAL_SURFACE ( 'NONE', #21709, 24.50000000000000000, 3.200000000000000178 ) ;
#4118 = B_SPLINE_CURVE_WITH_KNOTS ( 'NONE', 5,
 ( #30487, #6703, #10967, #6078, #27957, #16307, #13638, #1684, #15999 ),
 .UNSPECIFIED., .F., .F.,
 ( 6, 3, 6 ),
 ( 0.000000000000000000, 0.7281981532490000575, 1.224410044450000123 ),
 .UNSPECIFIED. ) ;
#4119 = CARTESIAN_POINT ( 'NONE',  ( -5.885952403586735215, -0.3768160556055083488, -5.148838774900003301 ) ) ;
#4120 = CARTESIAN_POINT ( 'NONE',  ( 5.403695180783418373, -1.168003237233325553, -22.79036215650000941 ) ) ;
#4121 = CARTESIAN_POINT ( 'NONE',  ( -9.944224317832761173, -25.63928765730900139, 203.0568480260882041 ) ) ;
#4122 = PRODUCT ( 'Plunger Disc', 'Plunger Disc', '', ( #18536 ) ) ;
#4123 = CARTESIAN_POINT ( 'NONE',  ( -23.73992238019999945, -12.43607998449999918, 225.0000000000000000 ) ) ;
#4124 = CARTESIAN_POINT ( 'NONE',  ( 0.1574870170871346953, 3.500159137053637348, 227.6463841914532509 ) ) ;
#4125 = CARTESIAN_POINT ( 'NONE',  ( -25.00848080823378083, 13.67001762859745639, 6.099998581000005693 ) ) ;
#4126 = CARTESIAN_POINT ( 'NONE',  ( -23.66327188690000227, -14.59170227449999935, 225.7602679599999931 ) ) ;
#4127 = CARTESIAN_POINT ( 'NONE',  ( 23.88846875288458804, -13.62395840498221844, 223.8999999999999773 ) ) ;
#4128 = CARTESIAN_POINT ( 'NONE',  ( 1.000415564672181512, -28.48292217092965828, 6.002515439000016606 ) ) ;
#4129 = DIRECTION ( 'NONE',  ( 0.000000000000000000, 0.000000000000000000, 1.000000000000000000 ) ) ;
#4130 = ORIENTED_EDGE ( 'NONE', *, *, #2509, .F. ) ;
#4131 = CARTESIAN_POINT ( 'NONE',  ( -4.880917369133354278, -2.481566535878938495, -61.56424626872499317 ) ) ;
#4132 = CARTESIAN_POINT ( 'NONE',  ( 20.30405755279999980, 20.00000000000000000, 226.9999998930000231 ) ) ;
#4133 = ORIENTED_EDGE ( 'NONE', *, *, #22688, .T. ) ;
#4134 = CARTESIAN_POINT ( 'NONE',  ( 18.26900987428666667, 10.87604578382501330, -4.336808689942017736E-16 ) ) ;
#4135 = CARTESIAN_POINT ( 'NONE',  ( -1.006352433577557770, 6.195109836679514537, -34.84333403589999278 ) ) ;
#4136 = EDGE_LOOP ( 'NONE', ( #10645, #7084, #21287, #19421 ) ) ;
#4137 = B_SPLINE_CURVE_WITH_KNOTS ( 'NONE', 1,
 ( #28887, #16615 ),
 .UNSPECIFIED., .F., .F.,
 ( 2, 2 ),
 ( -2.557514682700000071E-06, 0.7000000000009999335 ),
 .UNSPECIFIED. ) ;
#4138 = DIRECTION ( 'NONE',  ( -3.927995826131583318E-12, 0.4082287037029531107, 0.9128796883888953273 ) ) ;
#4139 = CARTESIAN_POINT ( 'NONE',  ( -3.579340629180964850, -1.721930992784151293, -68.10000000002500542 ) ) ;
#4141 = ORIENTED_EDGE ( 'NONE', *, *, #13915, .F. ) ;
#4140 = VECTOR ( 'NONE', #22590, 1000.000000000000000 ) ;
#4142 = EDGE_LOOP ( 'NONE', ( #4413, #14991, #5800, #22104 ) ) ;
#4143 = EDGE_LOOP ( 'NONE', ( #17592, #28862, #14441, #6769 ) ) ;
#4144 = CARTESIAN_POINT ( 'NONE',  ( -0.1113126277255008650, -0.6952657331094624915, -40.47787123679744070 ) ) ;
#4145 = B_SPLINE_SURFACE_WITH_KNOTS ( 'NONE', 5, 1, ( 
 ( #25830, #4419 ),
 ( #20629, #4265 ),
 ( #21104, #1287 ),
 ( #30699, #18096 ),
 ( #27700, #6146 ),
 ( #3798, #7549 ),
 ( #20, #29102 ),
 ( #30853, #28643 ),
 ( #28952, #18892 ),
 ( #14024, #16990 ),
 ( #26744, #2063 ),
 ( #14175, #28786 ),
 ( #333, #26443 ),
 ( #21720, #26285 ),
 ( #23779, #19045 ) ),
 .UNSPECIFIED., .F., .F., .F.,
 ( 6, 3, 3, 3, 6 ),
 ( 2, 2 ),
 ( 0.000000000000000000, 0.5239015560140000138, 1.047803112029999983, 1.571704668039999975, 1.746338520049999898 ),
 ( -0.7000000000009999335, 2.556813327499999719E-06 ),
 .UNSPECIFIED. ) ;
#4146 = ADVANCED_FACE ( 'NONE', ( #1873 ), #21571, .F. ) ;
#4147 = SHAPE_REPRESENTATION_RELATIONSHIP ( 'NONE' , 'NONE' ,  #28252, #172 ) ;
#4148 = ORIENTED_EDGE ( 'NONE', *, *, #5761, .F. ) ;
#4149 = CARTESIAN_POINT ( 'NONE',  ( -12.29999999990142534, -25.03345049608028106, -30.95893389568501419 ) ) ;
#4150 = ADVANCED_FACE ( 'NONE', ( #19170 ), #14611, .F. ) ;
#4151 = CARTESIAN_POINT ( 'NONE',  ( 23.30309534860585075, -14.60301215431637800, 4.509445859277517066 ) ) ;
#4152 = CARTESIAN_POINT ( 'NONE',  ( 1.257215589593053906, -4.341675124665346885, -67.70367649352500905 ) ) ;
#4153 = CARTESIAN_POINT ( 'NONE',  ( 25.41516571979999739, -14.56554164990000011, 228.9999999990000106 ) ) ;
#4154 =( REPRESENTATION_RELATIONSHIP ('NONE','NONE', #2712, #8955 ) REPRESENTATION_RELATIONSHIP_WITH_TRANSFORMATION ( #3587 )SHAPE_REPRESENTATION_RELATIONSHIP( ) );
#4155 = CARTESIAN_POINT ( 'NONE',  ( -18.66687140124644984, 20.92780155647522378, -0.2432540810000105580 ) ) ;
#4157 = VECTOR ( 'NONE', #27316, 1000.000000000000000 ) ;
#4156 = CARTESIAN_POINT ( 'NONE',  ( 25.64086108080000059, -11.13108427080000062, 222.0000000000000000 ) ) ;
#4158 = CARTESIAN_POINT ( 'NONE',  ( -17.48838570233622747, -24.25553963907254484, -24.21099845983332344 ) ) ;
#4159 = VERTEX_POINT ( 'NONE', #29070 ) ;
#4160 = CARTESIAN_POINT ( 'NONE',  ( -22.92720033282126124, -13.87810118031797835, 225.9606284813543482 ) ) ;
#4161 = CARTESIAN_POINT ( 'NONE',  ( -4.101794773660127902, 5.071170285176791914, -13.60352819870000474 ) ) ;
#4162 = CARTESIAN_POINT ( 'NONE',  ( 26.80000000000001492, -1.754055898254314183, 136.7828584120000244 ) ) ;
#4163 = DIRECTION ( 'NONE',  ( 0.000000000000000000, 1.000000000000000000, 0.000000000000000000 ) ) ;
#4164 = CIRCLE ( 'NONE', #26265, 1.700000000000000178 ) ;
#4165 = VERTEX_POINT ( 'NONE', #28756 ) ;
#4166 = CARTESIAN_POINT ( 'NONE',  ( 26.38279268013727474, 5.187539658929759767, -1.399999999999998579 ) ) ;
#4167 = DIRECTION ( 'NONE',  ( -1.595945597898660305E-12, -0.7071067811865475727, -0.7071067811865475727 ) ) ;
#4168 = CARTESIAN_POINT ( 'NONE',  ( -8.699999999681903518, -14.92844969908904851, -33.25053330396269047 ) ) ;
#4169 = CARTESIAN_POINT ( 'NONE',  ( 26.85610471403804311, 4.933999481336595494, 0.000000000000000000 ) ) ;
#4170 = DIRECTION ( 'NONE',  ( 1.000000000000000000, 0.000000000000000000, 0.000000000000000000 ) ) ;
#4171 = CARTESIAN_POINT ( 'NONE',  ( -3.855177830964256813, -4.571422008809257420, -59.17407541852499975 ) ) ;
#4172 = CARTESIAN_POINT ( 'NONE',  ( 26.94142135619999934, -8.942955963489998358E-14, 230.0000000000000000 ) ) ;
#4173 = CARTESIAN_POINT ( 'NONE',  ( 8.000000000245886866, -28.22468611110216230, -31.13863906511491209 ) ) ;
#4174 = ORIENTED_EDGE ( 'NONE', *, *, #17484, .T. ) ;
#4175 = CARTESIAN_POINT ( 'NONE',  ( 10.82908725742652223, -27.76276047461856678, 136.7828584120000244 ) ) ;
#4176 = EDGE_CURVE ( 'NONE', #68, #7509, #22002, .T. ) ;
#4177 = CARTESIAN_POINT ( 'NONE',  ( 1.806982085357143886, -3.734583774770322329, -68.10000000002501963 ) ) ;
#4178 = DIRECTION ( 'NONE',  ( 0.3633921898465291567, 0.9316362575375349842, 0.000000000000000000 ) ) ;
#4179 = CARTESIAN_POINT ( 'NONE',  ( -24.24391315703382688, -12.98049462792616815, 225.6749683491732981 ) ) ;
#4180 = VERTEX_POINT ( 'NONE', #21851 ) ;
#4181 = CARTESIAN_POINT ( 'NONE',  ( -10.00000000020644997, -24.37864083493787604, -26.88914305888777534 ) ) ;
#4182 = AXIS2_PLACEMENT_3D ( 'NONE', #24679, #3112, #12096 ) ;
#4183 = CARTESIAN_POINT ( 'NONE',  ( 3.051761028451055680, 3.858721280585067248, -64.38768011632501498 ) ) ;
#4184 = EDGE_LOOP ( 'NONE', ( #19153, #6307, #31003, #10149 ) ) ;
#4185 = LINE ( 'NONE', #16451, #15928 ) ;
#4186 = CARTESIAN_POINT ( 'NONE',  ( -25.12347730974626714, -15.01204873981462384, 0.7069225330000039609 ) ) ;
#4187 = VERTEX_POINT ( 'NONE', #17110 ) ;
#4188 = DIRECTION ( 'NONE',  ( 0.2815395311429191305, 0.9595496299847263710, 0.000000000000000000 ) ) ;
#4189 = DIRECTION ( 'NONE',  ( 0.000000000000000000, -0.8660254037843289066, 0.5000000000001899592 ) ) ;
#4190 = FACE_OUTER_BOUND ( 'NONE', #1859, .T. ) ;
#4191 = CARTESIAN_POINT ( 'NONE',  ( 10.00000000060000005, -25.00000000000000000, -7.274962170899998526 ) ) ;
#4192 = CARTESIAN_POINT ( 'NONE',  ( -0.3076636919694037964, -28.49867017228337573, 4.240370246000018994 ) ) ;
#4193 = CARTESIAN_POINT ( 'NONE',  ( -12.42716818974678894, -22.00000000000000000, -26.94009942549494596 ) ) ;
#4194 = CARTESIAN_POINT ( 'NONE',  ( -24.41841039498785193, -14.69667350221323865, 6.099998581000020792 ) ) ;
#4195 = ORIENTED_EDGE ( 'NONE', *, *, #30349, .F. ) ;
#4196 = CARTESIAN_POINT ( 'NONE',  ( 28.35945635826399780, 7.983396865336832349, 1.000000000000000888 ) ) ;
#4197 = CARTESIAN_POINT ( 'NONE',  ( 0.6805609736260925802, -26.79155681409072898, 225.8766488246017730 ) ) ;
#4198 = CIRCLE ( 'NONE', #26331, 3.750000000000000000 ) ;
#4199 = CARTESIAN_POINT ( 'NONE',  ( 3.378474276019999945, 11.51459522689999915, 231.9999989789999972 ) ) ;
#4200 = EDGE_CURVE ( 'NONE', #7630, #30907, #2800, .T. ) ;
#4201 = CARTESIAN_POINT ( 'NONE',  ( -2.620483857012521511, -2.461162703801856644, 230.7813955785499047 ) ) ;
#4202 = FACE_OUTER_BOUND ( 'NONE', #28460, .T. ) ;
#4203 =( GEOMETRIC_REPRESENTATION_CONTEXT ( 3 ) GLOBAL_UNCERTAINTY_ASSIGNED_CONTEXT ( ( #4655 ) ) GLOBAL_UNIT_ASSIGNED_CONTEXT ( ( #10637, #22750, #17555 ) ) REPRESENTATION_CONTEXT ( 'NONE', 'WORKASPACE' ) );
#4204 = DIRECTION ( 'NONE',  ( 0.000000000000000000, 1.000000000000000000, 0.000000000000000000 ) ) ;
#4205 = DIRECTION ( 'NONE',  ( 0.000000000000000000, 0.000000000000000000, 1.000000000000000000 ) ) ;
#4206 = CARTESIAN_POINT ( 'NONE',  ( -24.24144457387483698, -14.48500828217274439, 0.000000000000000000 ) ) ;
#4207 = CARTESIAN_POINT ( 'NONE',  ( 0.7122403016127445419, -5.223333760075516530, -49.01468436622501201 ) ) ;
#4208 = EDGE_CURVE ( 'NONE', #17102, #2571, #24337, .T. ) ;
#4209 = DIRECTION ( 'NONE',  ( 0.000000000000000000, -1.000000000000000000, 2.257145581549999994E-12 ) ) ;
#4210 = CARTESIAN_POINT ( 'NONE',  ( 14.84775334008999970, -29.39779533080000107, -32.78913491209999620 ) ) ;
#4211 = CARTESIAN_POINT ( 'NONE',  ( 2.340434223344346254, -2.945736553369034283, 230.6852868990013405 ) ) ;
#4212 = CARTESIAN_POINT ( 'NONE',  ( 8.699999999974050269, -116.8589940799748632, 11.34037320843244956 ) ) ;
#4213 = ORIENTED_EDGE ( 'NONE', *, *, #30162, .F. ) ;
#4214 = CARTESIAN_POINT ( 'NONE',  ( -23.50695179570000093, -14.84192241259999889, 225.0000014190000002 ) ) ;
#4215 = VECTOR ( 'NONE', #8723, 1000.000000000000000 ) ;
#4216 = ORIENTED_EDGE ( 'NONE', *, *, #3684, .F. ) ;
#4217 = EDGE_CURVE ( 'NONE', #18284, #12444, #22763, .T. ) ;
#4218 = CARTESIAN_POINT ( 'NONE',  ( 3.599561039400463347, 4.779710538180673041, -55.10619010302499987 ) ) ;
#4219 = CIRCLE ( 'NONE', #24298, 3.199999983039998774 ) ;
#4220 = ORIENTED_EDGE ( 'NONE', *, *, #9740, .F. ) ;
#4221 = VECTOR ( 'NONE', #14826, 1000.000000000000000 ) ;
#4222 = APPLICATION_PROTOCOL_DEFINITION ( 'draft international standard', 'automotive_design', 1998, #20224 ) ;
#4223 = VECTOR ( 'NONE', #10793, 1000.000000000000000 ) ;
#4224 = VERTEX_POINT ( 'NONE', #10349 ) ;
#4225 = VECTOR ( 'NONE', #2677, 1000.000000000000000 ) ;
#4226 = PLANE ( 'NONE',  #16600 ) ;
#4227 = ORIENTED_EDGE ( 'NONE', *, *, #23844, .F. ) ;
#4228 = CARTESIAN_POINT ( 'NONE',  ( 14.40197535836999876, -32.00000000000000000, -25.51324865394999719 ) ) ;
#4229 = CARTESIAN_POINT ( 'NONE',  ( -19.29999999990000248, -27.00000000000000000, -28.39999999989999679 ) ) ;
#4230 = CARTESIAN_POINT ( 'NONE',  ( -17.38746449168248276, -28.31653965577788057, -23.38660183296255468 ) ) ;
#4231 = B_SPLINE_CURVE_WITH_KNOTS ( 'NONE', 3,
 ( #14067, #26176, #16716, #9332, #63, #11855, #217, #14220, #2723, #23826, #21302, #21458 ),
 .UNSPECIFIED., .F., .F.,
 ( 4, 2, 2, 2, 2, 4 ),
 ( 0.000000000000000000, 0.1250000000000008049, 0.2500000000000016098, 0.5000000000000011102, 0.7500000000000005551, 1.000000000000000000 ),
 .UNSPECIFIED. ) ;
#4232 = DIRECTION ( 'NONE',  ( -0.9316362575375349842, 0.3633921898465292122, -0.000000000000000000 ) ) ;
#4233 = CARTESIAN_POINT ( 'NONE',  ( 4.175165894169885483, -50.49316738903675628, -43.39999999999999858 ) ) ;
#4234 = DIRECTION ( 'NONE',  ( 5.962915006522622422E-16, 0.4383711467890810676, 0.8987940462991651502 ) ) ;
#4235 = CARTESIAN_POINT ( 'NONE',  ( -2.624260084387257219, -3.463915187244964056, -3.728945369300004753 ) ) ;
#4236 = CARTESIAN_POINT ( 'NONE',  ( -14.02695468860000005, -28.16431168439999766, 229.7625741969999922 ) ) ;
#4237 = VERTEX_POINT ( 'NONE', #29840 ) ;
#4238 = CYLINDRICAL_SURFACE ( 'NONE', #4947, 26.80000000000002203 ) ;
#4239 = CARTESIAN_POINT ( 'NONE',  ( 1.403799475828179766, 5.569137675590418723, -17.05080441500000177 ) ) ;
#4240 = CARTESIAN_POINT ( 'NONE',  ( 5.132309988016721114, -0.8582124304006011339, -34.74517599850000948 ) ) ;
#4241 = ADVANCED_FACE ( 'NONE', ( #10650 ), #14541, .F. ) ;
#4242 = CONICAL_SURFACE ( 'NONE', #12279, 4.987531172069999741, 1.047197551199999799 ) ;
#4243 = CARTESIAN_POINT ( 'NONE',  ( 8.000000000480120832, -27.30911655970313845, -25.39023929163792204 ) ) ;
#4244 = CARTESIAN_POINT ( 'NONE',  ( -6.999999999718670374, -5.981227587263883372, -27.94042817487494901 ) ) ;
#4245 = AXIS2_PLACEMENT_3D ( 'NONE', #11752, #21359, #9381 ) ;
#4246 = CARTESIAN_POINT ( 'NONE',  ( -20.08700151986557358, -19.43868425012845336, 8.000000000000007105 ) ) ;
#4247 = CARTESIAN_POINT ( 'NONE',  ( -3.510560880917136473, 0.9192256959274132111, 227.7207037332345863 ) ) ;
#4248 = AXIS2_PLACEMENT_3D ( 'NONE', #13738, #22874, #30583 ) ;
#4249 = EDGE_CURVE ( 'NONE', #24850, #24204, #4401, .T. ) ;
#4250 = AXIS2_PLACEMENT_3D ( 'NONE', #19682, #3145, #13482 ) ;
#4251 = VECTOR ( 'NONE', #18365, 1000.000000000000000 ) ;
#4252 = CARTESIAN_POINT ( 'NONE',  ( 28.40974773466432168, 5.219434544874079762, 0.7595836940000044724 ) ) ;
#4253 = CARTESIAN_POINT ( 'NONE',  ( -23.20948082139999968, -13.40000000000000036, 3.900000000369999942 ) ) ;
#4254 = CARTESIAN_POINT ( 'NONE',  ( -17.90985823243290298, 11.26838425369655816, -4.336808689942017243E-16 ) ) ;
#4255 = DIRECTION ( 'NONE',  ( 0.000000000000000000, 0.000000000000000000, 1.000000000000000000 ) ) ;
#4256 = ORIENTED_EDGE ( 'NONE', *, *, #18238, .F. ) ;
#4257 = DIRECTION ( 'NONE',  ( 0.000000000000000000, 0.000000000000000000, 1.000000000000000000 ) ) ;
#4258 = LINE ( 'NONE', #27857, #13061 ) ;
#4259 = VERTEX_POINT ( 'NONE', #27474 ) ;
#4260 = CARTESIAN_POINT ( 'NONE',  ( -6.005838698572866008, -2.164963525412170853, -44.89497819512499177 ) ) ;
#4261 = VERTEX_POINT ( 'NONE', #25285 ) ;
#4262 = ORIENTED_EDGE ( 'NONE', *, *, #7146, .T. ) ;
#4263 = SURFACE_STYLE_USAGE ( .BOTH. , #27548 ) ;
#4264 = ORIENTED_EDGE ( 'NONE', *, *, #15641, .F. ) ;
#4265 = CARTESIAN_POINT ( 'NONE',  ( -1.100001419170000050, -27.77850706310000106, 224.8959436220000043 ) ) ;
#4266 = ADVANCED_FACE ( 'NONE', ( #19941 ), #277, .T. ) ;
#4267 = VECTOR ( 'NONE', #11990, 1000.000000000000000 ) ;
#4268 = ORIENTED_EDGE ( 'NONE', *, *, #2794, .F. ) ;
#4270 = CARTESIAN_POINT ( 'NONE',  ( -25.20890834729999952, -13.29605215849999844, 225.3106485179999936 ) ) ;
#4269 = TOROIDAL_SURFACE ( 'NONE', #14319, 30.50000000000000000, 3.000000000000000000 ) ;
#4271 = CARTESIAN_POINT ( 'NONE',  ( 23.82471740507292068, 15.64077205896351508, 4.791628269000009155 ) ) ;
#4272 = DIRECTION ( 'NONE',  ( 0.1090476345695675503, 0.6986477033489619792, 0.7071067811865496822 ) ) ;
#4273 = CARTESIAN_POINT ( 'NONE',  ( 2.748504964697384700, 2.712961263263990119, -35.69999999999999574 ) ) ;
#4274 = EDGE_CURVE ( 'NONE', #22839, #9868, #3253, .T. ) ;
#4275 = CARTESIAN_POINT ( 'NONE',  ( -4.888627181016710566, 6.461915854150526606, -40.63085611776214279 ) ) ;
#4276 = CARTESIAN_POINT ( 'NONE',  ( -8.999999999710000864, 18.79791847199999921, -43.89791847198399921 ) ) ;
#4277 = CARTESIAN_POINT ( 'NONE',  ( 2.552654958872357049, -2.578671917043665385, 227.7200428341182317 ) ) ;
#4278 = B_SPLINE_CURVE_WITH_KNOTS ( 'NONE', 3,
 ( #11008, #27672, #27373, #5812, #13359, #27991 ),
 .UNSPECIFIED., .F., .F.,
 ( 4, 2, 4 ),
 ( 0.000000000000000000, 0.5000000000000000000, 1.000000000000000000 ),
 .UNSPECIFIED. ) ;
#4279 = CARTESIAN_POINT ( 'NONE',  ( 2.521631941452528558, 3.946033397249446573, -5.700967428500005596 ) ) ;
#4280 = CIRCLE ( 'NONE', #20353, 2.926829268290000119 ) ;
#4281 = CARTESIAN_POINT ( 'NONE',  ( -4.215937884789293655, -1.105999120962562809, -25.04656121680000425 ) ) ;
#4282 = CARTESIAN_POINT ( 'NONE',  ( 2.020725942159999899, -3.500000000000000000, 229.2412452703699728 ) ) ;
#4283 = ADVANCED_FACE ( 'NONE', ( #5920 ), #1216, .T. ) ;
#4284 = AXIS2_PLACEMENT_3D ( 'NONE', #12197, #4656, #22116 ) ;
#4285 = CARTESIAN_POINT ( 'NONE',  ( -3.729856948807544814, -3.301783456504468806, -94.54588698005633773 ) ) ;
#4286 = CARTESIAN_POINT ( 'NONE',  ( -7.105427357599999217E-15, -7.105427357599999217E-15, 38.33953982530000104 ) ) ;
#4287 = CYLINDRICAL_SURFACE ( 'NONE', #12133, 1.700000000000000178 ) ;
#4288 = CARTESIAN_POINT ( 'NONE',  ( -10.82908725742658440, -27.76276047461855256, 136.7828584120000244 ) ) ;
#4289 = EDGE_CURVE ( 'NONE', #29282, #2751, #10032, .T. ) ;
#4290 = CARTESIAN_POINT ( 'NONE',  ( 26.94142135619999934, 6.628004359539999533E-14, 230.0000000000000000 ) ) ;
#4291 = CARTESIAN_POINT ( 'NONE',  ( 7.338008015029190645, -6.545783030477537068, -34.28657746947716589 ) ) ;
#4292 = CARTESIAN_POINT ( 'NONE',  ( -10.00000000033029224, -25.95491900952040965, -13.51082902143504860 ) ) ;
#4293 = ORIENTED_EDGE ( 'NONE', *, *, #2074, .T. ) ;
#4294 = CARTESIAN_POINT ( 'NONE',  ( 2.637655088286918748, -3.673227524439518277, -61.12197827312499498 ) ) ;
#4295 = CARTESIAN_POINT ( 'NONE',  ( -24.83650131330000121, 13.77747940670000126, 229.0000000000000000 ) ) ;
#4296 = EDGE_LOOP ( 'NONE', ( #11783, #29685, #16860, #15548 ) ) ;
#4297 = EDGE_CURVE ( 'NONE', #29399, #11656, #16336, .T. ) ;
#4298 = CARTESIAN_POINT ( 'NONE',  ( 0.9015611980529183445, -28.48625233387473799, 3.957673652000032405 ) ) ;
#4299 = CARTESIAN_POINT ( 'NONE',  ( 2.635706879431563898, 5.544231365240147369, -32.15113063600000487 ) ) ;
#4300 = EDGE_LOOP ( 'NONE', ( #4935, #20342, #20788, #6591, #30107, #25804, #13080, #30734, #5799, #21523, #21182, #27574, #2954, #27727, #26444, #5802, #15071, #20481, #871, #15393, #21291, #28606, #1793, #8776, #11064, #971, #19175, #3351, #16677, #29558, #4953, #18099, #3664, #2977, #19896, #27432, #27891, #13604, #5453, #27234, #22171, #8121, #5191, #15132 ) ) ;
#4301 = B_SPLINE_CURVE_WITH_KNOTS ( 'NONE', 3,
 ( #27035, #10514, #12707, #20113, #19953, #5472 ),
 .UNSPECIFIED., .F., .F.,
 ( 4, 2, 4 ),
 ( 0.000000000000000000, 0.5000000000000000000, 1.000000000000000000 ),
 .UNSPECIFIED. ) ;
#4302 = DIRECTION ( 'NONE',  ( 1.000000000000000000, 0.000000000000000000, 0.000000000000000000 ) ) ;
#4303 = DIRECTION ( 'NONE',  ( 0.000000000000000000, -1.000000000000000000, 0.000000000000000000 ) ) ;
#4304 = ORIENTED_EDGE ( 'NONE', *, *, #25948, .T. ) ;
#4305 = ORIENTED_EDGE ( 'NONE', *, *, #985, .T. ) ;
#4306 = ORIENTED_EDGE ( 'NONE', *, *, #7347, .F. ) ;
#4307 = SHAPE_REPRESENTATION_RELATIONSHIP ( 'NONE' , 'NONE' ,  #20626, #26089 ) ;
#4308 = ORIENTED_EDGE ( 'NONE', *, *, #13149, .T. ) ;
#4309 = CARTESIAN_POINT ( 'NONE',  ( 24.92013865993870425, -13.82966158318416738, 6.099998581000020792 ) ) ;
#4310 = MECHANICAL_DESIGN_GEOMETRIC_PRESENTATION_REPRESENTATION (  '', ( #14357 ), #26896 ) ;
#4311 = CARTESIAN_POINT ( 'NONE',  ( 23.76736455406628323, -13.83371703039393630, 3.899999999998877698 ) ) ;
#4312 = CARTESIAN_POINT ( 'NONE',  ( 1.257215589593047023, -4.341675124665348662, -67.30367649362501936 ) ) ;
#4313 = CYLINDRICAL_SURFACE ( 'NONE', #6886, 3.000000000000005329 ) ;
#4314 = DIRECTION ( 'NONE',  ( 6.325958275728752229E-12, 0.3568421334038983650, -0.9341647027306021478 ) ) ;
#4315 = CARTESIAN_POINT ( 'NONE',  ( 26.28651405470000313, -11.41137627250000008, 222.0000000000000000 ) ) ;
#4316 = CARTESIAN_POINT ( 'NONE',  ( -17.04621913067799710, -22.00000000000000000, -25.51324865357000249 ) ) ;
#4317 = ORIENTED_EDGE ( 'NONE', *, *, #20014, .F. ) ;
#4318 = CARTESIAN_POINT ( 'NONE',  ( -19.98350515471250688, 19.99996606751605555, 0.1429766398601999555 ) ) ;
#4319 = CARTESIAN_POINT ( 'NONE',  ( -6.108812354267502798, 0.1812703649498176306, -13.18304957890000040 ) ) ;
#4320 = CYLINDRICAL_SURFACE ( 'NONE', #21877, 10.00000000000000533 ) ;
#4321 = ADVANCED_FACE ( 'NONE', ( #25917 ), #9753, .T. ) ;
#4322 = DIRECTION ( 'NONE',  ( 0.3090169943750400994, -0.9510565162951234441, 0.000000000000000000 ) ) ;
#4323 = ORIENTED_EDGE ( 'NONE', *, *, #10749, .T. ) ;
#4324 = FACE_OUTER_BOUND ( 'NONE', #28948, .T. ) ;
#4325 = CARTESIAN_POINT ( 'NONE',  ( 18.95046173579999760, -18.95046173579999760, 93.21714158839999698 ) ) ;
#4326 = CARTESIAN_POINT ( 'NONE',  ( 18.03540948931063070, 11.69027953332313352, -0.6999999999999784173 ) ) ;
#4327 = CARTESIAN_POINT ( 'NONE',  ( 0.8738980057659999634, -27.78653623639999992, 225.6801530179999986 ) ) ;
#4328 = ADVANCED_FACE ( 'NONE', ( #2151 ), #23091, .F. ) ;
#4329 = CARTESIAN_POINT ( 'NONE',  ( -23.74292845509082994, -13.87604159531000647, 3.900000000370010600 ) ) ;
#4330 = ADVANCED_FACE ( 'NONE', ( #23242, #23409 ), #11738, .T. ) ;
#4331 = DIRECTION ( 'NONE',  ( -1.000000000000000000, 0.000000000000000000, 0.000000000000000000 ) ) ;
#4332 = CARTESIAN_POINT ( 'NONE',  ( -10.00000000052381921, -26.21475634692178858, -31.32191803000645436 ) ) ;
#4334 = ADVANCED_FACE ( 'NONE', ( #18660 ), #6702, .F. ) ;
#4333 = DIRECTION ( 'NONE',  ( -3.924189347185963153E-12, 0.4082287037029530552, 0.9128796883888953273 ) ) ;
#4335 = ORIENTED_EDGE ( 'NONE', *, *, #7284, .F. ) ;
#4336 = CARTESIAN_POINT ( 'NONE',  ( 24.43008698959658176, -14.67811372800087000, 4.492876031999992748 ) ) ;
#4337 = CARTESIAN_POINT ( 'NONE',  ( 16.29938252748853245, -9.691892145436083794, -0.6999999999999783062 ) ) ;
#4338 = CARTESIAN_POINT ( 'NONE',  ( 2.811346118373302172, -3.703141056614425164, -68.10000000002500542 ) ) ;
#4339 = CARTESIAN_POINT ( 'NONE',  ( 2.484315071036837352, -2.507604248800407554, -0.6999999999999783062 ) ) ;
#4340 = CARTESIAN_POINT ( 'NONE',  ( -23.99239029816459734, 14.04409902692776591, 5.882927410969883475 ) ) ;
#4341 = ORIENTED_EDGE ( 'NONE', *, *, #1965, .T. ) ;
#4342 = CARTESIAN_POINT ( 'NONE',  ( -7.265484932596181444, 9.961462390592322080, 232.6627637660203050 ) ) ;
#4343 = CARTESIAN_POINT ( 'NONE',  ( 4.782773383985687410, -2.143867810226098847, -68.02841551502500295 ) ) ;
#4344 = EDGE_LOOP ( 'NONE', ( #19120, #1180, #8088, #14127 ) ) ;
#4345 = DIRECTION ( 'NONE',  ( 0.000000000000000000, 0.000000000000000000, 1.000000000000000000 ) ) ;
#4346 = CARTESIAN_POINT ( 'NONE',  ( -27.79539923781770483, -0.5057481688778118212, 0.8585786439999909536 ) ) ;
#4347 = ORIENTED_EDGE ( 'NONE', *, *, #25464, .F. ) ;
#4348 = CARTESIAN_POINT ( 'NONE',  ( -16.83342759559999635, 11.00000000000000355, -0.6999999999999992895 ) ) ;
#4349 = CARTESIAN_POINT ( 'NONE',  ( -26.80000000069999899, 3.281945028329999726E-15, 187.1101814799999943 ) ) ;
#4350 = DIRECTION ( 'NONE',  ( 1.000000000000000000, -1.224606353819998843E-16, 0.000000000000000000 ) ) ;
#4351 = DIRECTION ( 'NONE',  ( -1.000000000000000000, 0.000000000000000000, 0.000000000000000000 ) ) ;
#4352 = UNCERTAINTY_MEASURE_WITH_UNIT (LENGTH_MEASURE( 1.000000000000000082E-05 ), #261, 'distance_accuracy_value', 'NONE');
#4353 = DIRECTION ( 'NONE',  ( 0.3633921898465272138, -0.9316362575375356503, -1.387778780781445044E-14 ) ) ;
#4354 = DIRECTION ( 'NONE',  ( 2.256992747040000044E-12, -0.000000000000000000, -1.000000000000000000 ) ) ;
#4355 = DIRECTION ( 'NONE',  ( -1.000000000000000000, 5.687697913153403713E-16, -6.771501495041734442E-12 ) ) ;
#4356 = EDGE_LOOP ( 'NONE', ( #12880, #9635, #28055, #16249 ) ) ;
#4357 = CARTESIAN_POINT ( 'NONE',  ( 19.80526555972147307, 19.50877392102524155, 3.000000000000002665 ) ) ;
#4358 = PLANE ( 'NONE',  #6731 ) ;
#4359 = CARTESIAN_POINT ( 'NONE',  ( 11.69999999989999928, -24.11120071670000087, -0.6999999995999997005 ) ) ;
#4360 = CARTESIAN_POINT ( 'NONE',  ( -1.346291201779999946, -4.118494162357343669, -70.37733883405731206 ) ) ;
#4361 = CARTESIAN_POINT ( 'NONE',  ( 3.378474373710000034, 11.51459555979999827, 232.0000000000000000 ) ) ;
#4362 = CARTESIAN_POINT ( 'NONE',  ( -0.6521609806839999690, -27.79292263629999837, 225.9009104920000084 ) ) ;
#4363 = CARTESIAN_POINT ( 'NONE',  ( 28.50000000000000000, 8.881784197000000993E-16, 222.0000000000000000 ) ) ;
#4364 = CARTESIAN_POINT ( 'NONE',  ( 0.000000000000000000, 0.000000000000000000, 230.6412452697800006 ) ) ;
#4365 = CARTESIAN_POINT ( 'NONE',  ( 4.046071919037112607, -3.280610007121229188, -54.60923804942499515 ) ) ;
#4366 = LINE ( 'NONE', #23581, #16283 ) ;
#4367 = DIRECTION ( 'NONE',  ( -1.667070188605962886E-12, 0.4082287037029531107, 0.9128796883888953273 ) ) ;
#4368 = CARTESIAN_POINT ( 'NONE',  ( 3.109970238519766728, -1.613691810954662298, 230.8361063485526188 ) ) ;
#4369 = CARTESIAN_POINT ( 'NONE',  ( -13.88917081232333395, 20.99999999996956745, -57.58165165637253580 ) ) ;
#4370 = CARTESIAN_POINT ( 'NONE',  ( -24.64674669169999888, -14.31123007319999907, 223.9013449489999914 ) ) ;
#4371 = VERTEX_POINT ( 'NONE', #26069 ) ;
#4372 = EDGE_CURVE ( 'NONE', #409, #15021, #22825, .T. ) ;
#4373 = CARTESIAN_POINT ( 'NONE',  ( 2.097865490181829884, -3.779070126327673140, -55.58172062782499268 ) ) ;
#4374 = VERTEX_POINT ( 'NONE', #4823 ) ;
#4375 = CONTEXT_DEPENDENT_SHAPE_REPRESENTATION ( #356, #16491 ) ;
#4376 = ORIENTED_EDGE ( 'NONE', *, *, #22972, .T. ) ;
#4377 = DIRECTION ( 'NONE',  ( -1.000000000000000000, 0.000000000000000000, -6.771000000000000128E-12 ) ) ;
#4378 = PRODUCT_DEFINITION_SHAPE ( 'NONE', 'NONE',  #17 ) ;
#4379 = ORIENTED_EDGE ( 'NONE', *, *, #18564, .F. ) ;
#4380 = CARTESIAN_POINT ( 'NONE',  ( 14.40197535836999876, -27.00000000000014566, -22.62649730800000114 ) ) ;
#4381 = EDGE_CURVE ( 'NONE', #10063, #17033, #16761, .T. ) ;
#4382 = FACE_OUTER_BOUND ( 'NONE', #11513, .T. ) ;
#4383 = LINE ( 'NONE', #11156, #20990 ) ;
#4384 = AXIS2_PLACEMENT_3D ( 'NONE', #29143, #9490, #2720 ) ;
#4385 = CIRCLE ( 'NONE', #23495, 26.80000000000000071 ) ;
#4386 = CARTESIAN_POINT ( 'NONE',  ( -12.29999999969999891, -30.00000000000000000, -28.40000000020000215 ) ) ;
#4387 = CARTESIAN_POINT ( 'NONE',  ( -27.66290831536081285, -7.787312998891453120, 8.000000000000007105 ) ) ;
#4388 = CARTESIAN_POINT ( 'NONE',  ( 11.20000000009999930, -32.00000000000000000, -31.28675134584999640 ) ) ;
#4389 = CARTESIAN_POINT ( 'NONE',  ( 4.116710911288348207, -1.508563155650262111, -5.336105321700006066 ) ) ;
#4390 = CARTESIAN_POINT ( 'NONE',  ( 19.90445648569999904, -20.03186682420000153, 230.6999999999999886 ) ) ;
#4391 = VERTEX_POINT ( 'NONE', #24477 ) ;
#4392 = CARTESIAN_POINT ( 'NONE',  ( -8.881784197000000993E-16, -8.881784197000000993E-16, 227.6412452697800006 ) ) ;
#4393 = CARTESIAN_POINT ( 'NONE',  ( -4.598830142556993295, 1.338852748371190282, -17.24193125760000100 ) ) ;
#4394 = CARTESIAN_POINT ( 'NONE',  ( -3.500772897184936561, -3.093025330206538470, -33.83447003410000775 ) ) ;
#4395 = CARTESIAN_POINT ( 'NONE',  ( -0.9242233315478671773, -26.78436826004146099, 5.597929193123646563 ) ) ;
#4396 = CARTESIAN_POINT ( 'NONE',  ( 0.1059454459540000032, -28.50005195860000029, 223.9040507550000143 ) ) ;
#4397 = CARTESIAN_POINT ( 'NONE',  ( -7.999999999629061165, -18.86445920977251234, -40.99220581062246538 ) ) ;
#4398 = CARTESIAN_POINT ( 'NONE',  ( -3.676689958403109859, 0.6312712462375396072, 227.7788113689686895 ) ) ;
#4399 = B_SPLINE_SURFACE_WITH_KNOTS ( 'NONE', 5, 1, ( 
 ( #24970, #24665 ),
 ( #1217, #1060 ),
 ( #17571, #29535 ),
 ( #3406, #3099 ),
 ( #17714, #12695 ),
 ( #13008, #10813 ),
 ( #10651, #27177 ),
 ( #17870, #27475 ),
 ( #7661, #24514 ),
 ( #22307, #20242 ),
 ( #29842, #2951 ),
 ( #5616, #3254 ),
 ( #15216, #24821 ),
 ( #17417, #29377 ),
 ( #22151, #27332 ) ),
 .UNSPECIFIED., .F., .F., .F.,
 ( 6, 3, 3, 3, 6 ),
 ( 2, 2 ),
 ( 0.000000000000000000, 0.5239049114029999954, 1.047809822800000124, 1.571714734209999964, 1.746349704670000058 ),
 ( -0.7000000000009999335, 2.557514682700000071E-06 ),
 .UNSPECIFIED. ) ;
#4400 = CARTESIAN_POINT ( 'NONE',  ( 27.95444821424234405, 5.135786986018160860, -0.2432540810000105580 ) ) ;
#4401 = B_SPLINE_CURVE_WITH_KNOTS ( 'NONE', 3,
 ( #17712, #15214, #912, #27331, #5769, #757 ),
 .UNSPECIFIED., .F., .F.,
 ( 4, 2, 4 ),
 ( 0.000000000000000000, 0.5000000000000000000, 1.000000000000000000 ),
 .UNSPECIFIED. ) ;
#4402 = VECTOR ( 'NONE', #1410, 1000.000000000000000 ) ;
#4403 = CARTESIAN_POINT ( 'NONE',  ( 17.83930301670000418, 19.99998169580000251, 230.0000000000000000 ) ) ;
#4404 = CARTESIAN_POINT ( 'NONE',  ( -9.707106781189999367, 19.99999999999999645, -43.10710678118599759 ) ) ;
#4405 = EDGE_CURVE ( 'NONE', #6605, #27863, #11543, .T. ) ;
#4406 = AXIS2_PLACEMENT_3D ( 'NONE', #24968, #2948, #604 ) ;
#4407 = DIRECTION ( 'NONE',  ( 1.000000000000000000, 0.000000000000000000, 0.000000000000000000 ) ) ;
#4408 = VERTEX_POINT ( 'NONE', #7783 ) ;
#4409 = VECTOR ( 'NONE', #12848, 1000.000000000000000 ) ;
#4410 = CARTESIAN_POINT ( 'NONE',  ( 8.700000000252410715, -24.26136093482726608, -29.62468611105379779 ) ) ;
#4411 = SURFACE_STYLE_FILL_AREA ( #6344 ) ;
#4412 = CARTESIAN_POINT ( 'NONE',  ( 1.229305342267849932, -4.993942504622491896, -0.7000000457190377334 ) ) ;
#4413 = ORIENTED_EDGE ( 'NONE', *, *, #28364, .F. ) ;
#4414 = CARTESIAN_POINT ( 'NONE',  ( -1.677440080217387219, -4.586793301645948340, -44.73640794712499513 ) ) ;
#4415 = ORIENTED_EDGE ( 'NONE', *, *, #22749, .T. ) ;
#4416 = ORIENTED_EDGE ( 'NONE', *, *, #14650, .T. ) ;
#4417 = DIRECTION ( 'NONE',  ( 0.000000000000000000, 0.000000000000000000, 1.000000000000000000 ) ) ;
#4418 = ORIENTED_EDGE ( 'NONE', *, *, #30801, .F. ) ;
#4419 = CARTESIAN_POINT ( 'NONE',  ( -1.100001419170000050, -27.77850706310000106, 225.0000014190000002 ) ) ;
#4420 = ORIENTED_EDGE ( 'NONE', *, *, #23196, .T. ) ;
#4421 = CARTESIAN_POINT ( 'NONE',  ( -24.12724309970000292, -13.81083407110000039, 226.0959706989999916 ) ) ;
#4422 = DIRECTION ( 'NONE',  ( -0.3633921898465291012, -0.9316362575375348731, 0.000000000000000000 ) ) ;
#4423 = EDGE_CURVE ( 'NONE', #1748, #23469, #28453, .T. ) ;
#4424 = DIRECTION ( 'NONE',  ( 0.000000000000000000, 0.000000000000000000, -1.000000000000000000 ) ) ;
#4425 = CARTESIAN_POINT ( 'NONE',  ( 1.930846921697753960, 3.466634617185091027, -35.69999999999999574 ) ) ;
#4426 = VECTOR ( 'NONE', #26640, 1000.000000000000114 ) ;
#4427 = CARTESIAN_POINT ( 'NONE',  ( 19.95603390318983372, 20.00015565088524738, 0.1175284324535141589 ) ) ;
#4428 = FACE_OUTER_BOUND ( 'NONE', #27819, .T. ) ;
#4429 = CARTESIAN_POINT ( 'NONE',  ( -6.615393565114344732, -7.263365266400284348, -33.93658922804166878 ) ) ;
#4430 = CYLINDRICAL_SURFACE ( 'NONE', #30067, 2.999999999999998668 ) ;
#4431 = ORIENTED_EDGE ( 'NONE', *, *, #4647, .T. ) ;
#4432 = VECTOR ( 'NONE', #12645, 1000.000000000000227 ) ;
#4433 = CARTESIAN_POINT ( 'NONE',  ( 4.116710911288348207, -1.508563155650262111, -6.336105321700005177 ) ) ;
#4434 = CARTESIAN_POINT ( 'NONE',  ( 0.1332961122732720383, -6.531058726825651028, -24.41888333260000365 ) ) ;
#4435 = CARTESIAN_POINT ( 'NONE',  ( 0.000000000000000000, 0.000000000000000000, 115.0000000000000000 ) ) ;
#4436 = AXIS2_PLACEMENT_3D ( 'NONE', #793, #12274, #10383 ) ;
#4437 = CARTESIAN_POINT ( 'NONE',  ( 23.72659769746557501, -12.46160974971369662, 225.2878164648903976 ) ) ;
#4438 = EDGE_CURVE ( 'NONE', #21319, #22703, #17075, .T. ) ;
#4439 = CARTESIAN_POINT ( 'NONE',  ( 24.98081130624543889, 13.71897605842228529, 4.999998581000003384 ) ) ;
#4440 = DIRECTION ( 'NONE',  ( 0.000000000000000000, 0.3420201433259318358, -0.9396926207858125046 ) ) ;
#4441 = CARTESIAN_POINT ( 'NONE',  ( -24.66442003930000126, -14.28072947929999970, 226.1000014189999945 ) ) ;
#4442 = ADVANCED_FACE ( 'NONE', ( #28884 ), #24316, .T. ) ;
#4443 = CARTESIAN_POINT ( 'NONE',  ( 24.05407933487299132, -13.93841814072233909, 5.964141603158990002 ) ) ;
#4444 = CARTESIAN_POINT ( 'NONE',  ( 0.7646642646963620615, -28.49022165133369455, 6.079790450999988494 ) ) ;
#4445 = FACE_OUTER_BOUND ( 'NONE', #85, .T. ) ;
#4446 = ORIENTED_EDGE ( 'NONE', *, *, #1962, .T. ) ;
#4447 = CARTESIAN_POINT ( 'NONE',  ( 1.494712469390715892, 4.699749685697345747, -59.71492395752500926 ) ) ;
#4448 = CARTESIAN_POINT ( 'NONE',  ( -24.74993094845043018, 14.13250375615880117, 6.042507811999997536 ) ) ;
#4449 = CIRCLE ( 'NONE', #19522, 2.500000000105230491 ) ;
#4450 = EDGE_LOOP ( 'NONE', ( #26699, #29595, #28166, #24278 ) ) ;
#4451 = ADVANCED_FACE ( 'NONE', ( #19289 ), #29900, .T. ) ;
#4452 = CARTESIAN_POINT ( 'NONE',  ( 8.700000000241654874, -24.19757157926353486, -27.32949869323976699 ) ) ;
#4453 = CARTESIAN_POINT ( 'NONE',  ( -5.367600138795724618, 3.713494282866228069, -25.46779765530001072 ) ) ;
#4454 = ORIENTED_EDGE ( 'NONE', *, *, #13252, .F. ) ;
#4455 = CARTESIAN_POINT ( 'NONE',  ( -10.00000000000000000, 20.99999999990000887, -70.10000000019999788 ) ) ;
#4456 = CARTESIAN_POINT ( 'NONE',  ( -16.04158851046123502, 10.23646161653652875, -0.6999999999999784173 ) ) ;
#4457 = EDGE_LOOP ( 'NONE', ( #13837, #3655, #13267, #11541, #22881 ) ) ;
#4458 = VERTEX_POINT ( 'NONE', #2914 ) ;
#4459 = ORIENTED_EDGE ( 'NONE', *, *, #24318, .T. ) ;
#4460 = SURFACE_SIDE_STYLE ('',( #11386 ) ) ;
#4461 = B_SPLINE_CURVE_WITH_KNOTS ( 'NONE', 3,
 ( #19468, #7354, #28908, #7504, #17247, #24344, #4844, #14443, #5135, #12681, #2787, #26549 ),
 .UNSPECIFIED., .F., .F.,
 ( 4, 2, 2, 2, 2, 4 ),
 ( 0.000000000000000000, 0.2499999999999892308, 0.4999999999999784617, 0.6249999999999731326, 0.7499999999999676925, 1.000000000000000000 ),
 .UNSPECIFIED. ) ;
#4462 = EDGE_LOOP ( 'NONE', ( #27785, #11812, #28209, #9013 ) ) ;
#4463 = CARTESIAN_POINT ( 'NONE',  ( -12.29999999975682812, -23.88328743466139059, -29.23759322996053811 ) ) ;
#4464 = EDGE_CURVE ( 'NONE', #24086, #7025, #12321, .T. ) ;
#4465 = DIRECTION ( 'NONE',  ( 1.000000000000000000, 0.000000000000000000, 0.000000000000000000 ) ) ;
#4466 = CARTESIAN_POINT ( 'NONE',  ( -0.8291470764733299692, -4.443337602648613327, -67.90745670422499813 ) ) ;
#4467 = SURFACE_SIDE_STYLE ('',( #11547 ) ) ;
#4468 = CARTESIAN_POINT ( 'NONE',  ( 2.168672284410000206E-10, -27.14999999990000035, 230.0000000000000000 ) ) ;
#4469 = CARTESIAN_POINT ( 'NONE',  ( -26.17719569180000150, -11.91170824980000020, 222.0000000000000000 ) ) ;
#4470 = CARTESIAN_POINT ( 'NONE',  ( 3.463630677558556581, -3.438880230788124326, -0.6996960715771658457 ) ) ;
#4471 = VERTEX_POINT ( 'NONE', #2766 ) ;
#4472 = EDGE_CURVE ( 'NONE', #5752, #7991, #21293, .T. ) ;
#4473 = CARTESIAN_POINT ( 'NONE',  ( 11.14649462760000098, -24.37257236010000128, -0.7852065437999946607 ) ) ;
#4474 = CARTESIAN_POINT ( 'NONE',  ( 4.630235822890134578, 0.3309221515414850767, -14.64454535870000207 ) ) ;
#4475 = CARTESIAN_POINT ( 'NONE',  ( 23.25788685383077592, -13.43083806724684948, 136.7828584119999960 ) ) ;
#4476 = CARTESIAN_POINT ( 'NONE',  ( -10.69999999969714999, -30.19999999999998863, -28.82059031327837673 ) ) ;
#4477 = EDGE_LOOP ( 'NONE', ( #20975, #14371, #15583, #26180 ) ) ;
#4478 = CARTESIAN_POINT ( 'NONE',  ( -23.31496426210264516, -15.14116962587117143, 4.441687039633147371 ) ) ;
#4479 = CARTESIAN_POINT ( 'NONE',  ( 1.157672466085042151, -27.77645868488912484, 4.099089508000003157 ) ) ;
#4480 = CARTESIAN_POINT ( 'NONE',  ( 18.26639035964474900, 11.02001161816309072, -0.6999999999999784173 ) ) ;
#4481 = CARTESIAN_POINT ( 'NONE',  ( 2.881840510881505502, -20.28149510505218700, -27.58722306354944820 ) ) ;
#4482 = CARTESIAN_POINT ( 'NONE',  ( 11.30445670279999959, -24.42656466549999905, -1.476955110899999646 ) ) ;
#4483 = CARTESIAN_POINT ( 'NONE',  ( 3.705709820302785396, 4.685590126413917034, -63.63768011632500787 ) ) ;
#4484 = AXIS2_PLACEMENT_3D ( 'NONE', #16654, #2354, #12092 ) ;
#4485 = CARTESIAN_POINT ( 'NONE',  ( 12.70717268325767968, 20.99999999997303135, -56.04772914979974985 ) ) ;
#4486 = DIRECTION ( 'NONE',  ( -1.000000000000000000, 0.000000000000000000, 0.000000000000000000 ) ) ;
#4487 = ORIENTED_EDGE ( 'NONE', *, *, #353, .T. ) ;
#4488 = CARTESIAN_POINT ( 'NONE',  ( -10.69999999999999929, -24.73190191370000335, -30.37453596639999986 ) ) ;
#4489 = DIRECTION ( 'NONE',  ( -0.000000000000000000, -0.000000000000000000, -1.000000000000000000 ) ) ;
#4490 = CARTESIAN_POINT ( 'NONE',  ( 0.8796424051323141757, -4.905285046648036662, -68.10000000002500542 ) ) ;
#4491 = CARTESIAN_POINT ( 'NONE',  ( -7.717292505705527716, 4.672683073074085591, -39.75818898190081541 ) ) ;
#4492 = CARTESIAN_POINT ( 'NONE',  ( 10.69999999999999929, -24.87867965640000278, -30.52132034359999935 ) ) ;
#4493 = DIRECTION ( 'NONE',  ( 0.000000000000000000, 1.000000000000000000, 0.000000000000000000 ) ) ;
#4494 =( LENGTH_UNIT ( ) NAMED_UNIT ( * ) SI_UNIT ( .MILLI., .METRE. ) );
#4495 = ORIENTED_EDGE ( 'NONE', *, *, #24886, .F. ) ;
#4496 = DIRECTION ( 'NONE',  ( -1.000000000000000000, 0.000000000000000000, 0.000000000000000000 ) ) ;
#4497 = EDGE_CURVE ( 'NONE', #11846, #18237, #28383, .T. ) ;
#4498 = B_SPLINE_CURVE_WITH_KNOTS ( 'NONE', 5,
 ( #28048, #12843, #10485, #20081, #12989, #3543 ),
 .UNSPECIFIED., .F., .F.,
 ( 6, 6 ),
 ( -2.319814892689999741, 0.000000000000000000 ),
 .UNSPECIFIED. ) ;
#4499 = CARTESIAN_POINT ( 'NONE',  ( 4.441146713721671802, -1.990734395214990071, -67.27841551502500295 ) ) ;
#4500 = ORIENTED_EDGE ( 'NONE', *, *, #31039, .T. ) ;
#4501 = CARTESIAN_POINT ( 'NONE',  ( 24.83827260354858524, -12.48687744687322621, 4.852954933405435156 ) ) ;
#4502 = EDGE_CURVE ( 'NONE', #18566, #11709, #2930, .T. ) ;
#4503 = AXIS2_PLACEMENT_3D ( 'NONE', #17531, #27139, #21653 ) ;
#4504 = EDGE_CURVE ( 'NONE', #16579, #21098, #14196, .T. ) ;
#4505 = CARTESIAN_POINT ( 'NONE',  ( -24.36936511100012481, -14.56144439311391636, 0.000000000000000000 ) ) ;
#4506 = ORIENTED_EDGE ( 'NONE', *, *, #2903, .T. ) ;
#4507 = DIRECTION ( 'NONE',  ( 0.000000000000000000, 0.000000000000000000, 1.000000000000000000 ) ) ;
#4508 = PLANE ( 'NONE',  #25624 ) ;
#4509 = DIRECTION ( 'NONE',  ( 2.764802276011834743E-12, 0.9128796883888953273, -0.4082287037029531662 ) ) ;
#4510 = B_SPLINE_CURVE_WITH_KNOTS ( 'NONE', 3,
 ( #16881, #21768, #30906, #4785, #23674, #4929, #2110, #6823, #11701, #6983, #14537, #26337, #16572, #28835, #4470, #12159, #26179, #26030, #14383, #2421, #12010, #21617, #9647, #19249, #7294, #26485, #24131, #221, #21148, #30744, #9174, #15737, #6140, #23301, #4412, #14016, #22989, #8970, #25823, #18413, #16210, #25350, #11648, #30692, #20937, #20778, #25508, #3945, #23621, #18247, #11031, #30847, #1747, #28322, #23465, #13538, #2055 ),
 .UNSPECIFIED., .F., .F.,
 ( 4, 2, 2, 2, 1, 1, 1, 2, 2, 2, 2, 1, 1, 1, 2, 2, 2, 2, 2, 1, 1, 1, 2, 2, 2, 2, 2, 1, 1, 1, 1, 2, 2, 2, 4 ),
 ( 0.000000000000000000, 0.06250000000000456579, 0.09375000000000681399, 0.1093750000000078826, 0.1171875000000085071, 0.1210937500000087846, 0.1230468750000089095, 0.1240234375000090206, 0.1250000000000091316, 0.1875000000000074107, 0.2187500000000065781, 0.2343750000000061062, 0.2421875000000059952, 0.2460937500000059674, 0.2480468750000059397, 0.2500000000000058842, 0.3750000000000114353, 0.4375000000000142664, 0.4687500000000157097, 0.4843750000000163758, 0.4921875000000166533, 0.4960937500000167644, 0.4980468750000168199, 0.5000000000000168754, 0.6250000000000124345, 0.6875000000000101030, 0.7187500000000089928, 0.7343750000000083267, 0.7421875000000079936, 0.7460937500000078826, 0.7480468750000077716, 0.7490234375000077716, 0.7500000000000076605, 0.8750000000000038858, 1.000000000000000000 ),
 .UNSPECIFIED. ) ;
#4511 = CARTESIAN_POINT ( 'NONE',  ( 0.4024591535043843260, -27.79733476267318437, 3.904047916000019658 ) ) ;
#4512 = CARTESIAN_POINT ( 'NONE',  ( -10.69999999993478923, -25.95311069648830937, -13.50784318091593406 ) ) ;
#4513 = CARTESIAN_POINT ( 'NONE',  ( 6.999999999945624829, -115.1185614904238577, 21.95989595801592031 ) ) ;
#4514 = ORIENTED_EDGE ( 'NONE', *, *, #10467, .T. ) ;
#4515 = DIRECTION ( 'NONE',  ( -0.000000000000000000, 0.000000000000000000, 1.000000000000000000 ) ) ;
#4516 = CARTESIAN_POINT ( 'NONE',  ( -8.699999999650268379, -15.05691612485074948, -37.86814428179198444 ) ) ;
#4517 = CARTESIAN_POINT ( 'NONE',  ( 19.29843289230000281, 19.63498672150000246, 229.6955567279999855 ) ) ;
#4518 = CARTESIAN_POINT ( 'NONE',  ( -22.83911268609999823, 16.42879705509999866, 226.2000000000000171 ) ) ;
#4519 = CARTESIAN_POINT ( 'NONE',  ( -10.99289321870000080, 19.99999999999999645, -1.692893218799999877 ) ) ;
#4520 = CARTESIAN_POINT ( 'NONE',  ( -0.2402207101440000103, -27.79943747540000132, 226.0797932899999978 ) ) ;
#4521 = CARTESIAN_POINT ( 'NONE',  ( -24.34137756212881953, 13.42980562992878646, 3.899998581000013509 ) ) ;
#4522 = CARTESIAN_POINT ( 'NONE',  ( 1.947945353336630880, -0.5234957687185622932, 227.6412452702158475 ) ) ;
#4523 = CARTESIAN_POINT ( 'NONE',  ( 2.097865490181839654, -3.779070126327678025, -55.18172062782500120 ) ) ;
#4524 = CIRCLE ( 'NONE', #999, 3.200000000000000178 ) ;
#4525 = CARTESIAN_POINT ( 'NONE',  ( -7.999999999726708388, -29.41772009837547586, -26.57524823659570146 ) ) ;
#4526 = CARTESIAN_POINT ( 'NONE',  ( -16.09345594084761188, -8.185437083264902824, 0.000000000000000000 ) ) ;
#4527 = CARTESIAN_POINT ( 'NONE',  ( 2.874206261753454061, -2.022079741049881196, 230.8361203540554527 ) ) ;
#4528 = CARTESIAN_POINT ( 'NONE',  ( -10.69999999969999926, -27.00000000000000000, -28.40000000000000213 ) ) ;
#4529 = CARTESIAN_POINT ( 'NONE',  ( -24.09883371379999772, -15.21565466309999870, 225.0000014190000002 ) ) ;
#4530 = CARTESIAN_POINT ( 'NONE',  ( -3.985743628842677300, -2.180176701716181942, -53.74982952342499232 ) ) ;
#4531 = ORIENTED_EDGE ( 'NONE', *, *, #16998, .T. ) ;
#4532 = EDGE_CURVE ( 'NONE', #9238, #25602, #14330, .T. ) ;
#4533 = ORIENTED_EDGE ( 'NONE', *, *, #16774, .F. ) ;
#4534 = CARTESIAN_POINT ( 'NONE',  ( -17.40441589017246571, -30.57978506141823161, -32.10670460369477297 ) ) ;
#4535 = EDGE_CURVE ( 'NONE', #8375, #24893, #22444, .T. ) ;
#4536 = ORIENTED_EDGE ( 'NONE', *, *, #26507, .F. ) ;
#4537 = CARTESIAN_POINT ( 'NONE',  ( -24.49999999470000134, 3.000285566209999917E-15, 40.00000000070000539 ) ) ;
#4538 = DIRECTION ( 'NONE',  ( -1.000000000000000000, 0.000000000000000000, 0.000000000000000000 ) ) ;
#4539 = CARTESIAN_POINT ( 'NONE',  ( -27.87609112763790975, 3.928995115430390150, 1.000000000000000888 ) ) ;
#4540 = VERTEX_POINT ( 'NONE', #3683 ) ;
#4541 = CARTESIAN_POINT ( 'NONE',  ( -5.646154341209335570, 5.077040771992966661, -43.29321323052663217 ) ) ;
#4542 = LINE ( 'NONE', #7054, #16590 ) ;
#4543 = CARTESIAN_POINT ( 'NONE',  ( 8.700000000252410715, -24.26136093482726608, -29.62468611105379779 ) ) ;
#4544 = CARTESIAN_POINT ( 'NONE',  ( 4.347198243976411192, 0.5700341643805815206, -5.126979598399998395 ) ) ;
#4545 = CARTESIAN_POINT ( 'NONE',  ( -28.50000000000000000, 3.552713678799999608E-15, 229.2404163060000144 ) ) ;
#4546 = VERTEX_POINT ( 'NONE', #12658 ) ;
#4547 = DIRECTION ( 'NONE',  ( 0.000000000000000000, -2.257145581549999994E-12, -1.000000000000000000 ) ) ;
#4548 = AXIS2_PLACEMENT_3D ( 'NONE', #16178, #1866, #25790 ) ;
#4549 = CARTESIAN_POINT ( 'NONE',  ( 4.813350086082918367, -2.000601425115993148, -18.87122516810000405 ) ) ;
#4550 = CARTESIAN_POINT ( 'NONE',  ( 27.90810418749530086, 6.414199157211339042, 8.000000000000007105 ) ) ;
#4551 = CARTESIAN_POINT ( 'NONE',  ( 24.73568148353697183, -12.68911065183860920, 5.680831396999986183 ) ) ;
#4552 = B_SPLINE_CURVE_WITH_KNOTS ( 'NONE', 3,
 ( #20897, #8921, #28273, #10979, #20732, #27966, #16008, #25621, #18521, #28123 ),
 .UNSPECIFIED., .F., .F.,
 ( 4, 2, 2, 2, 4 ),
 ( 0.000000000000000000, 0.2500000000000000000, 0.5000000000000000000, 0.7500000000000000000, 1.000000000000000000 ),
 .UNSPECIFIED. ) ;
#4553 = CARTESIAN_POINT ( 'NONE',  ( -4.595673019280000382, -11.13819881049999871, 230.6412452697800006 ) ) ;
#4554 = CARTESIAN_POINT ( 'NONE',  ( -15.73360964030186970, 11.02001161816959396, -0.6999999999999784173 ) ) ;
#4555 = CARTESIAN_POINT ( 'NONE',  ( -19.79264346680938758, 19.51191464210150173, 0.8505138480000007384 ) ) ;
#4556 = CARTESIAN_POINT ( 'NONE',  ( 27.55801272791059731, 0.5014288284349612823, -0.5592437529999827461 ) ) ;
#4557 = CARTESIAN_POINT ( 'NONE',  ( 8.700000000289984214, -14.75121143964889292, -37.75136796596272148 ) ) ;
#4558 = LINE ( 'NONE', #23766, #2255 ) ;
#4559 = EDGE_CURVE ( 'NONE', #16212, #17178, #2779, .T. ) ;
#4560 = FACE_OUTER_BOUND ( 'NONE', #29563, .T. ) ;
#4561 = ORIENTED_EDGE ( 'NONE', *, *, #26132, .F. ) ;
#4562 = CARTESIAN_POINT ( 'NONE',  ( 7.638687372223567529, -9.716283825213444914, -32.74022090981047484 ) ) ;
#4563 = CARTESIAN_POINT ( 'NONE',  ( 10.87708494459999997, 19.99999999999999645, -1.827228080399999399 ) ) ;
#4564 = CARTESIAN_POINT ( 'NONE',  ( 14.47923079777919142, -26.76823368177736739, -34.03969234558647372 ) ) ;
#4565 = VERTEX_POINT ( 'NONE', #8390 ) ;
#4566 = CARTESIAN_POINT ( 'NONE',  ( 0.7190444496271986008, -5.886645524271489904, -44.26057807742500216 ) ) ;
#4567 = ORIENTED_EDGE ( 'NONE', *, *, #3884, .T. ) ;
#4568 = ORIENTED_EDGE ( 'NONE', *, *, #9104, .F. ) ;
#4569 = VERTEX_POINT ( 'NONE', #5883 ) ;
#4570 = DIRECTION ( 'NONE',  ( -0.3633921898465274913, 0.9316362575375356503, 0.000000000000000000 ) ) ;
#4571 = ORIENTED_EDGE ( 'NONE', *, *, #9036, .T. ) ;
#4572 = CARTESIAN_POINT ( 'NONE',  ( 24.09856112909999837, -15.21545593799999985, 225.1041867410000350 ) ) ;
#4573 = CARTESIAN_POINT ( 'NONE',  ( 23.78314118259453380, 14.39461387841678608, 3.901343066999990228 ) ) ;
#4574 = LINE ( 'NONE', #11966, #3913 ) ;
#4575 = CARTESIAN_POINT ( 'NONE',  ( 0.5265107913985979105, 4.688092003840730548, -35.69999999999999574 ) ) ;
#4576 = CARTESIAN_POINT ( 'NONE',  ( 20.04888805111184524, 19.99998387947535861, 0.2364017625693574376 ) ) ;
#4577 = DIRECTION ( 'NONE',  ( -1.020425574104003999E-15, 0.000000000000000000, -1.000000000000000000 ) ) ;
#4578 = CARTESIAN_POINT ( 'NONE',  ( -22.75778669576351732, -14.15360906368043281, 5.666076084815538927 ) ) ;
#4579 = DIRECTION ( 'NONE',  ( 2.612942924549014782E-24, -1.000000000000000000, 2.257145581549775024E-12 ) ) ;
#4580 = CARTESIAN_POINT ( 'NONE',  ( -5.082228009654736312, -3.365126390422853220, -6.889929326000007848 ) ) ;
#4581 = CARTESIAN_POINT ( 'NONE',  ( 3.790912472548403578, -2.108217834232220422, -26.93037294500000201 ) ) ;
#4582 = DIRECTION ( 'NONE',  ( 0.000000000000000000, 0.000000000000000000, 1.000000000000000000 ) ) ;
#4583 = FACE_BOUND ( 'NONE', #7581, .T. ) ;
#4584 = CARTESIAN_POINT ( 'NONE',  ( 24.36724935763797006, 13.38201651305720574, 5.104178997000024864 ) ) ;
#4585 = PLANE ( 'NONE',  #21690 ) ;
#4586 = CARTESIAN_POINT ( 'NONE',  ( 3.931047123110473329, -1.876836795983962469, -20.88180150029999993 ) ) ;
#4587 = EDGE_CURVE ( 'NONE', #8607, #4930, #20356, .T. ) ;
#4588 = CIRCLE ( 'NONE', #8100, 27.69999999999999929 ) ;
#4589 = CARTESIAN_POINT ( 'NONE',  ( 26.80000000069999899, -3.214342854470000215E-14, 230.0000000000000000 ) ) ;
#4590 = CARTESIAN_POINT ( 'NONE',  ( 1.607747500023186893, -28.45491842328712551, 5.310199493000017590 ) ) ;
#4591 = CARTESIAN_POINT ( 'NONE',  ( -25.66631072470286412, -7.791349473814749516, -1.399999999999998579 ) ) ;
#4592 = ORIENTED_EDGE ( 'NONE', *, *, #10403, .F. ) ;
#4593 = EDGE_CURVE ( 'NONE', #17040, #12444, #1395, .T. ) ;
#4594 = ORIENTED_EDGE ( 'NONE', *, *, #26202, .F. ) ;
#4595 = LINE ( 'NONE', #23344, #17284 ) ;
#4596 = DIRECTION ( 'NONE',  ( -0.000000000000000000, 0.000000000000000000, 1.000000000000000000 ) ) ;
#4597 = ORIENTED_EDGE ( 'NONE', *, *, #27196, .F. ) ;
#4598 = FACE_OUTER_BOUND ( 'NONE', #13478, .T. ) ;
#4599 = CARTESIAN_POINT ( 'NONE',  ( 23.87963657767028280, 15.55698410313905988, 4.493007569000006640 ) ) ;
#4600 = EDGE_LOOP ( 'NONE', ( #8740, #17630 ) ) ;
#4601 = EDGE_LOOP ( 'NONE', ( #17333, #23624, #15907, #25632, #10441, #8662, #12181, #21943 ) ) ;
#4602 = ORIENTED_EDGE ( 'NONE', *, *, #12558, .F. ) ;
#4603 = B_SPLINE_CURVE_WITH_KNOTS ( 'NONE', 5,
 ( #13439, #16117, #21309, #13603, #23209, #18320, #16268, #15962, #8714 ),
 .UNSPECIFIED., .F., .F.,
 ( 6, 3, 6 ),
 ( 8.011061266649999624, 9.405960541640000727, 10.80085981660000094 ),
 .UNSPECIFIED. ) ;
#4604 = SURFACE_STYLE_FILL_AREA ( #26781 ) ;
#4605 = VERTEX_POINT ( 'NONE', #13122 ) ;
#4606 = CARTESIAN_POINT ( 'NONE',  ( 9.999999999958941288, -28.46561708990600081, -25.75493691892357617 ) ) ;
#4607 = CARTESIAN_POINT ( 'NONE',  ( 28.50000000000000000, -1.776356839399999804E-15, 229.0000000000000000 ) ) ;
#4608 = EDGE_CURVE ( 'NONE', #25001, #9747, #10070, .T. ) ;
#4609 = CARTESIAN_POINT ( 'NONE',  ( -1.449312944839809658, 3.998683954144026220, -68.75099036452500911 ) ) ;
#4610 = ORIENTED_EDGE ( 'NONE', *, *, #26734, .F. ) ;
#4611 = EDGE_CURVE ( 'NONE', #1273, #13384, #22368, .T. ) ;
#4612 = DIRECTION ( 'NONE',  ( 1.180736691910036071E-13, -0.9986295347540310452, -0.05233595625330160483 ) ) ;
#4613 = CARTESIAN_POINT ( 'NONE',  ( 10.97739439859999955, -26.47071190269999974, 222.0000000000000000 ) ) ;
#4614 = AXIS2_PLACEMENT_3D ( 'NONE', #8039, #27246, #24896 ) ;
#4615 = CARTESIAN_POINT ( 'NONE',  ( 1.115119965759999943, -28.47834310740000063, 225.2081038119999903 ) ) ;
#4616 = ORIENTED_EDGE ( 'NONE', *, *, #17169, .F. ) ;
#4617 = CARTESIAN_POINT ( 'NONE',  ( -20.30403093138962234, 20.00000000003553424, 1.000000000000000888 ) ) ;
#4618 = B_SPLINE_CURVE_WITH_KNOTS ( 'NONE', 3,
 ( #4925, #5078, #7440, #29144 ),
 .UNSPECIFIED., .F., .F.,
 ( 4, 4 ),
 ( 0.000000000000000000, 1.000000000000000000 ),
 .UNSPECIFIED. ) ;
#4619 = PRODUCT_DEFINITION ( 'UNKNOWN', '', #6817, #30121 ) ;
#4620 = CARTESIAN_POINT ( 'NONE',  ( 1.002713911322304696, 3.977955482547951505, -17.05080441500000177 ) ) ;
#4621 = FACE_OUTER_BOUND ( 'NONE', #26466, .T. ) ;
#4622 = CARTESIAN_POINT ( 'NONE',  ( 1.100000000000000533, -27.47799119229999931, 5.097016884910053669 ) ) ;
#4623 = ORIENTED_EDGE ( 'NONE', *, *, #619, .T. ) ;
#4624 = CARTESIAN_POINT ( 'NONE',  ( 8.000000000245886866, -28.22468611110216230, -31.13863906511491209 ) ) ;
#4625 = CARTESIAN_POINT ( 'NONE',  ( -10.69999999999999929, -127.6591310166000142, -34.79037178941999997 ) ) ;
#4626 = CARTESIAN_POINT ( 'NONE',  ( -28.39963399990000070, 2.618402366230000222, 222.0000000000000000 ) ) ;
#4627 = CYLINDRICAL_SURFACE ( 'NONE', #17977, 1.099999999999999867 ) ;
#4628 = CARTESIAN_POINT ( 'NONE',  ( -5.973670867983248201, -0.3179945487330332332, -65.56421022022500722 ) ) ;
#4629 = EDGE_CURVE ( 'NONE', #3424, #13976, #8146, .T. ) ;
#4630 = AXIS2_PLACEMENT_3D ( 'NONE', #14913, #7513, #12230 ) ;
#4631 = DIRECTION ( 'NONE',  ( 0.000000000000000000, 0.000000000000000000, -1.000000000000000000 ) ) ;
#4632 = CYLINDRICAL_SURFACE ( 'NONE', #12252, 1.099999999999999867 ) ;
#4633 = VERTEX_POINT ( 'NONE', #20210 ) ;
#4634 = VECTOR ( 'NONE', #26799, 1000.000000000000000 ) ;
#4635 = CARTESIAN_POINT ( 'NONE',  ( -18.00000000000000000, 2.204291436879999808E-15, 229.6412452697800006 ) ) ;
#4636 = CARTESIAN_POINT ( 'NONE',  ( -7.999999999661569383, -18.38684431933573649, -36.12071760317176228 ) ) ;
#4637 = CARTESIAN_POINT ( 'NONE',  ( -0.9048066599225317308, -5.015669600398491745, -68.10000000002501963 ) ) ;
#4638 = CARTESIAN_POINT ( 'NONE',  ( -4.849877185155405890, 0.08414189257355281226, -68.10000000002500542 ) ) ;
#4639 = EDGE_CURVE ( 'NONE', #8738, #27983, #15328, .T. ) ;
#4640 = PLANE ( 'NONE',  #22305 ) ;
#4641 = CARTESIAN_POINT ( 'NONE',  ( -4.882699615093633483, -0.1730453822568271960, -44.10000000002499121 ) ) ;
#4642 = ORIENTED_EDGE ( 'NONE', *, *, #26958, .T. ) ;
#4643 = CYLINDRICAL_SURFACE ( 'NONE', #1921, 2.100000000000000977 ) ;
#4644 = CARTESIAN_POINT ( 'NONE',  ( 1.605176535610508326, -27.75389821387976852, 4.895940783000013674 ) ) ;
#4645 = ORIENTED_EDGE ( 'NONE', *, *, #2333, .T. ) ;
#4646 = CARTESIAN_POINT ( 'NONE',  ( -19.38902494840800017, 18.61775191683619823, 0.000000000000000000 ) ) ;
#4647 = EDGE_CURVE ( 'NONE', #7844, #24648, #28407, .T. ) ;
#4648 = CARTESIAN_POINT ( 'NONE',  ( 4.569612387855602087, -0.08076758077263379576, -58.09793411332499602 ) ) ;
#4649 = VERTEX_POINT ( 'NONE', #1964 ) ;
#4650 = CARTESIAN_POINT ( 'NONE',  ( 3.389121577680000108, 11.55088360999999963, 224.6412452697800290 ) ) ;
#4651 = AXIS2_PLACEMENT_3D ( 'NONE', #17236, #27301, #5744 ) ;
#4652 = PRODUCT_DEFINITION ( 'UNKNOWN', '', #21403, #10614 ) ;
#4653 = CARTESIAN_POINT ( 'NONE',  ( -24.40022624598054435, -14.72688605908970239, 3.899998581000013509 ) ) ;
#4654 = CARTESIAN_POINT ( 'NONE',  ( 23.66291322330000213, -14.59162663150000050, 224.2398658380000143 ) ) ;
#4655 = UNCERTAINTY_MEASURE_WITH_UNIT (LENGTH_MEASURE( 1.000000000000000082E-05 ), #10637, 'distance_accuracy_value', 'NONE');
#4656 = DIRECTION ( 'NONE',  ( 0.000000000000000000, 0.000000000000000000, 1.000000000000000000 ) ) ;
#4657 = CARTESIAN_POINT ( 'NONE',  ( -10.69999999992642259, -25.11960129118233809, -9.802886333996065460 ) ) ;
#4658 = LINE ( 'NONE', #16613, #16028 ) ;
#4659 = VERTEX_POINT ( 'NONE', #21153 ) ;
#4660 = CARTESIAN_POINT ( 'NONE',  ( -2.107992564109736122, -27.41908764619381245, 210.0000000000000284 ) ) ;
#4661 = CARTESIAN_POINT ( 'NONE',  ( 1.100000000000000089, -26.77741585740000119, 225.0000000000000000 ) ) ;
#4662 = CARTESIAN_POINT ( 'NONE',  ( 17.83931934289999788, 20.00000000000000000, 229.9999934530000019 ) ) ;
#4663 = CARTESIAN_POINT ( 'NONE',  ( -15.73632211102524181, -9.091892911704846370, 0.000000000000000000 ) ) ;
#4664 = B_SPLINE_CURVE_WITH_KNOTS ( 'NONE', 5,
 ( #20883, #18971, #30483, #28578, #16302, #18657 ),
 .UNSPECIFIED., .F., .F.,
 ( 6, 6 ),
 ( -2.300779653589999807, 0.000000000000000000 ),
 .UNSPECIFIED. ) ;
#4665 = CARTESIAN_POINT ( 'NONE',  ( 8.999999999770000869, 21.35000000040000145, -64.10000000000000853 ) ) ;
#4666 = CARTESIAN_POINT ( 'NONE',  ( -16.04158851046123502, 10.23646161653652875, -0.6999999999999784173 ) ) ;
#4667 = CARTESIAN_POINT ( 'NONE',  ( 4.276011752548591005, -110.9401521129877892, -1.050525799503824409 ) ) ;
#4668 = ADVANCED_FACE ( 'NONE', ( #20685 ), #4320, .T. ) ;
#4669 = CARTESIAN_POINT ( 'NONE',  ( 8.700000000277906764, -15.94902145836247342, -35.53273252485295330 ) ) ;
#4670 = CARTESIAN_POINT ( 'NONE',  ( 23.73489144358727998, -14.47434652104479191, 225.8865410910789251 ) ) ;
#4671 = EDGE_CURVE ( 'NONE', #28783, #13152, #4006, .T. ) ;
#4672 = CARTESIAN_POINT ( 'NONE',  ( -24.34660549313268163, -12.78643034497024367, 5.145673169883069775 ) ) ;
#4673 = CARTESIAN_POINT ( 'NONE',  ( 13.88949358619128027, 20.99999999996956745, -57.58230229939546518 ) ) ;
#4674 = CARTESIAN_POINT ( 'NONE',  ( 24.92639507930385889, 13.81781707913292934, 5.506973475999988210 ) ) ;
#4675 = ADVANCED_BREP_SHAPE_REPRESENTATION ( '', ( #10459, #17722 ), #10330 ) ;
#4676 = CIRCLE ( 'NONE', #21279, 1.700000000000000844 ) ;
#4677 = ORIENTED_EDGE ( 'NONE', *, *, #28548, .F. ) ;
#4678 = EDGE_CURVE ( 'NONE', #2824, #10568, #30410, .T. ) ;
#4679 = LINE ( 'NONE', #12376, #28318 ) ;
#4680 = B_SPLINE_CURVE_WITH_KNOTS ( 'NONE', 3,
 ( #24026, #31104, #18669, #9545 ),
 .UNSPECIFIED., .F., .F.,
 ( 4, 4 ),
 ( 0.000000000000000000, 1.000000000000000000 ),
 .UNSPECIFIED. ) ;
#4681 = EDGE_LOOP ( 'NONE', ( #29799, #13105, #7613, #8297 ) ) ;
#4682 = DIRECTION ( 'NONE',  ( 0.000000000000000000, 1.000000000000000000, 0.000000000000000000 ) ) ;
#4683 = CARTESIAN_POINT ( 'NONE',  ( -4.566814987872939824, -1.843056667269423743, -60.13491726642500623 ) ) ;
#4684 = VERTEX_POINT ( 'NONE', #1811 ) ;
#4685 = ORIENTED_EDGE ( 'NONE', *, *, #7721, .T. ) ;
#4686 = LINE ( 'NONE', #4996, #8548 ) ;
#4687 = EDGE_LOOP ( 'NONE', ( #26398, #94, #9751, #13440 ) ) ;
#4688 = PRESENTATION_STYLE_ASSIGNMENT (( #10037 ) ) ;
#4689 = AXIS2_PLACEMENT_3D ( 'NONE', #387, #547, #5243 ) ;
#4690 = CARTESIAN_POINT ( 'NONE',  ( -18.95046173579999760, -18.95046173579999760, 193.2171415880000040 ) ) ;
#4691 = CARTESIAN_POINT ( 'NONE',  ( 9.291972389019999667, 19.99999999999999645, -43.36399323947500051 ) ) ;
#4692 = PRODUCT_DEFINITION_SHAPE ( 'NONE', 'NONE',  #31131 ) ;
#4693 = CARTESIAN_POINT ( 'NONE',  ( 2.522786916459999862, -12.03261735549999933, 232.6627648150000027 ) ) ;
#4694 = DIRECTION ( 'NONE',  ( 0.000000000000000000, 0.7113488923935510355, -0.7028390664230811380 ) ) ;
#4695 = CARTESIAN_POINT ( 'NONE',  ( 8.700000000276881806, -18.45710910160467932, -35.79080037231529587 ) ) ;
#4696 = CARTESIAN_POINT ( 'NONE',  ( -1.814319851916122772, 5.833166587536846137, -4.174955258300000693 ) ) ;
#4697 = CIRCLE ( 'NONE', #12729, 27.69999999999999929 ) ;
#4698 = CARTESIAN_POINT ( 'NONE',  ( -28.35924375220000115, -10.41922902620000002, 229.7625741969999922 ) ) ;
#4699 = VERTEX_POINT ( 'NONE', #30750 ) ;
#4700 = DIRECTION ( 'NONE',  ( 1.000000000000000000, 0.000000000000000000, 0.000000000000000000 ) ) ;
#4701 = CARTESIAN_POINT ( 'NONE',  ( 4.324151835433248436, -2.064520475586355985, -21.81930150030000348 ) ) ;
#4702 = CARTESIAN_POINT ( 'NONE',  ( 1.275182700913060962, 3.500000000000000444, 230.7151724862288233 ) ) ;
#4703 = CARTESIAN_POINT ( 'NONE',  ( -8.699999999697419995, -28.90937277432163199, -30.74718652567387522 ) ) ;
#4704 = EDGE_CURVE ( 'NONE', #5374, #28074, #20846, .T. ) ;
#4705 = CARTESIAN_POINT ( 'NONE',  ( -7.428896285829999613, -9.584552481639999399, 230.6412452697800006 ) ) ;
#4706 = CARTESIAN_POINT ( 'NONE',  ( -16.06988921231594603, 11.79183908526949054, -0.6999999999999784173 ) ) ;
#4707 = CARTESIAN_POINT ( 'NONE',  ( 0.5498575204270228500, -4.501552459765379766, -43.38057807742500671 ) ) ;
#4708 = CARTESIAN_POINT ( 'NONE',  ( 24.37165445055180157, -14.77472140295711434, 4.999998581000003384 ) ) ;
#4709 = ADVANCED_FACE ( 'NONE', ( #11706 ), #28225, .T. ) ;
#4710 = DIRECTION ( 'NONE',  ( 0.8775825618903722036, 0.4794255386042040601, 0.000000000000000000 ) ) ;
#4711 = CARTESIAN_POINT ( 'NONE',  ( -24.96253706803760153, -13.75225324404262572, 5.310538869999992251 ) ) ;
#4712 = EDGE_CURVE ( 'NONE', #22821, #15775, #7446, .T. ) ;
#4713 = VECTOR ( 'NONE', #19034, 1000.000000000000114 ) ;
#4714 = VECTOR ( 'NONE', #15692, 1000.000000000000000 ) ;
#4715 = AXIS2_PLACEMENT_3D ( 'NONE', #7534, #29088, #19346 ) ;
#4716 = CARTESIAN_POINT ( 'NONE',  ( -26.95239803419980973, 3.927549058536718106E-14, 37.87317709539253485 ) ) ;
#4717 = ORIENTED_EDGE ( 'NONE', *, *, #28112, .F. ) ;
#4718 = VECTOR ( 'NONE', #2749, 1000.000000000000000 ) ;
#4719 = CARTESIAN_POINT ( 'NONE',  ( -11.69999999989999928, 19.99999999999999645, -0.6999999999999992895 ) ) ;
#4720 = DIRECTION ( 'NONE',  ( -1.000000000000000000, 0.000000000000000000, 0.000000000000000000 ) ) ;
#4721 = FACE_OUTER_BOUND ( 'NONE', #17251, .T. ) ;
#4722 = ORIENTED_EDGE ( 'NONE', *, *, #12979, .F. ) ;
#4723 = LINE ( 'NONE', #30109, #30351 ) ;
#4724 = CARTESIAN_POINT ( 'NONE',  ( 5.643028086411650435, 2.011589847869324377, -46.40627377572500478 ) ) ;
#4725 = ORIENTED_EDGE ( 'NONE', *, *, #291, .T. ) ;
#4726 = ORIENTED_EDGE ( 'NONE', *, *, #25225, .T. ) ;
#4727 = DIRECTION ( 'NONE',  ( 1.000000000000000000, 0.000000000000000000, 0.000000000000000000 ) ) ;
#4728 = B_SPLINE_CURVE_WITH_KNOTS ( 'NONE', 3,
 ( #24508, #455, #24197, #5001, #19327, #7207 ),
 .UNSPECIFIED., .F., .F.,
 ( 4, 2, 4 ),
 ( 0.000000000000000000, 0.5000000000000000000, 1.000000000000000000 ),
 .UNSPECIFIED. ) ;
#4729 = B_SPLINE_SURFACE_WITH_KNOTS ( 'NONE', 5, 1, ( 
 ( #20882, #3716 ),
 ( #13315, #25914 ),
 ( #22926, #1997 ),
 ( #30781, #1367 ),
 ( #25447, #30482 ),
 ( #20557, #11119 ),
 ( #14416, #23710 ),
 ( #21341, #415 ),
 ( #19129, #28880 ),
 ( #4962, #14106 ),
 ( #7478, #11890 ),
 ( #26216, #26522 ),
 ( #21493, #7329 ),
 ( #4653, #16914 ),
 ( #16608, #24162 ) ),
 .UNSPECIFIED., .F., .F., .F.,
 ( 6, 3, 3, 3, 6 ),
 ( 2, 2 ),
 ( 0.000000000000000000, 0.5238999883129999979, 1.047799976630000129, 1.571699964940000083, 1.746333294380000067 ),
 ( -0.7000000000009999335, 2.555882144480000001E-06 ),
 .UNSPECIFIED. ) ;
#4730 = ORIENTED_EDGE ( 'NONE', *, *, #567, .T. ) ;
#4731 = DIRECTION ( 'NONE',  ( 1.000000000000000000, -1.843431230208684678E-12, 2.650498504958264790E-12 ) ) ;
#4732 = ORIENTED_EDGE ( 'NONE', *, *, #8956, .T. ) ;
#4733 = CARTESIAN_POINT ( 'NONE',  ( 23.52644129040000109, -14.81042608839999808, 225.3105549429999996 ) ) ;
#4734 = DIRECTION ( 'NONE',  ( 0.000000000000000000, 0.3420201433259318358, -0.9396926207858125046 ) ) ;
#4735 = CARTESIAN_POINT ( 'NONE',  ( 0.3409666413401617469, 4.631268320286548779, -35.69999999999999574 ) ) ;
#4736 = CARTESIAN_POINT ( 'NONE',  ( 20.04510529260553042, 19.99998683332297489, 0.2311123248240848915 ) ) ;
#4737 = CARTESIAN_POINT ( 'NONE',  ( -2.446005382334546230, -2.858172524253452806, -0.6999999999999992895 ) ) ;
#4738 = DIRECTION ( 'NONE',  ( 0.000000000000000000, 0.000000000000000000, 1.000000000000000000 ) ) ;
#4739 = AXIS2_PLACEMENT_3D ( 'NONE', #23387, #7000, #20862 ) ;
#4740 = CARTESIAN_POINT ( 'NONE',  ( -19.49313842129999941, 19.58644462790000063, 229.5590894759999969 ) ) ;
#4741 = EDGE_CURVE ( 'NONE', #24961, #5868, #18151, .T. ) ;
#4742 = VECTOR ( 'NONE', #12840, 1000.000000000000114 ) ;
#4743 = EDGE_LOOP ( 'NONE', ( #7044, #3276, #18654, #13099, #12888, #22337, #17132 ) ) ;
#4745 = ADVANCED_FACE ( 'NONE', ( #9030 ), #23392, .F. ) ;
#4744 = CIRCLE ( 'NONE', #12775, 1.700000000000000178 ) ;
#4746 = CARTESIAN_POINT ( 'NONE',  ( -4.484282906631567478, 1.269983465873030015, -7.310827254900003069 ) ) ;
#4747 = CARTESIAN_POINT ( 'NONE',  ( 4.801822465207213675, -2.670409256638542672, -25.93037294500000201 ) ) ;
#4748 = AXIS2_PLACEMENT_3D ( 'NONE', #10840, #17737, #30020 ) ;
#4749 = FACE_OUTER_BOUND ( 'NONE', #26017, .T. ) ;
#4750 = B_SPLINE_CURVE_WITH_KNOTS ( 'NONE', 3,
 ( #16965, #26263, #24209, #17119, #28622, #19021, #19337, #311, #11296, #2198, #14000, #9581, #12243, #29080, #9729, #2042, #28928, #4702, #7524, #19178 ),
 .UNSPECIFIED., .F., .F.,
 ( 4, 1, 1, 1, 2, 2, 2, 1, 1, 1, 2, 2, 4 ),
 ( 0.000000000000000000, 0.1249999999999887590, 0.1874999999999831246, 0.2187499999999802380, 0.2343749999999805433, 0.2499999999999807931, 0.4999999999999914513, 0.6249999999999968914, 0.6875000000000003331, 0.7187500000000021094, 0.7343750000000029976, 0.7500000000000038858, 1.000000000000000000 ),
 .UNSPECIFIED. ) ;
#4751 = B_SPLINE_CURVE_WITH_KNOTS ( 'NONE', 5,
 ( #22984, #17923, #20303, #18242, #17775, #22824, #20458, #10407, #27233, #22372, #24722, #15428 ),
 .UNSPECIFIED., .F., .F.,
 ( 6, 3, 3, 6 ),
 ( 0.000000000000000000, 1.357884647149999902, 2.715789077610000213, 3.784579751189999897 ),
 .UNSPECIFIED. ) ;
#4752 = CARTESIAN_POINT ( 'NONE',  ( -17.83931601609999973, 20.00000000000000000, 230.0000000010000178 ) ) ;
#4753 = CARTESIAN_POINT ( 'NONE',  ( 9.007237960087341122, -15.62744792347586476, -74.56625543065413808 ) ) ;
#4754 = CARTESIAN_POINT ( 'NONE',  ( -8.000000000005952572, -116.8591659214701792, 11.34031266722930908 ) ) ;
#4755 = CARTESIAN_POINT ( 'NONE',  ( 4.130711734062736618, 1.221343755424965316, -17.54190840230000248 ) ) ;
#4756 = CARTESIAN_POINT ( 'NONE',  ( 23.77307027438277842, -14.41181805763364210, 5.147042609327748153 ) ) ;
#4757 = APPLICATION_CONTEXT ( 'automotive_design' ) ;
#4758 = LINE ( 'NONE', #23336, #15758 ) ;
#4759 = CARTESIAN_POINT ( 'NONE',  ( 0.9176177226984534308, -3.499836378223736943, 230.7680100055947037 ) ) ;
#4760 = VERTEX_POINT ( 'NONE', #30604 ) ;
#4761 =( GEOMETRIC_REPRESENTATION_CONTEXT ( 3 ) GLOBAL_UNCERTAINTY_ASSIGNED_CONTEXT ( ( #28579 ) ) GLOBAL_UNIT_ASSIGNED_CONTEXT ( ( #2447, #12037, #19587 ) ) REPRESENTATION_CONTEXT ( 'NONE', 'WORKASPACE' ) );
#4762 = PLANE ( 'NONE',  #15787 ) ;
#4763 = CARTESIAN_POINT ( 'NONE',  ( -5.984522419796141079, -1.167122196978044535, -31.09652066320001040 ) ) ;
#4764 = ORIENTED_EDGE ( 'NONE', *, *, #9621, .T. ) ;
#4765 = LINE ( 'NONE', #18761, #5275 ) ;
#4766 = CARTESIAN_POINT ( 'NONE',  ( -11.00000000000000000, 25.22617105830878614, -61.82510970417090590 ) ) ;
#4767 = CIRCLE ( 'NONE', #18319, 5.400000000370001274 ) ;
#4768 = ORIENTED_EDGE ( 'NONE', *, *, #8887, .T. ) ;
#4769 = CIRCLE ( 'NONE', #15317, 27.50000000000000000 ) ;
#4770 = ORIENTED_EDGE ( 'NONE', *, *, #5, .F. ) ;
#4771 = VERTEX_POINT ( 'NONE', #6668 ) ;
#4772 = AXIS2_PLACEMENT_3D ( 'NONE', #29294, #9958, #19558 ) ;
#4773 =( LENGTH_UNIT ( ) NAMED_UNIT ( * ) SI_UNIT ( .MILLI., .METRE. ) );
#4774 = ORIENTED_EDGE ( 'NONE', *, *, #25154, .F. ) ;
#4775 = CARTESIAN_POINT ( 'NONE',  ( 0.000000000000000000, 0.000000000000000000, 115.0000000000000000 ) ) ;
#4776 = CARTESIAN_POINT ( 'NONE',  ( 28.49528339128749366, 0.5184828350247757678, 0.7595836940000044724 ) ) ;
#4777 = EDGE_CURVE ( 'NONE', #10568, #6141, #24662, .T. ) ;
#4778 = CARTESIAN_POINT ( 'NONE',  ( 18.11750013295242212, -8.428624923737988439, -4.336808689942017243E-16 ) ) ;
#4779 = ORIENTED_EDGE ( 'NONE', *, *, #10749, .F. ) ;
#4780 = ADVANCED_FACE ( 'NONE', ( #25417 ), #3849, .F. ) ;
#4781 = FACE_OUTER_BOUND ( 'NONE', #28752, .T. ) ;
#4782 = CARTESIAN_POINT ( 'NONE',  ( -7.105427357599999217E-15, -7.105427357599999217E-15, 186.7828584120000244 ) ) ;
#4783 = CARTESIAN_POINT ( 'NONE',  ( -17.04621913067799710, -32.00000000058999916, -25.51324865459000080 ) ) ;
#4784 = VECTOR ( 'NONE', #11927, 1000.000000000000000 ) ;
#4785 = CARTESIAN_POINT ( 'NONE',  ( 3.750083858941618775, -2.929025673886469505, -0.7000271815399211617 ) ) ;
#4786 = ORIENTED_EDGE ( 'NONE', *, *, #28216, .F. ) ;
#4787 = EDGE_CURVE ( 'NONE', #4408, #6144, #2871, .T. ) ;
#4788 = CARTESIAN_POINT ( 'NONE',  ( 11.51411768920000078, -24.20066399999999973, -0.7084723288000027708 ) ) ;
#4789 = CARTESIAN_POINT ( 'NONE',  ( 4.190083271568243894, -3.954132654168471817, -17.43565260999999822 ) ) ;
#4790 = PLANE ( 'NONE',  #9276 ) ;
#4791 = CARTESIAN_POINT ( 'NONE',  ( -2.595987296758533791, -16.63200279366337497, -109.8342699012249994 ) ) ;
#4792 = VERTEX_POINT ( 'NONE', #11862 ) ;
#4793 = CARTESIAN_POINT ( 'NONE',  ( -23.67228571422688788, -14.57675966245750665, 3.926818800612126292 ) ) ;
#4794 = CARTESIAN_POINT ( 'NONE',  ( 0.6243462152986178904, -28.49342029039284085, 3.904048352000033528 ) ) ;
#4795 = VECTOR ( 'NONE', #4138, 999.9999999999998863 ) ;
#4796 = DIRECTION ( 'NONE',  ( 1.000000000000000000, 0.000000000000000000, 0.000000000000000000 ) ) ;
#4797 = LINE ( 'NONE', #6618, #1925 ) ;
#4798 = CARTESIAN_POINT ( 'NONE',  ( -1.100000000000000089, -17.25771824079999917, 5.000000000000000000 ) ) ;
#4799 = CARTESIAN_POINT ( 'NONE',  ( 27.09307779339999911, -1.410781934549999973E-12, 229.9751247039999953 ) ) ;
#4800 = DIRECTION ( 'NONE',  ( 0.000000000000000000, -1.000000000000000000, 0.000000000000000000 ) ) ;
#4801 = ORIENTED_EDGE ( 'NONE', *, *, #24644, .T. ) ;
#4802 = EDGE_CURVE ( 'NONE', #21281, #29484, #13803, .T. ) ;
#4803 = CARTESIAN_POINT ( 'NONE',  ( 27.50000000000000000, -1.044349611129999949E-13, 0.000000000000000000 ) ) ;
#4804 = CARTESIAN_POINT ( 'NONE',  ( -16.81341597763548990, -10.09981795544978311, -0.6999999999999784173 ) ) ;
#4805 = FACE_OUTER_BOUND ( 'NONE', #5454, .T. ) ;
#4806 = CARTESIAN_POINT ( 'NONE',  ( -9.000000000000000000, 20.99999999990000887, -67.10000000019999788 ) ) ;
#4807 = CIRCLE ( 'NONE', #2295, 3.999999999669999973 ) ;
#4808 = PRESENTATION_LAYER_ASSIGNMENT (  '', '', ( #5295 ) ) ;
#4809 = ADVANCED_FACE ( 'NONE', ( #4621 ), #25902, .T. ) ;
#4810 = ORIENTED_EDGE ( 'NONE', *, *, #21781, .F. ) ;
#4811 = CARTESIAN_POINT ( 'NONE',  ( 10.69999999997017248, -24.07790633733921126, -29.18485145324821772 ) ) ;
#4812 = VERTEX_POINT ( 'NONE', #9338 ) ;
#4813 = CARTESIAN_POINT ( 'NONE',  ( 24.06001628433582695, 15.27670955088212068, 5.888744266207340594 ) ) ;
#4814 = CARTESIAN_POINT ( 'NONE',  ( -1.895255389310859684, 5.229048247678121264, -69.63099036452499035 ) ) ;
#4815 = EDGE_LOOP ( 'NONE', ( #5174, #19426, #23159, #12950 ) ) ;
#4816 = CARTESIAN_POINT ( 'NONE',  ( -1.611722395286938170, -6.291674585240492057, -27.54882611459999353 ) ) ;
#4817 = DIRECTION ( 'NONE',  ( 0.8775825618903718706, -0.4794255386042047262, 0.000000000000000000 ) ) ;
#4818 = CARTESIAN_POINT ( 'NONE',  ( -4.848570193085766533, 0.4842359979205582143, -47.62737393802499497 ) ) ;
#4819 = CARTESIAN_POINT ( 'NONE',  ( -4.299999999899999814, -24.07317073171000033, -28.39999999989999679 ) ) ;
#4820 = CARTESIAN_POINT ( 'NONE',  ( 0.8805184772471983390, -27.48609199509227352, 224.3250316508714661 ) ) ;
#4821 = CARTESIAN_POINT ( 'NONE',  ( -11.08346179031913437, -28.41490585489481191, 193.6055512750000105 ) ) ;
#4822 = ADVANCED_FACE ( 'NONE', ( #7599, #2425, #31061 ), #4790, .T. ) ;
#4823 = CARTESIAN_POINT ( 'NONE',  ( -1.100000000000000089, -26.77741585740000119, 225.0000000000000000 ) ) ;
#4824 = CARTESIAN_POINT ( 'NONE',  ( 9.999999999959999997, -29.30501631460000311, -26.47986984960000001 ) ) ;
#4825 = EDGE_LOOP ( 'NONE', ( #14337, #9663, #15397, #16875 ) ) ;
#4826 = CARTESIAN_POINT ( 'NONE',  ( -17.83928249649999742, 19.99999999999999645, -1.399999999999998579 ) ) ;
#4827 = DIRECTION ( 'NONE',  ( 0.000000000000000000, 0.000000000000000000, 1.000000000000000000 ) ) ;
#4828 = CARTESIAN_POINT ( 'NONE',  ( -23.81776757772072983, -15.65134804123479917, 4.999998581000003384 ) ) ;
#4829 = CARTESIAN_POINT ( 'NONE',  ( -25.27355171200000328, 12.75978488059999805, 226.2000000000000171 ) ) ;
#4830 = CARTESIAN_POINT ( 'NONE',  ( -12.30489359501159008, -29.59544839336084010, -32.67501986352419152 ) ) ;
#4831 = CARTESIAN_POINT ( 'NONE',  ( -7.838355892653579460, -25.63086664713629759, 207.3305258794510166 ) ) ;
#4832 = CARTESIAN_POINT ( 'NONE',  ( 17.16657240420000008, 10.97998838177520931, -1.972246272986471594 ) ) ;
#4833 = EDGE_CURVE ( 'NONE', #10669, #15475, #26645, .T. ) ;
#4834 = CARTESIAN_POINT ( 'NONE',  ( -25.41286868644903763, 12.90211872717319430, 4.492873454000012146 ) ) ;
#4835 = CARTESIAN_POINT ( 'NONE',  ( 13.99999999979999821, 20.99999999999999645, -67.09999999999999432 ) ) ;
#4836 = ADVANCED_FACE ( 'NONE', ( #29152 ), #14226, .F. ) ;
#4837 = CARTESIAN_POINT ( 'NONE',  ( -7.999999999729645594, -28.43173360601001320, -25.75874043427127091 ) ) ;
#4838 = FACE_OUTER_BOUND ( 'NONE', #30028, .T. ) ;
#4839 = CARTESIAN_POINT ( 'NONE',  ( 24.61381495442905276, 14.36755986797187923, 6.042472827000016977 ) ) ;
#4840 = ORIENTED_EDGE ( 'NONE', *, *, #28591, .F. ) ;
#4841 = CARTESIAN_POINT ( 'NONE',  ( 10.69999999930000101, -29.06671945340000107, -26.22544931050000017 ) ) ;
#4842 = EDGE_CURVE ( 'NONE', #16921, #23754, #2879, .T. ) ;
#4843 = ORIENTED_EDGE ( 'NONE', *, *, #23886, .F. ) ;
#4844 = CARTESIAN_POINT ( 'NONE',  ( 24.22507564037507422, -15.01326821648306797, 224.3203909782756682 ) ) ;
#4845 = CARTESIAN_POINT ( 'NONE',  ( 1.169850847344618083, -6.301966510834352775, -58.74125695792500323 ) ) ;
#4846 = EDGE_LOOP ( 'NONE', ( #14823, #29844, #10226, #4995 ) ) ;
#4847 = CONTEXT_DEPENDENT_SHAPE_REPRESENTATION ( #22256, #4692 ) ;
#4848 = B_SPLINE_CURVE_WITH_KNOTS ( 'NONE', 3,
 ( #9368, #29150, #10122, #7597, #11739, #17190 ),
 .UNSPECIFIED., .F., .F.,
 ( 4, 2, 4 ),
 ( 0.000000000000000000, 0.5000000000000000000, 1.000000000000000000 ),
 .UNSPECIFIED. ) ;
#4849 = ORIENTED_EDGE ( 'NONE', *, *, #18735, .F. ) ;
#4851 = EDGE_CURVE ( 'NONE', #14446, #1273, #780, .T. ) ;
#4850 = LINE ( 'NONE', #10033, #10148 ) ;
#4852 = ORIENTED_EDGE ( 'NONE', *, *, #27429, .F. ) ;
#4853 = DIRECTION ( 'NONE',  ( 0.000000000000000000, 0.3420201433259318913, -0.9396926207858126157 ) ) ;
#4854 = CARTESIAN_POINT ( 'NONE',  ( -27.87609112763790975, 3.928995115430390150, 2.400000000000013234 ) ) ;
#4855 = CARTESIAN_POINT ( 'NONE',  ( 11.76719066729999774, -2.870640063430000222, 231.9999991140000191 ) ) ;
#4856 = FACE_OUTER_BOUND ( 'NONE', #19999, .T. ) ;
#4857 = CARTESIAN_POINT ( 'NONE',  ( -22.63992238019999803, -14.34133587289999845, 5.000000000000000000 ) ) ;
#4858 = CARTESIAN_POINT ( 'NONE',  ( -6.277996069133942925, 1.777976852108807737, -7.310827254900003069 ) ) ;
#4859 = CARTESIAN_POINT ( 'NONE',  ( 27.56257419730000180, -5.329070518199999767E-14, 230.5592437530000041 ) ) ;
#4860 = EDGE_LOOP ( 'NONE', ( #17286, #17172, #23952, #15060 ) ) ;
#4861 = CARTESIAN_POINT ( 'NONE',  ( -9.699999999996551381, -18.19238022167704116, -35.02544418635115875 ) ) ;
#4862 = ADVANCED_FACE ( 'NONE', ( #2277 ), #5084, .F. ) ;
#4863 = CARTESIAN_POINT ( 'NONE',  ( -3.665401116828205463, 4.874126016103034864, -19.63064294430000345 ) ) ;
#4864 = CARTESIAN_POINT ( 'NONE',  ( -1.100001419170000050, -27.77850706310000106, 225.0000014190000002 ) ) ;
#4865 = CARTESIAN_POINT ( 'NONE',  ( -9.130136616382021231, 21.00000000000501643, -52.40873942185827161 ) ) ;
#4866 = CARTESIAN_POINT ( 'NONE',  ( -6.339027081030000540E-10, -3.776474019031412777, -71.31703145484311790 ) ) ;
#4867 = PLANE ( 'NONE',  #17666 ) ;
#4868 = CARTESIAN_POINT ( 'NONE',  ( -1.557622931652903331, -4.259165208650873780, -43.58640794712500366 ) ) ;
#4869 = CARTESIAN_POINT ( 'NONE',  ( 10.69999999999999929, -27.00000000000000000, -25.39999999999999858 ) ) ;
#4870 = CARTESIAN_POINT ( 'NONE',  ( 13.00000000000000000, 22.40709319595134730, -62.85117013414870257 ) ) ;
#4871 = CARTESIAN_POINT ( 'NONE',  ( 8.699999999974050269, -116.8589940799748632, 11.34037320843244956 ) ) ;
#4872 = DIRECTION ( 'NONE',  ( -0.1090476345695678556, -0.6986477033489640887, -0.7071067811865475727 ) ) ;
#4873 = EDGE_LOOP ( 'NONE', ( #27142, #1559, #15542, #15942 ) ) ;
#4874 = CARTESIAN_POINT ( 'NONE',  ( 0.6752547517502489605, 4.742883336923179094, -29.94350711720000291 ) ) ;
#4875 = DIRECTION ( 'NONE',  ( 0.000000000000000000, -1.000000000000000000, 0.000000000000000000 ) ) ;
#4876 = ORIENTED_EDGE ( 'NONE', *, *, #1982, .T. ) ;
#4877 = CARTESIAN_POINT ( 'NONE',  ( 24.93720649360215802, -13.79881813812812297, 3.899998581000013509 ) ) ;
#4878 = CARTESIAN_POINT ( 'NONE',  ( 3.389692407805919849, 3.523397910813145906, -49.09426496242500093 ) ) ;
#4879 = ORIENTED_EDGE ( 'NONE', *, *, #18466, .F. ) ;
#4880 = EDGE_LOOP ( 'NONE', ( #13102, #7729, #5992, #20078, #15839, #24120 ) ) ;
#4881 = AXIS2_PLACEMENT_3D ( 'NONE', #21799, #26371, #7775 ) ;
#4882 = SHAPE_REPRESENTATION_RELATIONSHIP ( 'NONE' , 'NONE' ,  #17403, #20440 ) ;
#4883 = ORIENTED_EDGE ( 'NONE', *, *, #20470, .T. ) ;
#4884 = CARTESIAN_POINT ( 'NONE',  ( 6.000000000000000000, -17.74403716370463968, -75.33663091226621589 ) ) ;
#4885 = EDGE_CURVE ( 'NONE', #11584, #29101, #4807, .T. ) ;
#4886 = ORIENTED_EDGE ( 'NONE', *, *, #14233, .F. ) ;
#4887 = CARTESIAN_POINT ( 'NONE',  ( -8.903108651239966420, -22.82508830966961000, 190.0000000000000000 ) ) ;
#4888 = CARTESIAN_POINT ( 'NONE',  ( 24.36724935763797006, 13.38201651305720574, 4.895818164000031558 ) ) ;
#4889 = CARTESIAN_POINT ( 'NONE',  ( 9.999999999968435915, -29.93910046810518111, -27.70552897400620296 ) ) ;
#4890 = CARTESIAN_POINT ( 'NONE',  ( 1.161059139478890501, 3.931710991834906466, -35.69999999999999574 ) ) ;
#4891 = EDGE_CURVE ( 'NONE', #23146, #2707, #14136, .T. ) ;
#4892 = EDGE_CURVE ( 'NONE', #3434, #19387, #30298, .T. ) ;
#4893 = CARTESIAN_POINT ( 'NONE',  ( 19.40982886648660255, 20.00003049653962606, -0.3209631320504065521 ) ) ;
#4894 = EDGE_CURVE ( 'NONE', #28185, #16, #383, .T. ) ;
#4895 = CARTESIAN_POINT ( 'NONE',  ( 9.499999999614264112, -13.84939817494163350, -36.47165854346829406 ) ) ;
#4896 = FACE_OUTER_BOUND ( 'NONE', #14984, .T. ) ;
#4897 = CYLINDRICAL_SURFACE ( 'NONE', #24062, 1.099999999999999867 ) ;
#4898 = CARTESIAN_POINT ( 'NONE',  ( -5.003376521275985311, 3.147367150682292447, -11.44547590280000193 ) ) ;
#4899 = CARTESIAN_POINT ( 'NONE',  ( -3.878879136156900387, -1.961445906012333928, -27.46472909260000961 ) ) ;
#4900 = FACE_OUTER_BOUND ( 'NONE', #29909, .T. ) ;
#4901 = CARTESIAN_POINT ( 'NONE',  ( 24.43008698959658176, -14.67811372800087000, 5.507121129000008608 ) ) ;
#4902 = CARTESIAN_POINT ( 'NONE',  ( 24.83401022448529005, 13.98326749045440032, 5.760125282000011282 ) ) ;
#4903 = DIRECTION ( 'NONE',  ( -1.000000000000000000, 5.687697999151106851E-16, -6.771501495036750356E-12 ) ) ;
#4904 = CARTESIAN_POINT ( 'NONE',  ( -4.169787897409099386, -0.4107988151082903050, -1.146254077200002719 ) ) ;
#4905 = PRESENTATION_LAYER_ASSIGNMENT (  '', '', ( #25502 ) ) ;
#4906 = DIRECTION ( 'NONE',  ( 0.000000000000000000, 1.000000000000000000, 0.000000000000000000 ) ) ;
#4907 = CARTESIAN_POINT ( 'NONE',  ( -24.98081131316241255, -13.71897606304888662, 4.895818166000015736 ) ) ;
#4908 = DIRECTION ( 'NONE',  ( 0.7071067811870476172, -0.7071067811860475283, 1.007806864420067330E-13 ) ) ;
#4909 = ORIENTED_EDGE ( 'NONE', *, *, #29739, .T. ) ;
#4910 = DIRECTION ( 'NONE',  ( 1.000000000000000000, -1.843431230200084908E-12, 2.650498504963248473E-12 ) ) ;
#4911 = LINE ( 'NONE', #21747, #17809 ) ;
#4912 = ORIENTED_EDGE ( 'NONE', *, *, #15869, .F. ) ;
#4913 = CARTESIAN_POINT ( 'NONE',  ( -22.97554992469999746, 15.65135060219999907, 222.0000000000000000 ) ) ;
#4914 = CARTESIAN_POINT ( 'NONE',  ( 24.40022624086872938, 14.72688605419589614, 3.899998581000013509 ) ) ;
#4915 = ORIENTED_EDGE ( 'NONE', *, *, #25016, .T. ) ;
#4916 = ORIENTED_EDGE ( 'NONE', *, *, #15918, .T. ) ;
#4917 = ORIENTED_EDGE ( 'NONE', *, *, #6056, .T. ) ;
#4918 = EDGE_LOOP ( 'NONE', ( #22766, #19058, #4779, #4993 ) ) ;
#4919 = CARTESIAN_POINT ( 'NONE',  ( -17.49999999970000175, -29.40181682655888906, -30.23939095857821968 ) ) ;
#4920 = VECTOR ( 'NONE', #8697, 1000.000000000000000 ) ;
#4921 = CARTESIAN_POINT ( 'NONE',  ( 17.16657240419154462, 10.99999999996915179, -0.6999999999999784173 ) ) ;
#4922 = CARTESIAN_POINT ( 'NONE',  ( -10.00000000070000183, 19.99999999999999645, -22.39999999999999858 ) ) ;
#4923 = ORIENTED_EDGE ( 'NONE', *, *, #5389, .T. ) ;
#4924 = CARTESIAN_POINT ( 'NONE',  ( 26.79556473285982321, 0.4875557887249851730, -0.6999999999999784173 ) ) ;
#4925 = CARTESIAN_POINT ( 'NONE',  ( -12.77820031409999935, 21.69999999929999390, -56.09999999999999432 ) ) ;
#4926 = EDGE_CURVE ( 'NONE', #28330, #28642, #16417, .T. ) ;
#4927 = CARTESIAN_POINT ( 'NONE',  ( 3.441895497200000431, 11.73074891959999988, 232.6627635220000059 ) ) ;
#4928 = CARTESIAN_POINT ( 'NONE',  ( 7.499725500497901542, -7.593926722894613235, -37.11316945461116035 ) ) ;
#4929 = CARTESIAN_POINT ( 'NONE',  ( 3.658248740575405833, -3.120266197651133222, -0.6999349691374636695 ) ) ;
#4930 = VERTEX_POINT ( 'NONE', #6005 ) ;
#4931 = DIRECTION ( 'NONE',  ( 0.9316362575375356503, 0.3633921898465274913, 0.000000000000000000 ) ) ;
#4932 = CARTESIAN_POINT ( 'NONE',  ( -5.990533020055879732, -1.129328118392731950, -15.49949426529999919 ) ) ;
#4933 = CARTESIAN_POINT ( 'NONE',  ( 17.95841148951064525, -9.763538383420391042, -0.6999999999999784173 ) ) ;
#4934 = DIRECTION ( 'NONE',  ( -5.962915006522622422E-16, -0.4383711467890810676, -0.8987940462991651502 ) ) ;
#4935 = ORIENTED_EDGE ( 'NONE', *, *, #25863, .T. ) ;
#4936 = CARTESIAN_POINT ( 'NONE',  ( -12.41448843479028241, -28.30844421074986528, -33.41806619590747118 ) ) ;
#4937 = CARTESIAN_POINT ( 'NONE',  ( 23.55447120710000064, 16.04539730710000001, 222.0000000000000000 ) ) ;
#4938 = CYLINDRICAL_SURFACE ( 'NONE', #9770, 2.999999999999999112 ) ;
#4939 = TOROIDAL_SURFACE ( 'NONE', #2912, 18.16530045470000232, 1.699999999999999956 ) ;
#4940 = DIRECTION ( 'NONE',  ( -2.254051133279049930E-12, -0.05233595624287792208, 0.9986295347545773859 ) ) ;
#4941 = CARTESIAN_POINT ( 'NONE',  ( 1.415268835064556363, -5.780081730213937341, -64.70397119102500483 ) ) ;
#4942 = DIRECTION ( 'NONE',  ( 1.224606353819999829E-16, 1.000000000000000000, 0.000000000000000000 ) ) ;
#4943 = CARTESIAN_POINT ( 'NONE',  ( 8.700000000279958456, -18.28438020625039329, -36.42481760783426381 ) ) ;
#4944 = ORIENTED_EDGE ( 'NONE', *, *, #16041, .F. ) ;
#4945 = CARTESIAN_POINT ( 'NONE',  ( -12.39150945513257263, -23.44570582929690516, -24.67857000453599881 ) ) ;
#4946 = CARTESIAN_POINT ( 'NONE',  ( 0.2112796128213221825, -5.021789149852340373, -68.10000000002501963 ) ) ;
#4947 = AXIS2_PLACEMENT_3D ( 'NONE', #25805, #20922, #8627 ) ;
#4948 = CARTESIAN_POINT ( 'NONE',  ( -4.886044239781965004, -0.7344065197421389968, -68.10000000002503384 ) ) ;
#4949 = EDGE_LOOP ( 'NONE', ( #22413, #27085, #7136, #26059 ) ) ;
#4950 = EDGE_CURVE ( 'NONE', #14341, #26977, #30438, .T. ) ;
#4951 = CARTESIAN_POINT ( 'NONE',  ( 0.000000000000000000, 0.000000000000000000, 230.8412452700000017 ) ) ;
#4952 = B_SPLINE_CURVE_WITH_KNOTS ( 'NONE', 3,
 ( #21626, #21777, #2429, #9972, #78, #26495 ),
 .UNSPECIFIED., .F., .F.,
 ( 4, 2, 4 ),
 ( 0.000000000000000000, 0.5000000000000000000, 1.000000000000000000 ),
 .UNSPECIFIED. ) ;
#4953 = ORIENTED_EDGE ( 'NONE', *, *, #6593, .T. ) ;
#4954 = DIRECTION ( 'NONE',  ( -0.8090169943751909232, 0.5877852522921378498, 0.000000000000000000 ) ) ;
#4955 = CARTESIAN_POINT ( 'NONE',  ( 0.2444022557069394641, 3.892334458579130185, -69.35875473022500159 ) ) ;
#4956 = ORIENTED_EDGE ( 'NONE', *, *, #25149, .T. ) ;
#4957 = CARTESIAN_POINT ( 'NONE',  ( 3.790912472548402246, -2.108217834232220866, -27.43037294500001266 ) ) ;
#4958 = CARTESIAN_POINT ( 'NONE',  ( -9.700000000002093614, -15.94902145825307826, -35.53273252502644652 ) ) ;
#4959 = AXIS2_PLACEMENT_3D ( 'NONE', #30406, #18430, #23320 ) ;
#4960 = CARTESIAN_POINT ( 'NONE',  ( 2.752605500610148859, 3.655072764496607007, -54.62619010302499589 ) ) ;
#4961 = CARTESIAN_POINT ( 'NONE',  ( 8.000000000241653808, -24.19750966826863348, -27.32947504231146851 ) ) ;
#4962 = CARTESIAN_POINT ( 'NONE',  ( -24.21906834513991313, -15.02342241408235068, 3.957526371000025023 ) ) ;
#4963 = CARTESIAN_POINT ( 'NONE',  ( 24.07552037900000030, -13.90000980950000020, 223.9000014189999774 ) ) ;
#4964 = CARTESIAN_POINT ( 'NONE',  ( -7.999999999639610948, -13.66761481655621147, -39.85825877797649497 ) ) ;
#4965 = UNCERTAINTY_MEASURE_WITH_UNIT (LENGTH_MEASURE( 1.000000000000000082E-05 ), #4773, 'distance_accuracy_value', 'NONE');
#4966 = CARTESIAN_POINT ( 'NONE',  ( 8.700000000296645553, -12.00150950392997018, -38.75816838998848368 ) ) ;
#4967 = AXIS2_PLACEMENT_3D ( 'NONE', #10051, #5470, #7526 ) ;
#4968 = DIRECTION ( 'NONE',  ( 1.180736691910036071E-13, -0.9986295347540310452, -0.05233595625330160483 ) ) ;
#4969 = ADVANCED_FACE ( 'NONE', ( #992 ), #18850, .T. ) ;
#4970 = VERTEX_POINT ( 'NONE', #20177 ) ;
#4971 = PLANE ( 'NONE',  #450 ) ;
#4972 = PLANE ( 'NONE',  #3721 ) ;
#4973 = CARTESIAN_POINT ( 'NONE',  ( -1.870553977679999980, -12.14393525709999899, 232.6627643349999914 ) ) ;
#4974 = DIRECTION ( 'NONE',  ( 0.000000000000000000, -1.000000000000000000, 0.000000000000000000 ) ) ;
#4975 = FACE_OUTER_BOUND ( 'NONE', #18975, .T. ) ;
#4976 = CARTESIAN_POINT ( 'NONE',  ( -5.936576268373215726, -30.44659052782209585, -79.95998223598701315 ) ) ;
#4977 = CARTESIAN_POINT ( 'NONE',  ( 24.55235481438089096, -13.03932691102154351, 224.5041740165282533 ) ) ;
#4978 = CARTESIAN_POINT ( 'NONE',  ( 23.27660429769468919, -19.83288784532059168, -0.5592437529999827461 ) ) ;
#4979 = CARTESIAN_POINT ( 'NONE',  ( -0.8466629493849215926, -26.78674366432005982, 225.7036427418658775 ) ) ;
#4980 = DIRECTION ( 'NONE',  ( -1.000000000000000000, 1.224606353819999829E-16, 0.000000000000000000 ) ) ;
#4981 = CARTESIAN_POINT ( 'NONE',  ( 1.747572776708516740, 1.007237960741798055, 227.6412452701233633 ) ) ;
#4982 = AXIS2_PLACEMENT_3D ( 'NONE', #874, #12660, #8236 ) ;
#4983 = CARTESIAN_POINT ( 'NONE',  ( -1.871217229734078780, -11.95683611934309099, 232.0000002394077683 ) ) ;
#4984 = CARTESIAN_POINT ( 'NONE',  ( -16.11786738712100941, -8.163589694621649073, 0.000000000000000000 ) ) ;
#4985 = CARTESIAN_POINT ( 'NONE',  ( 7.105427357599999217E-15, 8.881784196999999612E-15, 43.60555127550000520 ) ) ;
#4986 = EDGE_CURVE ( 'NONE', #3686, #24086, #29401, .T. ) ;
#4987 = CARTESIAN_POINT ( 'NONE',  ( 19.80526555972147307, 19.50877392102524155, 1.000000000000000888 ) ) ;
#4988 = CARTESIAN_POINT ( 'NONE',  ( -24.09302906149999757, -13.87041066189999938, 223.9000014189999774 ) ) ;
#4989 = EDGE_LOOP ( 'NONE', ( #16987, #24151, #27357, #3350 ) ) ;
#4990 = FACE_OUTER_BOUND ( 'NONE', #14209, .T. ) ;
#4991 = CIRCLE ( 'NONE', #6497, 27.92857142840000151 ) ;
#4992 = CARTESIAN_POINT ( 'NONE',  ( -3.468517234904579194, -2.575357395510371461, -56.27895058492499913 ) ) ;
#4993 = ORIENTED_EDGE ( 'NONE', *, *, #16546, .F. ) ;
#4994 = ITEM_DEFINED_TRANSFORMATION ( 'NONE', 'NONE', #19876,  #17722 ) ;
#4995 = ORIENTED_EDGE ( 'NONE', *, *, #19018, .F. ) ;
#4996 = CARTESIAN_POINT ( 'NONE',  ( 2.220446049249999755E-16, 2.100000000000000089, 227.6412452697800006 ) ) ;
#4997 = VERTEX_POINT ( 'NONE', #3487 ) ;
#4998 = ORIENTED_EDGE ( 'NONE', *, *, #21912, .T. ) ;
#4999 = EDGE_CURVE ( 'NONE', #30538, #14788, #17800, .T. ) ;
#5000 = CARTESIAN_POINT ( 'NONE',  ( 1.992768273684766056, 0.6766242665914681265, 226.6412452697800006 ) ) ;
#5001 = CARTESIAN_POINT ( 'NONE',  ( -16.26054471315379857, -9.950349629747549329, -0.6999999999999784173 ) ) ;
#5002 = ADVANCED_FACE ( 'NONE', ( #22395 ), #29462, .F. ) ;
#5003 = CARTESIAN_POINT ( 'NONE',  ( 12.04114732370000063, -0.8001383763589999809, 231.9999991140000191 ) ) ;
#5004 = CARTESIAN_POINT ( 'NONE',  ( -20.30403093128963476, 20.00000000003735323, 1.800000043000016259 ) ) ;
#5005 = CARTESIAN_POINT ( 'NONE',  ( 1.604951280288046567, -4.392199147046019547, -5.760585232199999517 ) ) ;
#5006 = CYLINDRICAL_SURFACE ( 'NONE', #968, 1.099999999999999867 ) ;
#5007 = ORIENTED_EDGE ( 'NONE', *, *, #26382, .F. ) ;
#5008 = CARTESIAN_POINT ( 'NONE',  ( -2.501313136143258120, -4.446574868790201585, -44.10000000002499121 ) ) ;
#5009 = EDGE_CURVE ( 'NONE', #9711, #20581, #7798, .T. ) ;
#5010 = CARTESIAN_POINT ( 'NONE',  ( 4.190083271568243894, -3.954132654168471817, -18.03565260999999964 ) ) ;
#5011 = CARTESIAN_POINT ( 'NONE',  ( -0.8693959255619594373, -27.78669396130685953, 225.6773692761587142 ) ) ;
#5012 = CIRCLE ( 'NONE', #22110, 3.200000004570001888 ) ;
#5013 = CARTESIAN_POINT ( 'NONE',  ( 0.2182390026759475909, -27.49908342132813033, 226.0877068033350099 ) ) ;
#5014 = B_SPLINE_SURFACE_WITH_KNOTS ( 'NONE', 5, 1, ( 
 ( #4439, #16543 ),
 ( #26152, #4584 ),
 ( #14192, #23795 ),
 ( #2242, #11832 ),
 ( #12436, #14964 ),
 ( #26762, #19379 ),
 ( #4902, #5197 ),
 ( #2690, #28660 ),
 ( #655, #12291 ),
 ( #21736, #14507 ),
 ( #16691, #29120 ),
 ( #9619, #17010 ),
 ( #21903, #10242 ),
 ( #14814, #349 ),
 ( #24103, #7564 ) ),
 .UNSPECIFIED., .F., .F., .F.,
 ( 6, 3, 3, 3, 6 ),
 ( 2, 2 ),
 ( 0.000000000000000000, 0.5239010159489999596, 1.047802031900000097, 1.571703047840000034, 1.746336719830000161 ),
 ( -0.7000000000009999335, 2.556023102059999913E-06 ),
 .UNSPECIFIED. ) ;
#5015 = DIRECTION ( 'NONE',  ( -1.000000000000000000, 0.000000000000000000, 0.000000000000000000 ) ) ;
#5016 = FACE_OUTER_BOUND ( 'NONE', #28886, .T. ) ;
#5017 = LINE ( 'NONE', #26268, #7281 ) ;
#5018 = DIRECTION ( 'NONE',  ( 0.000000000000000000, 0.3420201433259318913, -0.9396926207858126157 ) ) ;
#5019 = CARTESIAN_POINT ( 'NONE',  ( 0.2196051099681128049, -26.79904497464113078, 223.9123790608769866 ) ) ;
#5020 = DIRECTION ( 'NONE',  ( 2.966217977826874882E-25, -1.000000000000000000, 2.257145581549900232E-12 ) ) ;
#5021 = EDGE_CURVE ( 'NONE', #23376, #28017, #7382, .T. ) ;
#5022 = CARTESIAN_POINT ( 'NONE',  ( -24.39135169139800041, 14.74223402946396000, 5.310643621000004977 ) ) ;
#5023 = DIRECTION ( 'NONE',  ( -1.000000000000000000, 0.000000000000000000, -6.771000000000000128E-12 ) ) ;
#5024 = VERTEX_POINT ( 'NONE', #15604 ) ;
#5025 = CARTESIAN_POINT ( 'NONE',  ( -3.231711866632715147, -5.662799918003592836, -31.27642233980000697 ) ) ;
#5026 = CYLINDRICAL_SURFACE ( 'NONE', #23253, 4.099999999999999645 ) ;
#5027 = ORIENTED_EDGE ( 'NONE', *, *, #5785, .F. ) ;
#5028 = CARTESIAN_POINT ( 'NONE',  ( 24.83272649506304219, -12.49791454618707398, 4.791562841999996714 ) ) ;
#5029 = CARTESIAN_POINT ( 'NONE',  ( 1.634888019277630278, 4.633891277622259608, -45.89079303332500359 ) ) ;
#5030 = ORIENTED_EDGE ( 'NONE', *, *, #5785, .T. ) ;
#5031 = EDGE_CURVE ( 'NONE', #26158, #6269, #13397, .T. ) ;
#5032 = ORIENTED_EDGE ( 'NONE', *, *, #1945, .F. ) ;
#5033 = DIRECTION ( 'NONE',  ( 1.000000000000000000, 0.000000000000000000, 0.000000000000000000 ) ) ;
#5034 = VERTEX_POINT ( 'NONE', #3183 ) ;
#5035 = CYLINDRICAL_SURFACE ( 'NONE', #9454, 2.500000000000002220 ) ;
#5036 = VERTEX_POINT ( 'NONE', #25207 ) ;
#5037 = DIRECTION ( 'NONE',  ( 0.6941258031311203780, 0.7198537139083029945, 0.000000000000000000 ) ) ;
#5038 =( NAMED_UNIT ( * ) SI_UNIT ( $, .STERADIAN. ) SOLID_ANGLE_UNIT ( ) );
#5039 = CARTESIAN_POINT ( 'NONE',  ( 27.75695160390876737, 2.618790587933454983, 8.000000000000007105 ) ) ;
#5040 = CARTESIAN_POINT ( 'NONE',  ( 0.3828442953759031986, 4.648648069221508194, -35.69999999999999574 ) ) ;
#5041 = CARTESIAN_POINT ( 'NONE',  ( 19.88917888186078997, 20.00030014464526218, 0.04289124618241111492 ) ) ;
#5042 = EDGE_CURVE ( 'NONE', #13946, #7965, #20023, .T. ) ;
#5043 = CARTESIAN_POINT ( 'NONE',  ( -23.92481352202500489, 14.15879617713575911, 5.760265123000013254 ) ) ;
#5044 = CARTESIAN_POINT ( 'NONE',  ( -22.63996098036293247, -14.34127493679862120, 5.145878552503609704 ) ) ;
#5045 = CYLINDRICAL_SURFACE ( 'NONE', #24551, 4.099999999999997868 ) ;
#5046 = ORIENTED_EDGE ( 'NONE', *, *, #18737, .F. ) ;
#5047 = CARTESIAN_POINT ( 'NONE',  ( -4.338779899226326009, -4.343559731693466652, -10.41399163100000713 ) ) ;
#5048 = CARTESIAN_POINT ( 'NONE',  ( 4.634019325638262465, 0.4639887426745106791, -29.63116556699998938 ) ) ;
#5049 = FACE_OUTER_BOUND ( 'NONE', #5107, .T. ) ;
#5050 = CARTESIAN_POINT ( 'NONE',  ( 23.92481352800953331, -14.15879618172764509, 5.760265122000007842 ) ) ;
#5051 = CARTESIAN_POINT ( 'NONE',  ( -10.69999999989999928, -25.00000000000000000, -14.32712675259999813 ) ) ;
#5052 = SURFACE_STYLE_USAGE ( .BOTH. , #14360 ) ;
#5053 = CARTESIAN_POINT ( 'NONE',  ( 3.453746560993067316, -19.96450010785953566, -27.74183185409264851 ) ) ;
#5054 = CARTESIAN_POINT ( 'NONE',  ( -4.278952157217901231, -0.8066629416743145153, -16.09949426530000238 ) ) ;
#5055 = CARTESIAN_POINT ( 'NONE',  ( 9.999999999966631137, -24.07798516454965920, -27.61520910695477227 ) ) ;
#5056 = CARTESIAN_POINT ( 'NONE',  ( 14.80325893430790707, -25.27741815202685416, -23.62134642851259869 ) ) ;
#5057 = CARTESIAN_POINT ( 'NONE',  ( 9.897162125334212135, -25.37356426560172906, 141.6604601749999972 ) ) ;
#5058 = EDGE_CURVE ( 'NONE', #18447, #11838, #17898, .T. ) ;
#5059 = ORIENTED_EDGE ( 'NONE', *, *, #421, .T. ) ;
#5060 = EDGE_CURVE ( 'NONE', #12690, #6489, #5392, .T. ) ;
#5061 = CARTESIAN_POINT ( 'NONE',  ( 8.000000000735305150, -25.09035620894639962, -26.05319937780492623 ) ) ;
#5062 = CARTESIAN_POINT ( 'NONE',  ( 10.69999999999999929, -24.87867965640000278, -26.27867965640000136 ) ) ;
#5063 = AXIS2_PLACEMENT_3D ( 'NONE', #14348, #25990, #23950 ) ;
#5064 = ORIENTED_EDGE ( 'NONE', *, *, #15160, .F. ) ;
#5065 = PLANE ( 'NONE',  #19363 ) ;
#5066 = FACE_OUTER_BOUND ( 'NONE', #13070, .T. ) ;
#5067 = B_SPLINE_CURVE_WITH_KNOTS ( 'NONE', 3,
 ( #28710, #5097, #21948, #28563, #29165, #24003, #28861, #9985, #24149, #21641, #9353, #9668, #89, #7612, #7315, #7005, #4948, #246, #14560, #2131, #9828, #19424, #16592, #4638, #29015, #11722, #30927, #18956, #19739, #20191, #17364, #15017, #15159, #26970, #22566, #557, #8214, #3348, #12488, #14868, #24762, #1009, #855, #24460, #2895, #5711, #25073, #10298, #5406, #17661, #10138, #29639, #29318, #22100, #27426, #24612, #3197, #10446, #22410, #7766, #19895, #3046, #3505, #5863, #5259, #12955, #20041, #29478, #20347, #17818, #15471, #7913, #15320, #5557, #13101, #8067, #10598, #17519, #27274, #12637, #24921, #29784, #22711, #22249, #1154, #10746, #12804, #29943, #705, #17208, #27124, #26812, #8532, #27581, #20503, #27900, #25865, #11381, #1631, #6024, #4139, #11221, #6342, #3830, #8849, #20822, #30431 ),
 .UNSPECIFIED., .F., .F.,
 ( 4, 2, 2, 2, 2, 2, 2, 1, 2, 2, 1, 1, 2, 2, 1, 1, 2, 2, 1, 1, 1, 2, 2, 1, 1, 1, 2, 2, 1, 1, 1, 2, 2, 1, 1, 1, 1, 2, 2, 1, 1, 1, 2, 2, 1, 1, 1, 1, 2, 2, 1, 1, 1, 2, 2, 1, 1, 1, 2, 2, 1, 1, 2, 2, 1, 2, 2, 1, 2, 2, 4 ),
 ( 0.000000000000000000, 0.06250000000000298372, 0.1250000000000060230, 0.1875000000000090761, 0.2500000000000121014, 0.2812500000000136557, 0.3125000000000152101, 0.3437500000000167644, 0.3593750000000174860, 0.3750000000000182632, 0.4062500000000197620, 0.4218750000000205391, 0.4296875000000209277, 0.4375000000000212608, 0.4531250000000220379, 0.4609375000000223155, 0.4648437500000224820, 0.4687500000000225930, 0.4843750000000232592, 0.4921875000000235367, 0.4960937500000237033, 0.4980468750000237588, 0.5000000000000238698, 0.5078125000000240918, 0.5117187500000242029, 0.5136718750000242029, 0.5146484375000240918, 0.5156250000000240918, 0.5234375000000235367, 0.5273437500000233147, 0.5292968750000232037, 0.5302734375000230926, 0.5312500000000229816, 0.5390625000000220934, 0.5429687500000215383, 0.5449218750000213163, 0.5458984375000212053, 0.5463867187500212053, 0.5468750000000212053, 0.5546875000000200950, 0.5585937500000194289, 0.5605468750000190958, 0.5615234375000189848, 0.5625000000000189848, 0.5703125000000183187, 0.5742187500000180966, 0.5761718750000179856, 0.5771484375000178746, 0.5776367187500177636, 0.5781250000000177636, 0.5859375000000174305, 0.5898437500000173195, 0.5917968750000170974, 0.5927734375000170974, 0.5937500000000169864, 0.6093750000000160982, 0.6171875000000156541, 0.6210937500000154321, 0.6230468750000153211, 0.6250000000000152101, 0.6562500000000137668, 0.6718750000000131006, 0.6796875000000127676, 0.6875000000000125455, 0.7187500000000112133, 0.7343750000000106581, 0.7500000000000099920, 0.8125000000000075495, 0.8437500000000063283, 0.8750000000000049960, 1.000000000000000000 ),
 .UNSPECIFIED. ) ;
#5068 = ORIENTED_EDGE ( 'NONE', *, *, #15083, .F. ) ;
#5069 = EDGE_LOOP ( 'NONE', ( #16550, #29713, #5334, #30585 ) ) ;
#5070 = VERTEX_POINT ( 'NONE', #3813 ) ;
#5071 = FILL_AREA_STYLE_COLOUR ( '', #1249 ) ;
#5072 = EDGE_LOOP ( 'NONE', ( #26318, #22829 ) ) ;
#5073 = CARTESIAN_POINT ( 'NONE',  ( 9.999999999959999997, -29.06670649020000141, -26.22546295170000263 ) ) ;
#5074 = CARTESIAN_POINT ( 'NONE',  ( -8.699999999649984161, -14.75061022399014909, -37.75108774327986083 ) ) ;
#5075 = CARTESIAN_POINT ( 'NONE',  ( -7.999999999682583685, -17.59928882257115390, -33.62871304529124927 ) ) ;
#5076 = ORIENTED_EDGE ( 'NONE', *, *, #18040, .T. ) ;
#5077 = CARTESIAN_POINT ( 'NONE',  ( -24.73568147689258367, 12.68911064945909217, 5.680831397999991594 ) ) ;
#5078 = CARTESIAN_POINT ( 'NONE',  ( -13.15526697139052814, 21.69999999929937928, -56.37750232931335148 ) ) ;
#5079 = CARTESIAN_POINT ( 'NONE',  ( -17.42926651579458053, -31.99974916928463031, -27.34261348416758608 ) ) ;
#5080 = DIRECTION ( 'NONE',  ( -4.428977494234582379E-12, -0.8987940462991651502, 0.4383711467890810676 ) ) ;
#5081 = ORIENTED_EDGE ( 'NONE', *, *, #19270, .F. ) ;
#5082 = CIRCLE ( 'NONE', #15611, 27.50000000000000000 ) ;
#5083 = CARTESIAN_POINT ( 'NONE',  ( 1.002713911322309359, 3.977955482547946620, -16.55080441499999466 ) ) ;
#5084 = PLANE ( 'NONE',  #8805 ) ;
#5085 = CARTESIAN_POINT ( 'NONE',  ( 26.84464184930000030, -3.287411897459999980E-15, 87.43750406040000200 ) ) ;
#5086 = LINE ( 'NONE', #27110, #4634 ) ;
#5087 = CARTESIAN_POINT ( 'NONE',  ( -10.69999999999999929, -36.62914859500000375, -26.86371135770000151 ) ) ;
#5088 = CARTESIAN_POINT ( 'NONE',  ( 27.23548387180000319, -3.335274659869999873E-15, 91.66046017409999536 ) ) ;
#5089 = CARTESIAN_POINT ( 'NONE',  ( -7.861312627709997614, 3.765626869511068620, -39.31578811131726781 ) ) ;
#5090 = DIRECTION ( 'NONE',  ( -9.220055274816719609E-13, -0.9128796883888953273, 0.4082287037029531662 ) ) ;
#5091 = CARTESIAN_POINT ( 'NONE',  ( -10.99289321870000080, -24.65831413349999934, -1.692893218799999877 ) ) ;
#5092 = CARTESIAN_POINT ( 'NONE',  ( -14.00000000000000178, 21.69999999994719886, -67.49453140416896701 ) ) ;
#5093 = VERTEX_POINT ( 'NONE', #30564 ) ;
#5094 = CARTESIAN_POINT ( 'NONE',  ( -5.212126283948660621, -2.851000302232811201, -53.34982952342500084 ) ) ;
#5095 = CARTESIAN_POINT ( 'NONE',  ( 17.83929014045347827, 20.00000000006149392, -1.000005633855494125E-09 ) ) ;
#5096 = CARTESIAN_POINT ( 'NONE',  ( -27.71261514784112379, -0.5042418800003600765, 0.5514269430000329208 ) ) ;
#5097 = CARTESIAN_POINT ( 'NONE',  ( -2.954164893002536374, -4.165023816410697854, -68.10000000002500542 ) ) ;
#5098 = EDGE_CURVE ( 'NONE', #26548, #28697, #26895, .T. ) ;
#5099 = EDGE_LOOP ( 'NONE', ( #19272, #3557 ) ) ;
#5100 = LINE ( 'NONE', #14712, #4718 ) ;
#5101 = B_SPLINE_SURFACE_WITH_KNOTS ( 'NONE', 5, 1, ( 
 ( #21847, #21688 ),
 ( #28918, #14757 ),
 ( #2640, #12232 ),
 ( #23368, #9878 ),
 ( #26707, #26410 ),
 ( #10038, #19478 ),
 ( #29069, #7514 ),
 ( #19631, #29214 ),
 ( #17258, #26868 ),
 ( #19790, #5311 ),
 ( #14914, #2947 ),
 ( #12540, #22148 ),
 ( #5459, #603 ),
 ( #10189, #29373 ),
 ( #17412, #27020 ) ),
 .UNSPECIFIED., .F., .F., .F.,
 ( 6, 3, 3, 3, 6 ),
 ( 2, 2 ),
 ( 0.000000000000000000, 0.5239055193140000899, 1.047811038630000136, 1.571716557940000092, 1.746351731040000077 ),
 ( -0.7000000000009999335, 2.557301831960000071E-06 ),
 .UNSPECIFIED. ) ;
#5102 = COLOUR_RGB ( '', 0.66274510, 0.83137255, 0.94901961) ;
#5103 =( LENGTH_UNIT ( ) NAMED_UNIT ( * ) SI_UNIT ( .MILLI., .METRE. ) );
#5104 = ORIENTED_EDGE ( 'NONE', *, *, #4986, .F. ) ;
#5105 = DIRECTION ( 'NONE',  ( 0.000000000000000000, 0.000000000000000000, 1.000000000000000000 ) ) ;
#5106 = CARTESIAN_POINT ( 'NONE',  ( -5.007939960741254026, -2.959237434304809788, -69.12382590962499762 ) ) ;
#5107 = EDGE_LOOP ( 'NONE', ( #25076, #5491, #8819, #22333, #25699, #7087, #29094, #26436 ) ) ;
#5108 = CARTESIAN_POINT ( 'NONE',  ( -5.902313038799129608, -1.548398769286710053, -25.04656121680000425 ) ) ;
#5109 = DIRECTION ( 'NONE',  ( -3.924189347185962345E-12, 0.4082287037029530552, 0.9128796883888953273 ) ) ;
#5110 = B_SPLINE_CURVE_WITH_KNOTS ( 'NONE', 3,
 ( #18658, #8906, #13472, #1214, #25759, #13791 ),
 .UNSPECIFIED., .F., .F.,
 ( 4, 2, 4 ),
 ( 0.000000000000000000, 0.5000000000000000000, 1.000000000000000000 ),
 .UNSPECIFIED. ) ;
#5111 = CARTESIAN_POINT ( 'NONE',  ( -0.5163256777700186984, 4.538631023554798638, -48.26410749632499630 ) ) ;
#5112 = CARTESIAN_POINT ( 'NONE',  ( -24.29812717100513098, -12.87956648280661831, 4.509445856313639922 ) ) ;
#5113 = CARTESIAN_POINT ( 'NONE',  ( -7.999999999648228055, -10.57732533965963384, -37.42446625050693854 ) ) ;
#5114 = CARTESIAN_POINT ( 'NONE',  ( -10.69999999999999929, -24.78546131799999941, -26.37189816670000297 ) ) ;
#5115 = CYLINDRICAL_SURFACE ( 'NONE', #25061, 2.000000000000000000 ) ;
#5116 = ORIENTED_EDGE ( 'NONE', *, *, #10597, .F. ) ;
#5117 = CARTESIAN_POINT ( 'NONE',  ( 14.81448010921107539, -31.99990471976291317, -27.51316145670302404 ) ) ;
#5118 = CARTESIAN_POINT ( 'NONE',  ( 7.105427357599999217E-15, 3.552713678799999608E-15, 41.66046017469999896 ) ) ;
#5119 = EDGE_CURVE ( 'NONE', #15021, #6694, #22852, .T. ) ;
#5120 = CARTESIAN_POINT ( 'NONE',  ( -10.70571594490000145, -5.569299341639999845, 231.9999989789999972 ) ) ;
#5121 = DIRECTION ( 'NONE',  ( 5.962915006522622422E-16, 0.4383711467890810676, 0.8987940462991651502 ) ) ;
#5122 = AXIS2_PLACEMENT_3D ( 'NONE', #314, #29084, #17122 ) ;
#5123 = CARTESIAN_POINT ( 'NONE',  ( 10.00000000070000183, -27.00000000000000000, -25.39999999999999858 ) ) ;
#5124 = CARTESIAN_POINT ( 'NONE',  ( 3.041701536937339689, -2.824850560391100718, -0.6999999999999994005 ) ) ;
#5125 = CARTESIAN_POINT ( 'NONE',  ( -20.77600556904588913, -21.68409854326813146, 1.000000000000000888 ) ) ;
#5126 = CARTESIAN_POINT ( 'NONE',  ( -21.20818545079999851, 16.99505982179999819, 230.0000000000000000 ) ) ;
#5127 = CARTESIAN_POINT ( 'NONE',  ( -11.83960380690999870, -27.00000000000000000, -28.40000000000771863 ) ) ;
#5128 = CARTESIAN_POINT ( 'NONE',  ( -3.552713678799999608E-15, 0.000000000000000000, 43.21714158840000408 ) ) ;
#5129 = CARTESIAN_POINT ( 'NONE',  ( 9.129724771679379458, 21.69999999998125872, -52.40755693945581584 ) ) ;
#5130 = CARTESIAN_POINT ( 'NONE',  ( -16.06988921231594603, 11.79183908526949054, -0.6999999989999727834 ) ) ;
#5131 = DIRECTION ( 'NONE',  ( 0.000000000000000000, 0.3420201433259318913, -0.9396926207858126157 ) ) ;
#5132 = ORIENTED_EDGE ( 'NONE', *, *, #30437, .F. ) ;
#5133 = CARTESIAN_POINT ( 'NONE',  ( 4.041451884329999800, 2.220446049249999755E-16, 230.8412452700000017 ) ) ;
#5134 = CARTESIAN_POINT ( 'NONE',  ( -24.07583586439999834, -13.90018868249999962, 223.9000014189999774 ) ) ;
#5135 = CARTESIAN_POINT ( 'NONE',  ( 24.16278207617288487, -15.11329356718511008, 224.5017226534712620 ) ) ;
#5136 = AXIS2_PLACEMENT_3D ( 'NONE', #26345, #14391, #11403 ) ;
#5137 = CARTESIAN_POINT ( 'NONE',  ( -3.552810942249358117, -4.212879106168850640, -59.97407541852498980 ) ) ;
#5138 = ORIENTED_EDGE ( 'NONE', *, *, #30018, .F. ) ;
#5139 = ORIENTED_EDGE ( 'NONE', *, *, #27706, .F. ) ;
#5140 = CARTESIAN_POINT ( 'NONE',  ( 17.18658402238548533, 9.900182044515950963, -1.000005633855494125E-09 ) ) ;
#5141 = VERTEX_POINT ( 'NONE', #13879 ) ;
#5142 = ORIENTED_EDGE ( 'NONE', *, *, #1726, .T. ) ;
#5143 = DIRECTION ( 'NONE',  ( -0.1090476345695678556, -0.6986477033489640887, -0.7071067811865475727 ) ) ;
#5144 = CARTESIAN_POINT ( 'NONE',  ( -27.07233446881492611, 8.380004974212880597, 1.000000000000000888 ) ) ;
#5145 = EDGE_CURVE ( 'NONE', #20583, #14645, #27660, .T. ) ;
#5146 = B_SPLINE_CURVE_WITH_KNOTS ( 'NONE', 5,
 ( #12288, #9616, #7562, #7408, #14190, #16851, #2687, #21587, #19530, #21900, #16689, #14504, #24101, #9457, #26457, #347, #30873, #7262, #12127, #17153, #9929 ),
 .UNSPECIFIED., .F., .F.,
 ( 6, 3, 3, 3, 3, 3, 6 ),
 ( -15.54987830269999982, -12.96130453750000022, -10.36904362289999959, -7.776782722820000160, -5.184521831719999696, -2.592260920730000251, 0.000000000000000000 ),
 .UNSPECIFIED. ) ;
#5147 = CARTESIAN_POINT ( 'NONE',  ( 6.341353821860000295, 10.26877964679999877, 231.9999991140000191 ) ) ;
#5148 = DIRECTION ( 'NONE',  ( 0.000000000000000000, 0.000000000000000000, 1.000000000000000000 ) ) ;
#5149 = CARTESIAN_POINT ( 'NONE',  ( 3.486358836775539594, -2.566383416802844319, -8.972776792899997744 ) ) ;
#5150 = DIRECTION ( 'NONE',  ( -0.000000000000000000, 1.000000000000000000, -2.257145581549999994E-12 ) ) ;
#5151 = ORIENTED_EDGE ( 'NONE', *, *, #30602, .T. ) ;
#5152 = CARTESIAN_POINT ( 'NONE',  ( 2.416185723194861357, -3.531454376423425856, -44.10000000002499121 ) ) ;
#5153 = CARTESIAN_POINT ( 'NONE',  ( -10.69999999999999929, -130.0000000000000000, -42.39999999999999858 ) ) ;
#5154 = EDGE_CURVE ( 'NONE', #18993, #29098, #13321, .T. ) ;
#5155 = CARTESIAN_POINT ( 'NONE',  ( -0.7560282158644084927, 4.289996408053712962, -19.83583244400000112 ) ) ;
#5156 = CARTESIAN_POINT ( 'NONE',  ( 12.77819780750000156, 21.69999999929999390, -56.09999999999999432 ) ) ;
#5157 = DIRECTION ( 'NONE',  ( 0.8660254037843289066, -0.5000000000001899592, 0.000000000000000000 ) ) ;
#5158 = VECTOR ( 'NONE', #13245, 1000.000000000000000 ) ;
#5159 = CARTESIAN_POINT ( 'NONE',  ( 2.247467472219999429, 11.88585404949999891, 230.6412452697800006 ) ) ;
#5160 = CARTESIAN_POINT ( 'NONE',  ( 0.000000000000000000, 0.000000000000000000, 42.06031501460000044 ) ) ;
#5161 = CARTESIAN_POINT ( 'NONE',  ( -20.15224477982290452, 20.00000015333570857, 0.3713946529999845314 ) ) ;
#5162 = B_SPLINE_SURFACE_WITH_KNOTS ( 'NONE', 5, 1, ( 
 ( #20146, #3605 ),
 ( #25019, #15115 ),
 ( #17763, #10396 ),
 ( #5819, #18075 ),
 ( #15417, #3451 ),
 ( #6126, #8320 ),
 ( #13053, #29894 ),
 ( #17915, #27524 ),
 ( #22200, #22813 ) ),
 .UNSPECIFIED., .F., .F., .F.,
 ( 6, 3, 6 ),
 ( 2, 2 ),
 ( 0.000000000000000000, 55.31395627319999875, 94.75474476520000167 ),
 ( -3.500000000000000000, 3.500000000000000000 ),
 .UNSPECIFIED. ) ;
#5163 = CARTESIAN_POINT ( 'NONE',  ( -12.29999999974999803, -27.00000000000000000, -28.40000000020000215 ) ) ;
#5164 = CARTESIAN_POINT ( 'NONE',  ( 1.100000000000000533, -26.77741585740001184, 224.9029409945208613 ) ) ;
#5165 = CARTESIAN_POINT ( 'NONE',  ( -10.69999999930000101, -24.00000000000000000, -28.40000000000000213 ) ) ;
#5166 = CARTESIAN_POINT ( 'NONE',  ( -24.37165444408190851, 14.77472139917419369, 5.104215870000011535 ) ) ;
#5167 = EDGE_CURVE ( 'NONE', #4565, #16141, #8885, .T. ) ;
#5168 = CARTESIAN_POINT ( 'NONE',  ( 8.999999999770000869, 21.21773977379998755, -43.89049139494199636 ) ) ;
#5169 = ORIENTED_EDGE ( 'NONE', *, *, #9740, .T. ) ;
#5170 = CARTESIAN_POINT ( 'NONE',  ( -4.274658871253798509, -0.8336587121505270037, -31.09652066320001040 ) ) ;
#5171 = VERTEX_POINT ( 'NONE', #23011 ) ;
#5172 = CYLINDRICAL_SURFACE ( 'NONE', #20802, 1.999999999999999778 ) ;
#5173 = CARTESIAN_POINT ( 'NONE',  ( -3.362912017748242999, 4.936852587875802278, -48.05391720692499291 ) ) ;
#5174 = ORIENTED_EDGE ( 'NONE', *, *, #7196, .F. ) ;
#5175 = TOROIDAL_SURFACE ( 'NONE', #1165, 5.792819795519999815, 3.000000000000000000 ) ;
#5176 = ORIENTED_EDGE ( 'NONE', *, *, #23818, .F. ) ;
#5177 = DIRECTION ( 'NONE',  ( -5.077529062321360589E-17, -0.9999999999999998890, 4.862478470408825645E-17 ) ) ;
#5178 = PRESENTATION_LAYER_ASSIGNMENT (  '', '', ( #18750 ) ) ;
#5179 = ORIENTED_EDGE ( 'NONE', *, *, #5805, .T. ) ;
#5180 = CARTESIAN_POINT ( 'NONE',  ( -8.000000000477658801, -25.77531388886969310, -25.66136093485691916 ) ) ;
#5181 = ORIENTED_EDGE ( 'NONE', *, *, #23655, .F. ) ;
#5182 = AXIS2_PLACEMENT_3D ( 'NONE', #12295, #2850, #10699 ) ;
#5183 = FACE_OUTER_BOUND ( 'NONE', #18417, .T. ) ;
#5184 = CARTESIAN_POINT ( 'NONE',  ( 2.605043309139144281, 2.487932632647766873, 227.7052921205562370 ) ) ;
#5185 = CARTESIAN_POINT ( 'NONE',  ( 23.80322556508107112, 14.59355840047072661, 1.000000000000000888 ) ) ;
#5186 = CARTESIAN_POINT ( 'NONE',  ( 0.4316393286370151516, 4.665185289904927757, -35.69999999999999574 ) ) ;
#5187 = CARTESIAN_POINT ( 'NONE',  ( -21.70990266010000269, 18.50700188859999784, 225.0000000000000000 ) ) ;
#5188 = LINE ( 'NONE', #19055, #14946 ) ;
#5189 = FACE_OUTER_BOUND ( 'NONE', #21412, .T. ) ;
#5190 = DIRECTION ( 'NONE',  ( -1.000000000000000000, 5.687697999151106851E-16, -6.771501495036750356E-12 ) ) ;
#5191 = ORIENTED_EDGE ( 'NONE', *, *, #22922, .F. ) ;
#5192 = ADVANCED_FACE ( 'NONE', ( #30409 ), #25690, .T. ) ;
#5193 = CARTESIAN_POINT ( 'NONE',  ( 4.262818619062177738, -0.7545854518158021662, -8.771482634699998115 ) ) ;
#5194 = CARTESIAN_POINT ( 'NONE',  ( -3.878879136156893281, -1.961445906012333706, -27.96472909260000606 ) ) ;
#5195 = CARTESIAN_POINT ( 'NONE',  ( -27.79539923781770128, -0.5057481688779147389, 8.000000000000007105 ) ) ;
#5196 = CARTESIAN_POINT ( 'NONE',  ( 23.79228474585360686, -14.38012950158411662, 5.310643619999999565 ) ) ;
#5197 = CARTESIAN_POINT ( 'NONE',  ( 24.22405392119105016, 13.63981656816893739, 5.760125282000011282 ) ) ;
#5198 =( LENGTH_UNIT ( ) NAMED_UNIT ( * ) SI_UNIT ( .MILLI., .METRE. ) );
#5199 = VECTOR ( 'NONE', #14128, 1000.000000000000000 ) ;
#5200 = LINE ( 'NONE', #30611, #10649 ) ;
#5201 = CARTESIAN_POINT ( 'NONE',  ( 1.002713911322304696, 3.977955482547951505, -17.05080441500000177 ) ) ;
#5202 = VECTOR ( 'NONE', #26615, 1000.000000000000000 ) ;
#5203 = CIRCLE ( 'NONE', #7232, 1.100000000390000787 ) ;
#5204 = DIRECTION ( 'NONE',  ( 1.000000000000000000, 0.000000000000000000, 0.000000000000000000 ) ) ;
#5205 = CARTESIAN_POINT ( 'NONE',  ( -24.96253706803760153, -13.75225324404262572, 4.689458291000009105 ) ) ;
#5206 = DIRECTION ( 'NONE',  ( -0.000000000000000000, 1.000000000000000000, 0.000000000000000000 ) ) ;
#5207 = VERTEX_POINT ( 'NONE', #6631 ) ;
#5208 = ADVANCED_FACE ( 'NONE', ( #16230 ), #20643, .F. ) ;
#5209 = EDGE_CURVE ( 'NONE', #20042, #24964, #25845, .T. ) ;
#5210 = CARTESIAN_POINT ( 'NONE',  ( 1.645560275461343203, -28.45273235261698019, 4.895940783000013674 ) ) ;
#5211 = LINE ( 'NONE', #7422, #16325 ) ;
#5212 = ORIENTED_EDGE ( 'NONE', *, *, #10971, .T. ) ;
#5213 = EDGE_CURVE ( 'NONE', #13677, #6141, #1924, .T. ) ;
#5214 = CARTESIAN_POINT ( 'NONE',  ( -7.999999999652283478, -16.96959321758620476, -37.81493174591201978 ) ) ;
#5215 = DIRECTION ( 'NONE',  ( 0.8366600265365546907, 0.4922897737059920287, -0.2401057656541278063 ) ) ;
#5216 = ORIENTED_EDGE ( 'NONE', *, *, #14280, .F. ) ;
#5217 = PLANE ( 'NONE',  #7957 ) ;
#5218 = ORIENTED_EDGE ( 'NONE', *, *, #19252, .F. ) ;
#5219 = ORIENTED_EDGE ( 'NONE', *, *, #27942, .T. ) ;
#5220 = ADVANCED_FACE ( 'NONE', ( #9141 ), #6791, .T. ) ;
#5221 = ORIENTED_EDGE ( 'NONE', *, *, #26186, .F. ) ;
#5222 = CARTESIAN_POINT ( 'NONE',  ( 27.23548387100000312, -3.552713678799999608E-15, 38.33953982530000104 ) ) ;
#5223 = VECTOR ( 'NONE', #10015, 1000.000000000000000 ) ;
#5224 = CARTESIAN_POINT ( 'NONE',  ( -28.50000000000000000, -5.472165930259999123E-14, 229.0000000000000000 ) ) ;
#5225 = CARTESIAN_POINT ( 'NONE',  ( -7.999999999719186405, -5.927479909175757733, -27.82023779336357094 ) ) ;
#5226 = CIRCLE ( 'NONE', #9239, 4.000000000000000888 ) ;
#5227 = ORIENTED_EDGE ( 'NONE', *, *, #16542, .F. ) ;
#5228 = CARTESIAN_POINT ( 'NONE',  ( -25.35851007062240114, 13.00862288638852959, 5.680831397999991594 ) ) ;
#5229 = B_SPLINE_CURVE_WITH_KNOTS ( 'NONE', 5,
 ( #23713, #26072, #29301, #21188, #24596, #7895 ),
 .UNSPECIFIED., .F., .F.,
 ( 6, 6 ),
 ( 0.000000000000000000, 2.319814960350000010 ),
 .UNSPECIFIED. ) ;
#5230 = VECTOR ( 'NONE', #11561, 1000.000000000000000 ) ;
#5231 = DIRECTION ( 'NONE',  ( 0.3633921898465272138, -0.9316362575375356503, -9.251858538542967489E-15 ) ) ;
#5232 = EDGE_CURVE ( 'NONE', #2258, #2672, #26150, .T. ) ;
#5233 = CARTESIAN_POINT ( 'NONE',  ( -13.62135916515834388, 20.99999999990137312, -68.61085694035826066 ) ) ;
#5234 = CARTESIAN_POINT ( 'NONE',  ( 10.69999999994746887, -28.83990707537207143, -19.12610387680327761 ) ) ;
#5235 = ORIENTED_EDGE ( 'NONE', *, *, #17787, .F. ) ;
#5236 = ADVANCED_FACE ( 'NONE', ( #11829 ), #24902, .F. ) ;
#5237 = CARTESIAN_POINT ( 'NONE',  ( 13.12132034340000075, 20.99999999990000887, -69.22132034359999864 ) ) ;
#5238 = CARTESIAN_POINT ( 'NONE',  ( 0.5300456733980246637, -4.293941145674104121, -18.37054674910000429 ) ) ;
#5239 = DIRECTION ( 'NONE',  ( -0.3326278240906416217, 4.073516000799531462E-17, 0.9430581798811381589 ) ) ;
#5240 = DIRECTION ( 'NONE',  ( -0.1090476345695678695, -0.6986477033489640887, -0.7071067811865474617 ) ) ;
#5241 = PRESENTATION_LAYER_ASSIGNMENT (  '', '', ( #15305 ) ) ;
#5242 = CARTESIAN_POINT ( 'NONE',  ( 1.100000000000000089, -26.77741585740000119, 5.000000000000000000 ) ) ;
#5243 = DIRECTION ( 'NONE',  ( 1.000000000000000000, 0.000000000000000000, 0.000000000000000000 ) ) ;
#5244 = CARTESIAN_POINT ( 'NONE',  ( 27.92857142820000149, 1.776356839399999804E-15, 192.0603150150000147 ) ) ;
#5245 = CARTESIAN_POINT ( 'NONE',  ( 12.77819780750000156, 20.99999999999999645, -56.09999999999999432 ) ) ;
#5246 = EDGE_CURVE ( 'NONE', #5717, #13930, #5146, .T. ) ;
#5247 = DIRECTION ( 'NONE',  ( -1.000000000000000000, 0.000000000000000000, 0.000000000000000000 ) ) ;
#5248 = CARTESIAN_POINT ( 'NONE',  ( 27.06563794080000207, -3.314475219239999417E-15, 191.9402686260000053 ) ) ;
#5249 = DIRECTION ( 'NONE',  ( 0.000000000000000000, 0.000000000000000000, -1.000000000000000000 ) ) ;
#5250 = PLANE ( 'NONE',  #30366 ) ;
#5251 = AXIS2_PLACEMENT_3D ( 'NONE', #18600, #13725, #14047 ) ;
#5252 = VERTEX_POINT ( 'NONE', #19376 ) ;
#5253 = CARTESIAN_POINT ( 'NONE',  ( -5.939015604524707115, -0.1501891088408410790, -53.07673954922500315 ) ) ;
#5254 = DIRECTION ( 'NONE',  ( 2.416122857340496113E-12, -0.9341647027306024809, -0.3568421334038978099 ) ) ;
#5255 = CIRCLE ( 'NONE', #13288, 2.926829268290000119 ) ;
#5256 = AXIS2_PLACEMENT_3D ( 'NONE', #15966, #4010, #13607 ) ;
#5257 = CARTESIAN_POINT ( 'NONE',  ( -26.93580492059415121, 9.103810007694223216, 1.000000000000000888 ) ) ;
#5258 = B_SPLINE_CURVE_WITH_KNOTS ( 'NONE', 3,
 ( #30456, #9344, #11249, #30758, #8878, #28080, #25576, #28398, #30613, #16274, #23534, #6525 ),
 .UNSPECIFIED., .F., .F.,
 ( 4, 2, 2, 2, 2, 4 ),
 ( 0.000000000000000000, 0.2500000000000021094, 0.3750000000000024980, 0.5000000000000028866, 0.7500000000000014433, 1.000000000000000000 ),
 .UNSPECIFIED. ) ;
#5259 = CARTESIAN_POINT ( 'NONE',  ( -4.247090937810456879, 0.9000947937473684490, -68.10000000002501963 ) ) ;
#5260 = ORIENTED_EDGE ( 'NONE', *, *, #4372, .F. ) ;
#5261 = CARTESIAN_POINT ( 'NONE',  ( 2.914123423709013228, 2.127246859543532764, -88.52261276242110455 ) ) ;
#5262 = VERTEX_POINT ( 'NONE', #29118 ) ;
#5263 = FACE_BOUND ( 'NONE', #13903, .T. ) ;
#5264 = AXIS2_PLACEMENT_3D ( 'NONE', #13438, #23054, #11090 ) ;
#5265 = CARTESIAN_POINT ( 'NONE',  ( -9.999999999979998222, -127.2536115484999897, -34.36329565063000047 ) ) ;
#5266 = ORIENTED_EDGE ( 'NONE', *, *, #12718, .T. ) ;
#5267 = CARTESIAN_POINT ( 'NONE',  ( 1.566980368899947962, 4.067530462867743779, -26.09462237480000724 ) ) ;
#5268 = CYLINDRICAL_SURFACE ( 'NONE', #23984, 0.9999999999999988898 ) ;
#5269 = CARTESIAN_POINT ( 'NONE',  ( 0.6613659943794023555, -4.850238491497668392, -49.76468436622499780 ) ) ;
#5270 = ADVANCED_FACE ( 'NONE', ( #4900 ), #6945, .F. ) ;
#5272 = CARTESIAN_POINT ( 'NONE',  ( -24.05715877250037948, -13.32261293358842025, 4.005116771804169140 ) ) ;
#5271 = AXIS2_PLACEMENT_3D ( 'NONE', #9862, #19462, #29053 ) ;
#5273 = B_SPLINE_CURVE_WITH_KNOTS ( 'NONE', 5,
 ( #9704, #12216, #18992, #7038, #19617, #4839, #11910, #21827, #16628, #283, #4674, #26236, #14284, #19463, #14436 ),
 .UNSPECIFIED., .F., .F.,
 ( 6, 3, 3, 3, 6 ),
 ( 0.000000000000000000, 0.1000000000040084519, 0.3999999999988547716, 0.6999999999999999556, 1.000000000000000000 ),
 .UNSPECIFIED. ) ;
#5274 = B_SPLINE_CURVE_WITH_KNOTS ( 'NONE', 1,
 ( #23840, #6678 ),
 .UNSPECIFIED., .F., .F.,
 ( 2, 2 ),
 ( -2.556026163500000058E-06, 0.7000000000009999335 ),
 .UNSPECIFIED. ) ;
#5275 = VECTOR ( 'NONE', #28362, 1000.000000000000000 ) ;
#5276 = FILL_AREA_STYLE_COLOUR ( '', #6386 ) ;
#5277 = CARTESIAN_POINT ( 'NONE',  ( -4.129410714115038239, -19.58013141257310252, -27.92930099280837197 ) ) ;
#5278 = UNCERTAINTY_MEASURE_WITH_UNIT (LENGTH_MEASURE( 1.000000000000000082E-05 ), #18011, 'distance_accuracy_value', 'NONE');
#5279 = EDGE_CURVE ( 'NONE', #21828, #21856, #23354, .T. ) ;
#5280 = CARTESIAN_POINT ( 'NONE',  ( -7.999999999681902452, -14.92844969907143771, -33.25053330396754347 ) ) ;
#5281 = ADVANCED_FACE ( 'NONE', ( #5049 ), #28500, .F. ) ;
#5282 = EDGE_CURVE ( 'NONE', #11580, #23901, #2390, .T. ) ;
#5283 = CARTESIAN_POINT ( 'NONE',  ( -10.99999999999209344, -15.94902145825930617, -35.53273252503056767 ) ) ;
#5284 = EDGE_LOOP ( 'NONE', ( #4730, #3061, #16118, #7392 ) ) ;
#5285 = CARTESIAN_POINT ( 'NONE',  ( 14.74927456580200946, -31.99974519688053576, -29.72362367442748976 ) ) ;
#5286 = CARTESIAN_POINT ( 'NONE',  ( 23.20948082139999968, -13.40000000000000036, 223.8999999999999773 ) ) ;
#5287 = CARTESIAN_POINT ( 'NONE',  ( -23.81776757772072983, -15.65134804123479917, 5.104183903000020450 ) ) ;
#5288 = LINE ( 'NONE', #2772, #10747 ) ;
#5289 = CARTESIAN_POINT ( 'NONE',  ( -23.89302272057183885, -14.21215728459360150, 3.899998580999983311 ) ) ;
#5290 = DIRECTION ( 'NONE',  ( 0.000000000000000000, 1.665334536939999828E-16, -1.000000000000000000 ) ) ;
#5291 = CARTESIAN_POINT ( 'NONE',  ( 3.532024942903766007, -2.488032516543696282, -0.6999999999999994005 ) ) ;
#5292 = CARTESIAN_POINT ( 'NONE',  ( -26.90707039800299327, -7.574539066456210001, -0.6999999999999784173 ) ) ;
#5293 = CARTESIAN_POINT ( 'NONE',  ( 10.45000000009999930, -26.99999999999950617, -28.39999999990030588 ) ) ;
#5294 = AXIS2_PLACEMENT_3D ( 'NONE', #25055, #22549, #24598 ) ;
#5295 = STYLED_ITEM ( 'NONE', ( #18094 ), #9916 ) ;
#5296 = DIRECTION ( 'NONE',  ( 0.000000000000000000, 0.9396926207858125046, 0.3420201433259318358 ) ) ;
#5297 = CARTESIAN_POINT ( 'NONE',  ( 17.43495665862128874, 12.07643063644571946, 1.385610376436474414E-13 ) ) ;
#5298 = CARTESIAN_POINT ( 'NONE',  ( 10.69999999989999928, -45.00000000000000000, -7.274962170899998526 ) ) ;
#5299 = CARTESIAN_POINT ( 'NONE',  ( 18.26639035964474900, 11.02001161816309072, -0.6999999999999784173 ) ) ;
#5300 = ORIENTED_EDGE ( 'NONE', *, *, #13617, .F. ) ;
#5301 = CARTESIAN_POINT ( 'NONE',  ( 7.638687372291747657, 2.805115907256121144, -42.18512143522137592 ) ) ;
#5302 = CARTESIAN_POINT ( 'NONE',  ( 25.11738521000000190, -13.46751580659999981, 225.6806823370000075 ) ) ;
#5303 = CARTESIAN_POINT ( 'NONE',  ( 4.921121033118705412, -0.08698047164986451307, -58.84793411332501023 ) ) ;
#5304 = ORIENTED_EDGE ( 'NONE', *, *, #14737, .T. ) ;
#5305 = ORIENTED_EDGE ( 'NONE', *, *, #25713, .T. ) ;
#5306 = CARTESIAN_POINT ( 'NONE',  ( -10.00000000000000000, 20.99999999999999645, -62.10000000019999788 ) ) ;
#5307 = VERTEX_POINT ( 'NONE', #14657 ) ;
#5308 = PRODUCT_DEFINITION_FORMATION_WITH_SPECIFIED_SOURCE ( 'ANY', '', #28241, .NOT_KNOWN. ) ;
#5309 = ORIENTED_EDGE ( 'NONE', *, *, #2339, .T. ) ;
#5310 = CARTESIAN_POINT ( 'NONE',  ( 1.484924240490000047, 1.484924240490000047, 226.6412452697800006 ) ) ;
#5311 = CARTESIAN_POINT ( 'NONE',  ( -24.14205448738587023, 13.78537896750705194, 3.957489350000009676 ) ) ;
#5312 = FACE_OUTER_BOUND ( 'NONE', #1633, .T. ) ;
#5313 = CARTESIAN_POINT ( 'NONE',  ( 17.56757767936423775, 12.03437313983793011, -1.400000000000002132 ) ) ;
#5314 = CARTESIAN_POINT ( 'NONE',  ( 10.69999999999999929, -29.30501631380000305, -26.47986985000000004 ) ) ;
#5315 = CARTESIAN_POINT ( 'NONE',  ( 3.834994720502944876, -2.823021758520125601, -8.035276792900001297 ) ) ;
#5316 = FACE_OUTER_BOUND ( 'NONE', #28028, .T. ) ;
#5317 = ORIENTED_EDGE ( 'NONE', *, *, #6110, .F. ) ;
#5318 = CARTESIAN_POINT ( 'NONE',  ( 2.662870350918720597, -3.902358757652288901, -44.10000000002498410 ) ) ;
#5319 = CARTESIAN_POINT ( 'NONE',  ( 24.75645985066740806, 14.12045945716145390, 4.098702612000016288 ) ) ;
#5320 = CARTESIAN_POINT ( 'NONE',  ( -4.219802143832970920, -3.088637908568292012, -19.87254627010000263 ) ) ;
#5321 = CARTESIAN_POINT ( 'NONE',  ( -12.31579099197426075, -24.11373924793705115, -32.50693151577021212 ) ) ;
#5322 = CARTESIAN_POINT ( 'NONE',  ( 380005.9281980000087, 207598.1847299999790, -249768.1509097300004 ) ) ;
#5323 = CARTESIAN_POINT ( 'NONE',  ( -27.76135143710000008, 3.399672736049999681E-15, 187.6614141010000196 ) ) ;
#5324 = CARTESIAN_POINT ( 'NONE',  ( 3.389121577690000109, 11.55088360999999963, 229.6412452697800006 ) ) ;
#5325 = CARTESIAN_POINT ( 'NONE',  ( -6.340437944841875506, 0.6332316896323284539, -47.14737393802499810 ) ) ;
#5326 = CARTESIAN_POINT ( 'NONE',  ( -7.999999999957778662, -114.8354788345922941, 7.878836663909118521 ) ) ;
#5327 = CARTESIAN_POINT ( 'NONE',  ( -27.06563794070000029, 3.314475219249999806E-15, 141.9402686260000053 ) ) ;
#5328 = DIRECTION ( 'NONE',  ( 2.257144471330000330E-12, -0.000000000000000000, -1.000000000000000000 ) ) ;
#5329 = CARTESIAN_POINT ( 'NONE',  ( -26.80000000000000071, 4.518892556989999143, 230.0000000000000000 ) ) ;
#5330 = EDGE_CURVE ( 'NONE', #3101, #27268, #28858, .T. ) ;
#5331 = DIRECTION ( 'NONE',  ( 0.9595496299847263710, -0.2815395311429191305, 0.000000000000000000 ) ) ;
#5332 = ORIENTED_EDGE ( 'NONE', *, *, #22076, .T. ) ;
#5333 = CARTESIAN_POINT ( 'NONE',  ( -5.984522419796141079, -1.167122196978044535, -31.69652066320000117 ) ) ;
#5334 = ORIENTED_EDGE ( 'NONE', *, *, #19066, .T. ) ;
#5335 = CARTESIAN_POINT ( 'NONE',  ( 23.95771898011812340, -13.50170546717094311, 3.928090679509207206 ) ) ;
#5336 = CARTESIAN_POINT ( 'NONE',  ( -2.769456955792640951, 4.065643307668772799, -48.80391720702499470 ) ) ;
#5337 = ORIENTED_EDGE ( 'NONE', *, *, #22251, .F. ) ;
#5338 = ADVANCED_FACE ( 'NONE', ( #26300 ), #21268, .F. ) ;
#5339 = VERTEX_POINT ( 'NONE', #28656 ) ;
#5340 = SHAPE_DEFINITION_REPRESENTATION ( #11415, #25228 ) ;
#5341 = ORIENTED_EDGE ( 'NONE', *, *, #16783, .T. ) ;
#5343 = CARTESIAN_POINT ( 'NONE',  ( -7.999999999727681832, -25.78362547594782583, -25.65764409411462310 ) ) ;
#5342 = B_SPLINE_CURVE_WITH_KNOTS ( 'NONE', 3,
 ( #4661, #28267, #21661, #9217, #18977, #23415, #23875, #4197, #28585, #11743, #11595, #9691 ),
 .UNSPECIFIED., .F., .F.,
 ( 4, 2, 2, 2, 2, 4 ),
 ( 0.000000000000000000, 0.2500000000000334177, 0.3750000000000278666, 0.5000000000000223155, 0.7500000000000111022, 1.000000000000000000 ),
 .UNSPECIFIED. ) ;
#5344 = ORIENTED_EDGE ( 'NONE', *, *, #4249, .T. ) ;
#5345 = CARTESIAN_POINT ( 'NONE',  ( -10.00000000000000000, 4.552933401020911042, -69.34955285734142194 ) ) ;
#5346 = CARTESIAN_POINT ( 'NONE',  ( -5.702373156330470927, -9.141065521210249400, -36.35857944363798566 ) ) ;
#5347 = CARTESIAN_POINT ( 'NONE',  ( 27.51770821235203357, 4.728187301808492116, 1.000000000000000888 ) ) ;
#5348 = CARTESIAN_POINT ( 'NONE',  ( -12.29999999970000069, -27.00000000000000000, -28.40000000001083436 ) ) ;
#5349 = CARTESIAN_POINT ( 'NONE',  ( -12.49647831262676512, -27.90203718307900260, -23.14770133019309739 ) ) ;
#5350 = CARTESIAN_POINT ( 'NONE',  ( 13.12132034340000075, 21.69999999990000106, -69.22132034359999864 ) ) ;
#5351 = CARTESIAN_POINT ( 'NONE',  ( 0.5877407897813130555, -4.297347728519515186, -0.3731240480000022619 ) ) ;
#5352 = CARTESIAN_POINT ( 'NONE',  ( 28.50000000000000000, -3.490128108379999702E-15, 40.00000000000000000 ) ) ;
#5353 = EDGE_LOOP ( 'NONE', ( #14979, #20824, #16001, #18891 ) ) ;
#5354 = CARTESIAN_POINT ( 'NONE',  ( -3.950034095761360664, 2.484763540022561834, -10.94547590279999838 ) ) ;
#5355 = CARTESIAN_POINT ( 'NONE',  ( -2.923929784071483073, -5.123485640109426420, -29.67642233980000910 ) ) ;
#5356 = CARTESIAN_POINT ( 'NONE',  ( -7.867425209648341244, -15.86465192213301911, -74.65259062561435144 ) ) ;
#5357 = ADVANCED_FACE ( 'NONE', ( #4749 ), #14354, .F. ) ;
#5358 = CARTESIAN_POINT ( 'NONE',  ( 24.88589369718092215, -13.89120818692358483, 6.095967889000020179 ) ) ;
#5359 = CARTESIAN_POINT ( 'NONE',  ( 20.25359293946302941, 20.00000005145030002, 0.6182840029999858711 ) ) ;
#5360 = FILL_AREA_STYLE ('',( #26924 ) ) ;
#5361 = CARTESIAN_POINT ( 'NONE',  ( 3.760007715734311251, -19.71206033701148996, -27.86495495698533986 ) ) ;
#5362 = CARTESIAN_POINT ( 'NONE',  ( -8.699999999728817102, -29.34680062185485738, -26.49035620860901474 ) ) ;
#5363 = B_SPLINE_SURFACE_WITH_KNOTS ( 'NONE', 5, 1, ( 
 ( #18192, #25454 ),
 ( #1844, #3566 ),
 ( #20563, #6248 ),
 ( #13160, #29995 ),
 ( #1220, #15851 ),
 ( #3888, #27636 ),
 ( #6081, #11127 ),
 ( #4196, #20724 ),
 ( #15679, #25289 ) ),
 .UNSPECIFIED., .F., .F., .F.,
 ( 6, 3, 6 ),
 ( 2, 2 ),
 ( 0.000000000000000000, 55.31395511720000258, 94.75474465359999954 ),
 ( -3.500000000000000000, 3.500000000000000000 ),
 .UNSPECIFIED. ) ;
#5364 = CARTESIAN_POINT ( 'NONE',  ( 0.9758793681798838549, -27.78334643822867633, 6.002515439000016606 ) ) ;
#5365 = LINE ( 'NONE', #14512, #3698 ) ;
#5366 = CARTESIAN_POINT ( 'NONE',  ( 0.1574870170986610307, -3.500159137052063496, 230.8361063485508566 ) ) ;
#5367 = ORIENTED_EDGE ( 'NONE', *, *, #3492, .T. ) ;
#5368 = VECTOR ( 'NONE', #12353, 1000.000000000000114 ) ;
#5369 = DIRECTION ( 'NONE',  ( 0.000000000000000000, 0.000000000000000000, -1.000000000000000000 ) ) ;
#5370 = CARTESIAN_POINT ( 'NONE',  ( -2.200711091379580431, -20.50181238076427448, -27.47976714836060097 ) ) ;
#5371 = ORIENTED_EDGE ( 'NONE', *, *, #26182, .F. ) ;
#5372 = CARTESIAN_POINT ( 'NONE',  ( 23.55411374389282386, 16.04538543799059980, 8.000000000000007105 ) ) ;
#5373 = CARTESIAN_POINT ( 'NONE',  ( -1.419173393149999842E-06, -27.80022181310000207, 226.1000014189999945 ) ) ;
#5374 = VERTEX_POINT ( 'NONE', #19216 ) ;
#5375 = CARTESIAN_POINT ( 'NONE',  ( 9.738910687886868089, -24.96785170200598358, 36.78285841123148003 ) ) ;
#5376 = ORIENTED_EDGE ( 'NONE', *, *, #14126, .F. ) ;
#5377 = EDGE_CURVE ( 'NONE', #9001, #24684, #1370, .T. ) ;
#5378 = EDGE_LOOP ( 'NONE', ( #11345, #18822, #7457, #14477 ) ) ;
#5379 = ORIENTED_EDGE ( 'NONE', *, *, #8530, .F. ) ;
#5380 = CARTESIAN_POINT ( 'NONE',  ( 27.44334449189999958, 9.611089166140001083, 229.4982322489999831 ) ) ;
#5381 = CARTESIAN_POINT ( 'NONE',  ( -28.50000000000000000, 5.427757009279999762E-15, 222.0000000000000000 ) ) ;
#5382 = CARTESIAN_POINT ( 'NONE',  ( -10.69999999999999929, -24.90229870320000316, -26.25506064210000190 ) ) ;
#5383 = EDGE_LOOP ( 'NONE', ( #28747, #11348, #16725, #28288 ) ) ;
#5384 = B_SPLINE_CURVE_WITH_KNOTS ( 'NONE', 3,
 ( #1966, #23375, #28073, #6519, #1812, #30911, #25886, #18781, #30606, #28391, #11401, #6828, #28542, #16427, #11707, #27924, #9339, #6990 ),
 .UNSPECIFIED., .F., .F.,
 ( 4, 2, 2, 2, 2, 2, 2, 2, 4 ),
 ( 0.000000000000000000, 0.1249999999999999445, 0.2499999999999999445, 0.3749999999999999445, 0.5000000000000000000, 0.6250000000000000000, 0.7500000000000000000, 0.8749999999999998890, 1.000000000000000000 ),
 .UNSPECIFIED. ) ;
#5385 = CARTESIAN_POINT ( 'NONE',  ( 0.4478609109052260062, -28.49673184309145668, 6.098651241000007772 ) ) ;
#5386 = DIRECTION ( 'NONE',  ( -1.000000000000000000, 5.687697993419811493E-16, -6.771501495049272772E-12 ) ) ;
#5387 = EDGE_CURVE ( 'NONE', #16796, #5989, #6660, .T. ) ;
#5388 = CIRCLE ( 'NONE', #14969, 2.100000000000000089 ) ;
#5389 = EDGE_CURVE ( 'NONE', #22997, #6732, #15815, .T. ) ;
#5390 = DIRECTION ( 'NONE',  ( -0.8329895880221871440, 0.5532886644841251700, 0.000000000000000000 ) ) ;
#5391 = CARTESIAN_POINT ( 'NONE',  ( -3.665401116828205463, 4.874126016103034864, -19.03064294429999848 ) ) ;
#5392 = LINE ( 'NONE', #11516, #26408 ) ;
#5393 = CARTESIAN_POINT ( 'NONE',  ( 6.481092934035197040, 4.607732177564153098, -43.06431613492966903 ) ) ;
#5394 = DIRECTION ( 'NONE',  ( 1.000000000000000000, -0.000000000000000000, -2.257150022439999944E-12 ) ) ;
#5395 = LINE ( 'NONE', #17354, #2745 ) ;
#5396 = CARTESIAN_POINT ( 'NONE',  ( 10.00000000070000183, 19.99999999999999645, -22.39999999999999858 ) ) ;
#5397 = B_SPLINE_CURVE_WITH_KNOTS ( 'NONE', 5,
 ( #29540, #29384, #21858, #309, #3104, #22466, #7666, #24365, #15073, #29076, #27030, #26717, #7522, #24826, #2806 ),
 .UNSPECIFIED., .F., .F.,
 ( 6, 3, 3, 3, 6 ),
 ( 0.000000000000000000, 0.2999999999994274469, 0.6000000000000000888, 0.8999999999971368680, 1.000000000000000000 ),
 .UNSPECIFIED. ) ;
#5398 = CARTESIAN_POINT ( 'NONE',  ( -10.69999999999999929, -24.97190126590000148, -30.61453681870000310 ) ) ;
#5399 = CARTESIAN_POINT ( 'NONE',  ( 18.32613298889999953, 20.54575842250000051, 229.7313256499999738 ) ) ;
#5400 = CARTESIAN_POINT ( 'NONE',  ( -6.661312627754254478, -7.245008774242306160, -33.94554228703383103 ) ) ;
#5401 = ORIENTED_EDGE ( 'NONE', *, *, #23222, .T. ) ;
#5402 = CARTESIAN_POINT ( 'NONE',  ( 0.7192951553254764985, 4.518739695583327887, -54.41500058692499664 ) ) ;
#5403 = CARTESIAN_POINT ( 'NONE',  ( -12.38011772156684920, -25.48083565910511794, -23.50369165914649727 ) ) ;
#5404 = CARTESIAN_POINT ( 'NONE',  ( -24.95150188576097960, 13.62250486154599294, 1.000000000000000888 ) ) ;
#5405 = EDGE_CURVE ( 'NONE', #931, #3809, #10010, .T. ) ;
#5406 = CARTESIAN_POINT ( 'NONE',  ( -4.444041428977288710, 1.101146991380681728, -68.10000000002500542 ) ) ;
#5407 = ORIENTED_EDGE ( 'NONE', *, *, #20120, .T. ) ;
#5408 = AXIS2_PLACEMENT_3D ( 'NONE', #17904, #3593, #15404 ) ;
#5409 = CARTESIAN_POINT ( 'NONE',  ( -2.113314637130261353, 3.003384554638903303, -91.89588846697527913 ) ) ;
#5410 =( LENGTH_UNIT ( ) NAMED_UNIT ( * ) SI_UNIT ( .MILLI., .METRE. ) );
#5411 = AXIS2_PLACEMENT_3D ( 'NONE', #28568, #25750, #23077 ) ;
#5412 = EDGE_LOOP ( 'NONE', ( #16250, #14062, #10377, #22637 ) ) ;
#5413 = CARTESIAN_POINT ( 'NONE',  ( -24.49145440958036701, 14.57548795270903774, 4.319167817000008291 ) ) ;
#5414 = AXIS2_PLACEMENT_3D ( 'NONE', #9819, #16892, #9975 ) ;
#5415 = LINE ( 'NONE', #5722, #31091 ) ;
#5416 = ORIENTED_EDGE ( 'NONE', *, *, #26922, .T. ) ;
#5417 = CARTESIAN_POINT ( 'NONE',  ( -1.458225024262878255, -5.692467481908745519, -28.54882611460000419 ) ) ;
#5418 = ADVANCED_FACE ( 'NONE', ( #8594 ), #22936, .T. ) ;
#5419 = DIRECTION ( 'NONE',  ( 1.635844237846128888E-12, 0.6889064844606307414, -0.7248502298186121351 ) ) ;
#5420 = CARTESIAN_POINT ( 'NONE',  ( -22.26220695934820171, 17.72099999758041378, -0.2432540810000105580 ) ) ;
#5421 = CARTESIAN_POINT ( 'NONE',  ( -24.34663841808528062, -12.78636765232546324, 4.903540287127751363 ) ) ;
#5422 = CARTESIAN_POINT ( 'NONE',  ( -11.69999999989999928, -2.500000000000002220, -1.399999999999998579 ) ) ;
#5423 =( GEOMETRIC_REPRESENTATION_CONTEXT ( 3 ) GLOBAL_UNCERTAINTY_ASSIGNED_CONTEXT ( ( #12542 ) ) GLOBAL_UNIT_ASSIGNED_CONTEXT ( ( #21407, #2054, #13259 ) ) REPRESENTATION_CONTEXT ( 'NONE', 'WORKASPACE' ) );
#5424 = ORIENTED_EDGE ( 'NONE', *, *, #3059, .F. ) ;
#5425 = B_SPLINE_CURVE_WITH_KNOTS ( 'NONE', 3,
 ( #21762, #17182, #24434, #12151, #26479, #10114 ),
 .UNSPECIFIED., .F., .F.,
 ( 4, 2, 4 ),
 ( 0.000000000000000000, 0.5000000000000000000, 1.000000000000000000 ),
 .UNSPECIFIED. ) ;
#5426 = DIRECTION ( 'NONE',  ( -1.000000000000000000, 0.000000000000000000, 0.000000000000000000 ) ) ;
#5427 = CARTESIAN_POINT ( 'NONE',  ( -17.39358994609593267, -22.00021533137563168, -29.72298993498152697 ) ) ;
#5428 = VERTEX_POINT ( 'NONE', #29579 ) ;
#5429 = CARTESIAN_POINT ( 'NONE',  ( 14.74466352504733813, -31.99976755572771836, -27.04560447322398176 ) ) ;
#5430 = CARTESIAN_POINT ( 'NONE',  ( 8.999999999770000869, 21.70000000000000284, -53.60000000000000142 ) ) ;
#5431 = LINE ( 'NONE', #10008, #1236 ) ;
#5432 = AXIS2_PLACEMENT_3D ( 'NONE', #28018, #6614, #16217 ) ;
#5433 = CARTESIAN_POINT ( 'NONE',  ( 2.798846661298902916, -1.899199287238114930, -96.93852766386672215 ) ) ;
#5434 = CARTESIAN_POINT ( 'NONE',  ( 23.83740787290000185, -14.30495753649999990, 223.9972528570000065 ) ) ;
#5435 = CARTESIAN_POINT ( 'NONE',  ( -4.671347416476984371, -26.39088508839784453, 209.5126867146601910 ) ) ;
#5436 = CARTESIAN_POINT ( 'NONE',  ( 3.452488641071199460, -2.537741030969793865, -0.6999999999999991784 ) ) ;
#5437 = AXIS2_PLACEMENT_3D ( 'NONE', #1025, #5880, #15636 ) ;
#5438 = CARTESIAN_POINT ( 'NONE',  ( -27.03594125075309762, -0.4919295335571663430, -0.6999999999999784173 ) ) ;
#5439 = CARTESIAN_POINT ( 'NONE',  ( 1.071537507505435638, -27.47917025549320513, 4.713010325135398304 ) ) ;
#5440 = DIRECTION ( 'NONE',  ( -0.000000000000000000, -0.000000000000000000, -1.000000000000000000 ) ) ;
#5441 = CARTESIAN_POINT ( 'NONE',  ( 17.82645929468907298, 11.89178602526930817, 1.385610376436474667E-13 ) ) ;
#5442 = CARTESIAN_POINT ( 'NONE',  ( -1.841797396446221979, -26.73663745407121795, 20.00000000000000355 ) ) ;
#5443 = CARTESIAN_POINT ( 'NONE',  ( -0.1464386042498656837, -27.80011885101298930, 5.900904413000008120 ) ) ;
#5444 = ADVANCED_FACE ( 'NONE', ( #22196 ), #8758, .F. ) ;
#5445 = ORIENTED_EDGE ( 'NONE', *, *, #25645, .T. ) ;
#5446 = AXIS2_PLACEMENT_3D ( 'NONE', #21532, #2798, #16953 ) ;
#5447 = CARTESIAN_POINT ( 'NONE',  ( 11.63809019220000174, -24.14124255329999968, -0.6999999999999992895 ) ) ;
#5448 = ADVANCED_FACE ( 'NONE', ( #20565 ), #24407, .T. ) ;
#5449 = EDGE_CURVE ( 'NONE', #27611, #30938, #23574, .T. ) ;
#5450 = CARTESIAN_POINT ( 'NONE',  ( 24.68173674080000168, -14.25001227039999918, 226.1000014189999945 ) ) ;
#5451 = VECTOR ( 'NONE', #24263, 1000.000000000000114 ) ;
#5452 = CARTESIAN_POINT ( 'NONE',  ( -3.351703491987489958, 4.047634511443764183, -63.74933298492499034 ) ) ;
#5453 = ORIENTED_EDGE ( 'NONE', *, *, #22848, .F. ) ;
#5454 = EDGE_LOOP ( 'NONE', ( #19933, #23219, #15745, #8653, #11798, #2557, #27583, #5376, #7972, #12452 ) ) ;
#5456 = CARTESIAN_POINT ( 'NONE',  ( 27.89787437582684859, -9.677414786515893041, 0.5514269430000329208 ) ) ;
#5455 = AXIS2_PLACEMENT_3D ( 'NONE', #22550, #29464, #20024 ) ;
#5457 = ORIENTED_EDGE ( 'NONE', *, *, #27275, .F. ) ;
#5458 = CARTESIAN_POINT ( 'NONE',  ( -0.1113126277073495929, 2.989789856717120387, -42.27519293863267791 ) ) ;
#5459 = CARTESIAN_POINT ( 'NONE',  ( -24.90302310912370132, 13.86047864606265279, 3.901342110999989288 ) ) ;
#5460 = FACE_OUTER_BOUND ( 'NONE', #20828, .T. ) ;
#5461 = CARTESIAN_POINT ( 'NONE',  ( -8.881784197000000993E-16, -8.881784197000000993E-16, 227.6412452697800006 ) ) ;
#5462 = CARTESIAN_POINT ( 'NONE',  ( 10.69999999996534967, -29.70167663135993408, -27.04935189346707602 ) ) ;
#5463 = CARTESIAN_POINT ( 'NONE',  ( -23.81866442513004856, -14.33570206453694240, 6.099998581000020792 ) ) ;
#5464 = EDGE_LOOP ( 'NONE', ( #6335, #14608, #8373, #8852 ) ) ;
#5465 = CARTESIAN_POINT ( 'NONE',  ( 2.770284657207440659, -3.443617497140548434, -44.10000000002499831 ) ) ;
#5466 = DIRECTION ( 'NONE',  ( -1.181300906760215537E-13, 0.9986295347541825906, 0.05233595625040957794 ) ) ;
#5467 = CIRCLE ( 'NONE', #1983, 4.439999999999999503 ) ;
#5468 = CARTESIAN_POINT ( 'NONE',  ( -1.782928038406566884, 3.983823234458335527, -23.23780126170000671 ) ) ;
#5469 = CARTESIAN_POINT ( 'NONE',  ( -12.67644879028841309, -26.76800376598850661, -34.03955960393551550 ) ) ;
#5470 = DIRECTION ( 'NONE',  ( 0.000000000000000000, 0.000000000000000000, 1.000000000000000000 ) ) ;
#5471 = DIRECTION ( 'NONE',  ( 0.000000000000000000, -1.000000000000000000, 0.000000000000000000 ) ) ;
#5472 = CARTESIAN_POINT ( 'NONE',  ( 8.700000000276082446, -16.84110654130126150, -33.19737377701691372 ) ) ;
#5473 = CARTESIAN_POINT ( 'NONE',  ( -1.572917327626556228, -4.621985533170462901, -46.24520033292499477 ) ) ;
#5474 = CARTESIAN_POINT ( 'NONE',  ( 9.999999999959999997, -25.00000000000000000, -26.16393202319999745 ) ) ;
#5475 = CARTESIAN_POINT ( 'NONE',  ( 11.08346179031909529, -28.41490585489483678, 136.3944487250000179 ) ) ;
#5476 = CARTESIAN_POINT ( 'NONE',  ( -18.80296799075907543, 19.99998601668219678, 230.5746565848800742 ) ) ;
#5477 = AXIS2_PLACEMENT_3D ( 'NONE', #17844, #25425, #15186 ) ;
#5478 = LINE ( 'NONE', #20118, #6262 ) ;
#5479 = EDGE_CURVE ( 'NONE', #14785, #7767, #23866, .T. ) ;
#5480 = CARTESIAN_POINT ( 'NONE',  ( -1.822228222620360105, 1.053429627095256338, 226.6412452697799722 ) ) ;
#5481 = B_SPLINE_CURVE_WITH_KNOTS ( 'NONE', 3,
 ( #9111, #6756, #10866, #20451, #4398, #6444, #11017, #1267, #1582, #4247, #18233, #20765, #25659, #30373, #4089, #13687, #13846, #28310, #18559, #23290, #6128, #23456, #20928, #22978, #1735, #16353 ),
 .UNSPECIFIED., .F., .F.,
 ( 4, 2, 2, 1, 1, 2, 2, 2, 2, 2, 1, 1, 2, 2, 4 ),
 ( 0.000000000000000000, 0.1249999999999754086, 0.1874999999999651112, 0.2187499999999598377, 0.2343749999999587830, 0.2421874999999582556, 0.2499999999999577560, 0.4999999999999693578, 0.6249999999999750200, 0.6874999999999777955, 0.7187499999999790168, 0.7343749999999812372, 0.7421874999999835687, 0.7499999999999859002, 1.000000000000000000 ),
 .UNSPECIFIED. ) ;
#5482 = ORIENTED_EDGE ( 'NONE', *, *, #6809, .F. ) ;
#5483 = CARTESIAN_POINT ( 'NONE',  ( -3.866422574246632937, 4.445403037619903408, -29.58728588870000209 ) ) ;
#5484 = EDGE_CURVE ( 'NONE', #18608, #26133, #19843, .T. ) ;
#5485 = ORIENTED_EDGE ( 'NONE', *, *, #25016, .F. ) ;
#5486 = DIRECTION ( 'NONE',  ( 0.000000000000000000, -1.000000000000000000, 0.000000000000000000 ) ) ;
#5487 = CARTESIAN_POINT ( 'NONE',  ( -0.9881560945370695404, 5.823346091562972227, -51.25792092402499378 ) ) ;
#5488 = EDGE_LOOP ( 'NONE', ( #27503, #15488, #8684, #8669, #23780, #8219, #19638, #22878, #8071, #6815, #24594, #14210, #22404, #28136, #3713, #2377, #24766, #18086, #2088, #25941 ) ) ;
#5489 = ORIENTED_EDGE ( 'NONE', *, *, #14624, .F. ) ;
#5490 = APPLICATION_PROTOCOL_DEFINITION ( 'draft international standard', 'automotive_design', 1998, #22038 ) ;
#5491 = ORIENTED_EDGE ( 'NONE', *, *, #24846, .F. ) ;
#5492 = ORIENTED_EDGE ( 'NONE', *, *, #5484, .F. ) ;
#5493 = CARTESIAN_POINT ( 'NONE',  ( 24.05832192669999969, -13.92979812329999945, 226.1000014189999945 ) ) ;
#5494 = CARTESIAN_POINT ( 'NONE',  ( 24.45473033137484720, 14.63622297804190175, 3.901342939999996595 ) ) ;
#5495 = CARTESIAN_POINT ( 'NONE',  ( 0.000000000000000000, 0.000000000000000000, 115.0000000000000000 ) ) ;
#5496 = DIRECTION ( 'NONE',  ( 1.000000000000000000, -9.219999999999999084E-13, 4.710999999999999616E-12 ) ) ;
#5497 = VECTOR ( 'NONE', #17865, 1000.000000000000000 ) ;
#5498 = VECTOR ( 'NONE', #7890, 1000.000000000000000 ) ;
#5499 = CARTESIAN_POINT ( 'NONE',  ( 9.707106781189999367, 19.99999999999999645, -43.10710678118599759 ) ) ;
#5500 = CARTESIAN_POINT ( 'NONE',  ( -5.017113268509455715, -1.250814956824373159, -0.6999999999999992895 ) ) ;
#5501 = CARTESIAN_POINT ( 'NONE',  ( -22.97554992469999746, 15.65135060219999907, 222.0000000000000000 ) ) ;
#5502 = CARTESIAN_POINT ( 'NONE',  ( -10.00000000000000000, -130.0000000000000000, -41.24671599790000442 ) ) ;
#5503 = CARTESIAN_POINT ( 'NONE',  ( -21.02347494288676444, 19.26966991725469214, 4.000000085000010586 ) ) ;
#5504 = CARTESIAN_POINT ( 'NONE',  ( -6.108812354267502798, 0.1812703649498176306, -13.78304957890000360 ) ) ;
#5505 = CARTESIAN_POINT ( 'NONE',  ( 4.420334067734101424, -4.199682076162645217, -30.05126389020000488 ) ) ;
#5506 = CARTESIAN_POINT ( 'NONE',  ( 1.638687372183706747, -17.80543024188206758, -28.79488058872038891 ) ) ;
#5507 = CLOSED_SHELL ( 'NONE', ( #28429, #14817, #24150, #7508, #9986, #22534, #15077, #15194, #6951, #26124, #12842, #22434, #21444, #14875, #6897, #15867, #20612, #20588, #12531, #20010, #23916, #13038, #2267, #9320, #21326, #960, #26760, #7656, #30412, #18005, #22339, #19436, #18350, #16036, #25526, #20667, #6380, #22676, #16756, #19261, #28327, #245, #101, #30474, #16107, #26480, #18032, #15998, #7988, #11945, #21408, #10580, #8252, #15543, #2848, #18734, #4241, #11078, #2759, #15297, #16883, #21597, #27136, #8346, #27876, #29077, #772, #5621, #28997, #3271, #28612, #15978, #19490, #22543, #3751, #28061, #20941, #4321 ) ) ;
#5508 = CARTESIAN_POINT ( 'NONE',  ( 27.79539923781684507, 0.5057481689249235801, 8.000000000000007105 ) ) ;
#5509 = DIRECTION ( 'NONE',  ( 0.000000000000000000, 0.000000000000000000, -1.000000000000000000 ) ) ;
#5510 = FACE_BOUND ( 'NONE', #12271, .T. ) ;
#5511 = CARTESIAN_POINT ( 'NONE',  ( -26.80000000000000071, -8.704148513059999178E-14, 230.6999999999999886 ) ) ;
#5512 = CARTESIAN_POINT ( 'NONE',  ( 4.266075142677475007, -0.9221078188639888484, -23.79036215650000230 ) ) ;
#5513 = ADVANCED_FACE ( 'NONE', ( #7858 ), #27349, .F. ) ;
#5514 = B_SPLINE_CURVE_WITH_KNOTS ( 'NONE', 5,
 ( #7755, #24754, #2737, #391, #12334, #19575, #17357, #5398, #22241 ),
 .UNSPECIFIED., .F., .F.,
 ( 6, 3, 6 ),
 ( 0.000000000000000000, 2.405120303699999962, 3.339306057409999973 ),
 .UNSPECIFIED. ) ;
#5515 = DIRECTION ( 'NONE',  ( -1.000000000000000000, -1.433034374091448024E-13, -1.199006074478416896E-12 ) ) ;
#5516 = CARTESIAN_POINT ( 'NONE',  ( -24.92639508767336309, -13.81781708088548122, 4.493023692000025271 ) ) ;
#5517 = CARTESIAN_POINT ( 'NONE',  ( 0.8959394325020000327, -28.48619164239999790, 224.3198498209999912 ) ) ;
#5518 = VERTEX_POINT ( 'NONE', #18031 ) ;
#5519 = CARTESIAN_POINT ( 'NONE',  ( 1.344125205454980154, -28.46870209102154448, 4.240358041999986227 ) ) ;
#5520 = LINE ( 'NONE', #20615, #22300 ) ;
#5521 = ORIENTED_EDGE ( 'NONE', *, *, #28501, .T. ) ;
#5522 = CYLINDRICAL_SURFACE ( 'NONE', #28903, 2.999999999999999112 ) ;
#5523 = DIRECTION ( 'NONE',  ( 0.000000000000000000, 0.000000000000000000, 1.000000000000000000 ) ) ;
#5524 = ORIENTED_EDGE ( 'NONE', *, *, #24708, .T. ) ;
#5525 = CARTESIAN_POINT ( 'NONE',  ( -4.861312627776431583, -9.716283824988348528, -32.74022090947522656 ) ) ;
#5526 = ORIENTED_EDGE ( 'NONE', *, *, #7540, .T. ) ;
#5527 = ORIENTED_EDGE ( 'NONE', *, *, #26629, .F. ) ;
#5528 = SURFACE_STYLE_USAGE ( .BOTH. , #15284 ) ;
#5529 = ORIENTED_EDGE ( 'NONE', *, *, #6615, .F. ) ;
#5530 = CARTESIAN_POINT ( 'NONE',  ( 28.49999999979999998, 4.812685681769999668, 229.2404163060000144 ) ) ;
#5531 = CARTESIAN_POINT ( 'NONE',  ( 2.131628207279999844E-14, -1.704192342799999938E-14, 230.7531949689999919 ) ) ;
#5532 = CARTESIAN_POINT ( 'NONE',  ( -3.607824829760114760, 0.2143012804528021953, -68.80033026170877974 ) ) ;
#5533 = VERTEX_POINT ( 'NONE', #502 ) ;
#5534 = CARTESIAN_POINT ( 'NONE',  ( -19.80526803560000104, 19.50877411510000314, 229.0000000000000000 ) ) ;
#5535 = AXIS2_PLACEMENT_3D ( 'NONE', #10541, #19676, #8154 ) ;
#5536 = CARTESIAN_POINT ( 'NONE',  ( -23.89299059146159010, -14.21221066648391052, 6.099998581000002140 ) ) ;
#5537 = DIRECTION ( 'NONE',  ( -1.000000000000000000, -1.601966730286662369E-12, -3.582312748438143944E-12 ) ) ;
#5538 = DIRECTION ( 'NONE',  ( 1.000000000000000000, 0.000000000000000000, 0.000000000000000000 ) ) ;
#5539 = EDGE_CURVE ( 'NONE', #27866, #9943, #28428, .T. ) ;
#5540 = CARTESIAN_POINT ( 'NONE',  ( -10.69999999994747064, -28.84009800776623678, -19.12627107572801677 ) ) ;
#5541 = CARTESIAN_POINT ( 'NONE',  ( -4.448701673712585070, 0.6187532242676665462, -19.25159460730001371 ) ) ;
#5542 = CARTESIAN_POINT ( 'NONE',  ( -1.127665019380140299, -28.47796022461074728, 224.8525238069234717 ) ) ;
#5543 = CARTESIAN_POINT ( 'NONE',  ( 24.26032293416166041, 13.57529002140354812, 5.676497403531009844 ) ) ;
#5544 = CARTESIAN_POINT ( 'NONE',  ( -12.38011772158675150, -28.51916434083160112, -33.29630834130933437 ) ) ;
#5545 = CARTESIAN_POINT ( 'NONE',  ( 27.72013230379999627, 7.265883530940000057, 222.0000000000000000 ) ) ;
#5546 = AXIS2_PLACEMENT_3D ( 'NONE', #1126, #4377, #21068 ) ;
#5547 = CARTESIAN_POINT ( 'NONE',  ( 10.69999999995574491, -32.31918898725707123, -22.79246800231758741 ) ) ;
#5548 = EDGE_CURVE ( 'NONE', #9016, #24581, #10295, .T. ) ;
#5549 = DIRECTION ( 'NONE',  ( 1.000000000000000000, -1.843431230200084908E-12, 2.650498504963248473E-12 ) ) ;
#5550 = CARTESIAN_POINT ( 'NONE',  ( 27.79999999980000069, 4.694479351150000035, 229.0000000000000000 ) ) ;
#5551 = CARTESIAN_POINT ( 'NONE',  ( 10.90985366930000033, -24.71798678640000091, -1.786271610999999648 ) ) ;
#5552 = EDGE_LOOP ( 'NONE', ( #22733, #20786, #28170, #15062 ) ) ;
#5553 = CARTESIAN_POINT ( 'NONE',  ( -4.499599993570057244, -1.182519567789861004, -55.70102360502500005 ) ) ;
#5554 = LINE ( 'NONE', #14707, #23379 ) ;
#5555 = B_SPLINE_CURVE_WITH_KNOTS ( 'NONE', 5,
 ( #23629, #21254, #21417, #31007, #2376, #7088, #11810, #21573, #171 ),
 .UNSPECIFIED., .F., .F.,
 ( 6, 3, 6 ),
 ( 0.000000000000000000, 0.7281981214720000262, 1.224410003600000074 ),
 .UNSPECIFIED. ) ;
#5556 = CARTESIAN_POINT ( 'NONE',  ( -21.63136441776463315, 17.21881425927816878, 0.08279823700002575393 ) ) ;
#5557 = CARTESIAN_POINT ( 'NONE',  ( -4.222392096712967557, 0.7175927990900473619, -68.10000000002500542 ) ) ;
#5558 = EDGE_CURVE ( 'NONE', #3580, #4546, #16464, .T. ) ;
#5559 = EDGE_LOOP ( 'NONE', ( #22727, #13586, #8208, #8068 ) ) ;
#5560 = ORIENTED_EDGE ( 'NONE', *, *, #28306, .F. ) ;
#5561 = ADVANCED_FACE ( 'NONE', ( #9374 ), #11745, .F. ) ;
#5562 = CARTESIAN_POINT ( 'NONE',  ( -0.5632927345598660596, 3.521042344314967210, -88.52261276241718235 ) ) ;
#5563 = EDGE_LOOP ( 'NONE', ( #17924, #26344, #25983, #11477 ) ) ;
#5564 = DIRECTION ( 'NONE',  ( 0.000000000000000000, 0.000000000000000000, 1.000000000000000000 ) ) ;
#5565 =( REPRESENTATION_RELATIONSHIP ('NONE','NONE', #2712, #16405 ) REPRESENTATION_RELATIONSHIP_WITH_TRANSFORMATION ( #20428 )SHAPE_REPRESENTATION_RELATIONSHIP( ) );
#5566 = CARTESIAN_POINT ( 'NONE',  ( 23.23955039760055641, 15.25661106415676471, 5.208368893000026034 ) ) ;
#5567 = ORIENTED_EDGE ( 'NONE', *, *, #18472, .F. ) ;
#5568 = CARTESIAN_POINT ( 'NONE',  ( -4.069925668896384963, 4.914984763948436530, -62.99933298482500277 ) ) ;
#5569 = CARTESIAN_POINT ( 'NONE',  ( -27.71720220699999970, -10.18334195910000162, 229.4485730569999760 ) ) ;
#5570 = PRODUCT_RELATED_PRODUCT_CATEGORY ( 'part', '', ( #4122 ) ) ;
#5571 = AXIS2_PLACEMENT_3D ( 'NONE', #9859, #7495, #17089 ) ;
#5572 = CARTESIAN_POINT ( 'NONE',  ( -27.03594125075309762, -0.4919295335570806893, -0.6999999999999784173 ) ) ;
#5573 = CYLINDRICAL_SURFACE ( 'NONE', #15534, 2.000000000000002665 ) ;
#5574 = CARTESIAN_POINT ( 'NONE',  ( -13.99999999969999820, 21.34999999960000139, -67.09999999999999432 ) ) ;
#5575 = CARTESIAN_POINT ( 'NONE',  ( -2.449212707639999657E-16, 2.000000000000000000, 230.8412452696274499 ) ) ;
#5576 = EDGE_LOOP ( 'NONE', ( #3828, #23182, #2175, #1277 ) ) ;
#5577 = UNCERTAINTY_MEASURE_WITH_UNIT (LENGTH_MEASURE( 1.000000000000000082E-05 ), #22570, 'distance_accuracy_value', 'NONE');
#5578 = CARTESIAN_POINT ( 'NONE',  ( 16.85920661228352557, -7.934045360712157269, -4.336808689942018722E-16 ) ) ;
#5579 = ADVANCED_FACE ( 'NONE', ( #11596 ), #12014, .F. ) ;
#5580 = CARTESIAN_POINT ( 'NONE',  ( 17.83930301670000418, 19.99998169580000251, 230.0000000000000000 ) ) ;
#5581 = ORIENTED_EDGE ( 'NONE', *, *, #23852, .F. ) ;
#5582 = CARTESIAN_POINT ( 'NONE',  ( 18.95046173579999760, -18.95046173579999760, 36.78285841159999592 ) ) ;
#5583 = DIRECTION ( 'NONE',  ( 1.000000000000000000, -1.843431230198065828E-12, 2.650498504953516580E-12 ) ) ;
#5584 = DIRECTION ( 'NONE',  ( 0.000000000000000000, 0.000000000000000000, 1.000000000000000000 ) ) ;
#5585 = CARTESIAN_POINT ( 'NONE',  ( 23.62697774660000150, -14.64965012220000062, 224.3193082299999901 ) ) ;
#5586 = CARTESIAN_POINT ( 'NONE',  ( 16.10001530720865759, -9.306175026709254894, -0.000000000000000000 ) ) ;
#5587 = CARTESIAN_POINT ( 'NONE',  ( 3.355053135122043173, -2.604011111845283111, -0.6999999999999992895 ) ) ;
#5588 = CARTESIAN_POINT ( 'NONE',  ( 23.68253874081223387, -20.17876519719180095, -0.2432540810000105580 ) ) ;
#5589 = CARTESIAN_POINT ( 'NONE',  ( -9.229093440751908517, -15.48814874182538226, -74.51555467487568762 ) ) ;
#5590 = FILL_AREA_STYLE_COLOUR ( '', #25868 ) ;
#5591 = CARTESIAN_POINT ( 'NONE',  ( -7.999999999674140660, -13.61361098168129224, -34.64062768038885309 ) ) ;
#5592 = EDGE_CURVE ( 'NONE', #19446, #4103, #29366, .T. ) ;
#5593 = VECTOR ( 'NONE', #16392, 1000.000000000000000 ) ;
#5594 = CARTESIAN_POINT ( 'NONE',  ( -24.31247271682646272, -11.33627354958356825, 93.21714158842222275 ) ) ;
#5595 = CARTESIAN_POINT ( 'NONE',  ( 3.861721477338985409, 1.529807325115373207, -38.22530605780803370 ) ) ;
#5596 = ORIENTED_EDGE ( 'NONE', *, *, #21169, .T. ) ;
#5597 = EDGE_CURVE ( 'NONE', #2860, #28481, #16154, .T. ) ;
#5598 = DIRECTION ( 'NONE',  ( -5.962915006522622422E-16, -0.4383711467890810676, -0.8987940462991651502 ) ) ;
#5599 = DIRECTION ( 'NONE',  ( 0.000000000000000000, 0.000000000000000000, -1.000000000000000000 ) ) ;
#5600 = CARTESIAN_POINT ( 'NONE',  ( 2.048088563388107186, 2.463427384171473999, -42.01846880737406309 ) ) ;
#5601 = ADVANCED_FACE ( 'NONE', ( #23718 ), #19043, .F. ) ;
#5602 = CARTESIAN_POINT ( 'NONE',  ( 1.815007998551255941, 5.706838904126064094, -60.94492395752499903 ) ) ;
#5603 = ORIENTED_EDGE ( 'NONE', *, *, #1163, .F. ) ;
#5604 = PRODUCT_DEFINITION ( 'UNKNOWN', '', #11850, #7480 ) ;
#5605 = B_SPLINE_CURVE_WITH_KNOTS ( 'NONE', 3,
 ( #25718, #15792, #18616, #4151, #13745, #1324, #1950, #11228, #4311, #23360 ),
 .UNSPECIFIED., .F., .F.,
 ( 4, 2, 2, 2, 4 ),
 ( 0.000000000000000000, 0.2500000000000000000, 0.5000000000000000000, 0.7500000000000000000, 1.000000000000000000 ),
 .UNSPECIFIED. ) ;
#5606 = ORIENTED_EDGE ( 'NONE', *, *, #23406, .T. ) ;
#5607 = CARTESIAN_POINT ( 'NONE',  ( 23.47715715134837211, -20.00370206646827498, 1.000000001000006522 ) ) ;
#5608 = ORIENTED_EDGE ( 'NONE', *, *, #14778, .T. ) ;
#5609 = VERTEX_POINT ( 'NONE', #28889 ) ;
#5610 = CARTESIAN_POINT ( 'NONE',  ( -3.290913549170359165, 1.665752135100502684, -41.62941659330974886 ) ) ;
#5611 = CARTESIAN_POINT ( 'NONE',  ( -23.25782843603512617, -13.31625947502723939, 226.1000000000011880 ) ) ;
#5612 = CIRCLE ( 'NONE', #114, 26.80000000000000071 ) ;
#5613 = B_SPLINE_CURVE_WITH_KNOTS ( 'NONE', 3,
 ( #22619, #15069, #19794, #5462, #29220, #5314 ),
 .UNSPECIFIED., .F., .F.,
 ( 4, 2, 4 ),
 ( 0.000000000000000000, 0.5000000000000000000, 1.000000000000000000 ),
 .UNSPECIFIED. ) ;
#5614 = CARTESIAN_POINT ( 'NONE',  ( -27.84772847483668912, 6.760385877827641110, 8.000000000000007105 ) ) ;
#5615 = EDGE_CURVE ( 'NONE', #26138, #9514, #5431, .T. ) ;
#5616 = CARTESIAN_POINT ( 'NONE',  ( 24.98823331316959440, -13.70626928515100573, 6.095967861000000987 ) ) ;
#5617 = DIRECTION ( 'NONE',  ( -0.8366600265317032381, 0.4922897737126532003, -0.2401057656573751253 ) ) ;
#5618 = VERTEX_POINT ( 'NONE', #17390 ) ;
#5619 = CARTESIAN_POINT ( 'NONE',  ( 2.852595256171609250, -3.624945453263371586, -44.10000000002499831 ) ) ;
#5620 = CARTESIAN_POINT ( 'NONE',  ( 8.000000000286558333, -7.565603753400573339, -31.48340496130054689 ) ) ;
#5621 = ADVANCED_FACE ( 'NONE', ( #26387 ), #14281, .T. ) ;
#5622 = CARTESIAN_POINT ( 'NONE',  ( 0.2540922009626206957, 4.794324758835501576, -23.88168644580000688 ) ) ;
#5623 = DIRECTION ( 'NONE',  ( -1.000000000000000000, 0.000000000000000000, 0.000000000000000000 ) ) ;
#5624 = CARTESIAN_POINT ( 'NONE',  ( -12.75378086759999796, -22.00000000000000000, -25.51324865357000249 ) ) ;
#5625 = CARTESIAN_POINT ( 'NONE',  ( 18.95046173579999760, -18.95046173579999760, 86.78285841159998881 ) ) ;
#5626 = CARTESIAN_POINT ( 'NONE',  ( -24.00375951252449269, -14.02501865426384775, 226.1000014189999376 ) ) ;
#5627 = CARTESIAN_POINT ( 'NONE',  ( 4.880217822150678231, -0.7240669684095875080, -45.38818262062500253 ) ) ;
#5628 = EDGE_CURVE ( 'NONE', #23079, #21601, #22435, .T. ) ;
#5629 = CARTESIAN_POINT ( 'NONE',  ( -16.57246140003591250, 12.07825306296973800, -1.400000000000001910 ) ) ;
#5630 = CARTESIAN_POINT ( 'NONE',  ( 7.833397470852297317, -25.63019328476620018, 207.3161515959309895 ) ) ;
#5631 = CARTESIAN_POINT ( 'NONE',  ( -18.62251649170634238, 19.99999711498608690, 230.6160300935700036 ) ) ;
#5632 =( GEOMETRIC_REPRESENTATION_CONTEXT ( 3 ) GLOBAL_UNCERTAINTY_ASSIGNED_CONTEXT ( ( #30485 ) ) GLOBAL_UNIT_ASSIGNED_CONTEXT ( ( #24196, #29213, #2638 ) ) REPRESENTATION_CONTEXT ( 'NONE', 'WORKASPACE' ) );
#5633 = CARTESIAN_POINT ( 'NONE',  ( -24.76259292740831697, -10.24958551592169265, 43.21714158839987618 ) ) ;
#5634 = VECTOR ( 'NONE', #24138, 1000.000000000000114 ) ;
#5635 = CARTESIAN_POINT ( 'NONE',  ( 24.34663841809999951, -12.78636765230000094, 225.0000000000000000 ) ) ;
#5636 = ORIENTED_EDGE ( 'NONE', *, *, #31002, .F. ) ;
#5637 = PRODUCT_DEFINITION_SHAPE ( 'NONE', 'NONE',  #4619 ) ;
#5638 = CARTESIAN_POINT ( 'NONE',  ( 2.831388952324535691, -5.386915550550475551, -33.80721934060000677 ) ) ;
#5639 = VERTEX_POINT ( 'NONE', #878 ) ;
#5640 = CARTESIAN_POINT ( 'NONE',  ( -8.699999999679551621, -14.62812833074668184, -33.38483337050165289 ) ) ;
#5641 = CARTESIAN_POINT ( 'NONE',  ( 5.363076718300177959, -2.525690298526013677, -52.29872167392500160 ) ) ;
#5642 = ORIENTED_EDGE ( 'NONE', *, *, #12325, .F. ) ;
#5643 = ORIENTED_EDGE ( 'NONE', *, *, #24613, .T. ) ;
#5644 = CARTESIAN_POINT ( 'NONE',  ( -33.37382699101617334, 1.330009658206147360, 234.8504245338175167 ) ) ;
#5645 = ORIENTED_EDGE ( 'NONE', *, *, #19399, .F. ) ;
#5646 = AXIS2_PLACEMENT_3D ( 'NONE', #24078, #14633, #9431 ) ;
#5647 = VERTEX_POINT ( 'NONE', #10776 ) ;
#5648 = FACE_OUTER_BOUND ( 'NONE', #21683, .T. ) ;
#5649 = CARTESIAN_POINT ( 'NONE',  ( -25.77914833258148164, -15.40383343755785361, 1.000000000000000888 ) ) ;
#5650 = CARTESIAN_POINT ( 'NONE',  ( -0.3637587985824408121, -27.79782236981992583, 5.677349366198735758 ) ) ;
#5651 = CARTESIAN_POINT ( 'NONE',  ( 2.434861079626372327, 4.402890713382674015, -35.69999999999999574 ) ) ;
#5652 = DIRECTION ( 'NONE',  ( 0.000000000000000000, 0.000000000000000000, 1.000000000000000000 ) ) ;
#5653 = LINE ( 'NONE', #27369, #13591 ) ;
#5654 = ADVANCED_FACE ( 'NONE', ( #3689 ), #17994, .F. ) ;
#5655 = CARTESIAN_POINT ( 'NONE',  ( -3.926812182872200907, 0.9533004182003812499, -0.6999999999999992895 ) ) ;
#5656 = CARTESIAN_POINT ( 'NONE',  ( 4.373195337096347224, -2.904765488536225515, 0.6412452698000004059 ) ) ;
#5657 = CIRCLE ( 'NONE', #14207, 2.000000000000000000 ) ;
#5658 = CARTESIAN_POINT ( 'NONE',  ( -26.87967798701711786, 4.135222155429991275, -0.6999999999999784173 ) ) ;
#5659 = CARTESIAN_POINT ( 'NONE',  ( 15.51050023680984502, 10.97998838177520931, -1.452769935612311825 ) ) ;
#5660 = CARTESIAN_POINT ( 'NONE',  ( 4.741512700999319208, 1.965332957690412385, -12.43011350020000272 ) ) ;
#5661 = CARTESIAN_POINT ( 'NONE',  ( -2.308365619037855421, -4.044857084274065429, -30.67642233980000199 ) ) ;
#5662 = ADVANCED_FACE ( 'NONE', ( #19915 ), #20375, .F. ) ;
#5663 = EDGE_CURVE ( 'NONE', #17781, #4165, #10788, .T. ) ;
#5664 = CARTESIAN_POINT ( 'NONE',  ( 17.18658402238548533, 9.900182044515950963, -0.6999999989999727834 ) ) ;
#5665 = CARTESIAN_POINT ( 'NONE',  ( -24.60699597083884171, -12.93667822868543738, 225.1470444808221885 ) ) ;
#5666 = CARTESIAN_POINT ( 'NONE',  ( -7.707106781243226123, -115.2381289094444128, 21.69251968763726879 ) ) ;
#5667 = PLANE ( 'NONE',  #10216 ) ;
#5668 = CARTESIAN_POINT ( 'NONE',  ( 24.26750084572334032, 13.69201430750461412, -0.6577119969999878357 ) ) ;
#5669 = LINE ( 'NONE', #22365, #7715 ) ;
#5670 = CARTESIAN_POINT ( 'NONE',  ( 27.51770821235203357, 4.728187301808492116, 1.000000000000000888 ) ) ;
#5671 = ORIENTED_EDGE ( 'NONE', *, *, #1024, .T. ) ;
#5672 = CARTESIAN_POINT ( 'NONE',  ( 17.16657240421717390, -9.000000000001264766, -0.6999999999999784173 ) ) ;
#5673 = CARTESIAN_POINT ( 'NONE',  ( 8.999999999770000869, 21.70000000000000284, -60.10000000000000142 ) ) ;
#5674 = ORIENTED_EDGE ( 'NONE', *, *, #17117, .T. ) ;
#5675 = CARTESIAN_POINT ( 'NONE',  ( 8.700000000133357503, -67.40749995146175877, -17.04319545392437263 ) ) ;
#5676 = DIRECTION ( 'NONE',  ( 5.962915006522623408E-16, 0.4383711467890811231, 0.8987940462991652613 ) ) ;
#5678 = ORIENTED_EDGE ( 'NONE', *, *, #19856, .F. ) ;
#5677 = CIRCLE ( 'NONE', #20755, 2.926829268290000119 ) ;
#5679 = CARTESIAN_POINT ( 'NONE',  ( -12.29999999969999891, -24.60885018109999933, -24.02302961593000319 ) ) ;
#5680 = ORIENTED_EDGE ( 'NONE', *, *, #27186, .T. ) ;
#5681 = VERTEX_POINT ( 'NONE', #29807 ) ;
#5682 = VERTEX_POINT ( 'NONE', #17540 ) ;
#5683 = CARTESIAN_POINT ( 'NONE',  ( 27.29823224869999976, 4.609747771270000349, 230.6577119970000069 ) ) ;
#5684 = ADVANCED_FACE ( 'NONE', ( #20072 ), #27447, .F. ) ;
#5685 = CARTESIAN_POINT ( 'NONE',  ( -17.70061747254754181, -9.691892145441446615, -0.6999999999999783062 ) ) ;
#5686 = CARTESIAN_POINT ( 'NONE',  ( 16.06675444876397307, -9.020011618195203695, -0.6999999999999784173 ) ) ;
#5687 = ADVANCED_FACE ( 'NONE', ( #8091 ), #28370, .F. ) ;
#5688 = ORIENTED_EDGE ( 'NONE', *, *, #25620, .T. ) ;
#5689 = LINE ( 'NONE', #19873, #16444 ) ;
#5690 = CARTESIAN_POINT ( 'NONE',  ( -24.36725163762951851, -13.38201776504032381, 5.146975365592536988 ) ) ;
#5691 = CARTESIAN_POINT ( 'NONE',  ( -7.707106507371444870, -5.692566414263196428, -27.29492500646317765 ) ) ;
#5692 = CARTESIAN_POINT ( 'NONE',  ( 4.638687372223565752, -11.03139726556875999, -35.43660304871379907 ) ) ;
#5693 = CIRCLE ( 'NONE', #4715, 2.000000000000000000 ) ;
#5694 = CARTESIAN_POINT ( 'NONE',  ( 4.080592064681261455, -5.083854565965863159, -3.705321867100007438 ) ) ;
#5695 = CARTESIAN_POINT ( 'NONE',  ( 4.979326355943800131, -2.377326608238005790, -19.88180150030000348 ) ) ;
#5696 = AXIS2_PLACEMENT_3D ( 'NONE', #27541, #8648, #18246 ) ;
#5697 = CARTESIAN_POINT ( 'NONE',  ( 27.79999999980000069, -7.282770092329999834, 229.0000000000000000 ) ) ;
#5698 = CARTESIAN_POINT ( 'NONE',  ( -8.000000000444114079, -28.22468611108740788, -31.13863906519029001 ) ) ;
#5699 = CARTESIAN_POINT ( 'NONE',  ( 2.781964183363350607, -2.771187371452367376, -92.88964426498925775 ) ) ;
#5700 = CARTESIAN_POINT ( 'NONE',  ( -25.84755624059999946, 9.037785233809998431, 230.6999999999999886 ) ) ;
#5701 = DIRECTION ( 'NONE',  ( 1.224606353819999829E-16, 1.000000000000000000, 0.000000000000000000 ) ) ;
#5702 = CARTESIAN_POINT ( 'NONE',  ( 1.783682052046414057, 3.046043134630439297, -0.6999999999999784173 ) ) ;
#5703 = DIRECTION ( 'NONE',  ( 0.000000000000000000, 0.000000000000000000, 1.000000000000000000 ) ) ;
#5704 = CARTESIAN_POINT ( 'NONE',  ( -24.49999999589999788, 3.000285566369999841E-15, 190.0000000000000000 ) ) ;
#5705 = ORIENTED_EDGE ( 'NONE', *, *, #1176, .F. ) ;
#5706 = CARTESIAN_POINT ( 'NONE',  ( -4.535753307212162078, -3.367775055652930227, -55.79895058492499516 ) ) ;
#5707 = LINE ( 'NONE', #12952, #2257 ) ;
#5708 = B_SPLINE_CURVE_WITH_KNOTS ( 'NONE', 3,
 ( #19725, #22087, #545, #28696, #10125, #21466 ),
 .UNSPECIFIED., .F., .F.,
 ( 4, 2, 4 ),
 ( 0.000000000000000000, 0.5000000000000000000, 1.000000000000000000 ),
 .UNSPECIFIED. ) ;
#5709 = CARTESIAN_POINT ( 'NONE',  ( 4.880902371519058036, -3.592936783560450653, -8.972776792900004850 ) ) ;
#5710 = CARTESIAN_POINT ( 'NONE',  ( -24.24144457387483698, -14.48500828217274439, -0.6999999999999784173 ) ) ;
#5711 = CARTESIAN_POINT ( 'NONE',  ( -4.502786141747646909, 1.045045138632145321, -68.10000000002500542 ) ) ;
#5712 = VECTOR ( 'NONE', #7340, 1000.000000000000000 ) ;
#5713 = ADVANCED_FACE ( 'NONE', ( #17682, #27298, #5741, #22592 ), #30784, .F. ) ;
#5714 = AXIS2_PLACEMENT_3D ( 'NONE', #12100, #17285, #21708 ) ;
#5715 = ORIENTED_EDGE ( 'NONE', *, *, #17830, .T. ) ;
#5716 = AXIS2_PLACEMENT_3D ( 'NONE', #816, #10406, #14977 ) ;
#5717 = VERTEX_POINT ( 'NONE', #16431 ) ;
#5718 = CARTESIAN_POINT ( 'NONE',  ( -0.7489034454876208891, 2.331869397845270253, -95.48173244568418738 ) ) ;
#5719 = ORIENTED_EDGE ( 'NONE', *, *, #24701, .F. ) ;
#5720 = COLOUR_RGB ( '', 0.31764706, 0.68627451, 0.89019608) ;
#5721 = CARTESIAN_POINT ( 'NONE',  ( -24.70074544867652122, 14.21822122508601716, 3.997190861000005313 ) ) ;
#5722 = CARTESIAN_POINT ( 'NONE',  ( -3.458129700889219116, 0.5397582531354577773, -85.94068374672499999 ) ) ;
#5723 = CARTESIAN_POINT ( 'NONE',  ( 0.9016190905398319133, 4.836326944446648568, -62.67744533512500738 ) ) ;
#5724 = EDGE_CURVE ( 'NONE', #16061, #24893, #3195, .T. ) ;
#5725 = CARTESIAN_POINT ( 'NONE',  ( 1.645560275461679600, -28.45273235262772005, 5.147476193076592210 ) ) ;
#5726 = B_SPLINE_CURVE_WITH_KNOTS ( 'NONE', 3,
 ( #28802, #21737, #9462, #19064, #17156, #17011 ),
 .UNSPECIFIED., .F., .F.,
 ( 4, 2, 4 ),
 ( 0.000000000000000000, 0.5000000000000000000, 1.000000000000000000 ),
 .UNSPECIFIED. ) ;
#5727 = B_SPLINE_CURVE_WITH_KNOTS ( 'NONE', 5,
 ( #15377, #27961, #1688, #27799, #18515, #6249, #25455, #6401, #10655 ),
 .UNSPECIFIED., .F., .F.,
 ( 6, 3, 6 ),
 ( -88.40979499649999696, -77.81866039000000512, -72.24467995679999888 ),
 .UNSPECIFIED. ) ;
#5728 = CARTESIAN_POINT ( 'NONE',  ( -21.27524652179786457, 16.93536700441368126, -0.6999999999999784173 ) ) ;
#5729 = CARTESIAN_POINT ( 'NONE',  ( -27.79999999999999716, -2.375185619369999834, 222.0000000000000000 ) ) ;
#5730 = DIRECTION ( 'NONE',  ( 0.3633921898465272138, -0.9316362575375356503, -2.312964634635741872E-15 ) ) ;
#5731 = CARTESIAN_POINT ( 'NONE',  ( 6.000000000000000000, -16.12030425626696939, -76.87399601051191667 ) ) ;
#5732 = ORIENTED_EDGE ( 'NONE', *, *, #4891, .T. ) ;
#5733 = CARTESIAN_POINT ( 'NONE',  ( 16.37473331892315542, -8.236461616552139375, 0.000000000000000000 ) ) ;
#5734 = VECTOR ( 'NONE', #22273, 1000.000000000000000 ) ;
#5735 = CARTESIAN_POINT ( 'NONE',  ( -26.80000000069999899, 3.281945028329999726E-15, 92.88981852279999885 ) ) ;
#5736 = VERTEX_POINT ( 'NONE', #26040 ) ;
#5737 = CARTESIAN_POINT ( 'NONE',  ( 14.55660443455950315, -32.00000000000113687, -30.75110051328497462 ) ) ;
#5738 = CARTESIAN_POINT ( 'NONE',  ( -23.85408962131194954, -14.27673465746016213, 6.098654221000004760 ) ) ;
#5739 = STYLED_ITEM ( 'NONE', ( #30462 ), #21644 ) ;
#5740 = VECTOR ( 'NONE', #13256, 1000.000000000000000 ) ;
#5741 = FACE_BOUND ( 'NONE', #21997, .T. ) ;
#5742 = CARTESIAN_POINT ( 'NONE',  ( 17.14656078599760392, 12.09981795542235439, -0.6999999989999727834 ) ) ;
#5743 = CARTESIAN_POINT ( 'NONE',  ( -26.79556473285982321, -0.4875557887250224209, 0.000000000000000000 ) ) ;
#5744 = DIRECTION ( 'NONE',  ( 0.7071067811870476172, 0.000000000000000000, 0.7071067811860475283 ) ) ;
#5745 = CARTESIAN_POINT ( 'NONE',  ( -4.708590264754340282, -31.20269148734607256, -0.2432540810000105580 ) ) ;
#5746 = FACE_OUTER_BOUND ( 'NONE', #28008, .T. ) ;
#5747 = ORIENTED_EDGE ( 'NONE', *, *, #19483, .T. ) ;
#5748 = EDGE_CURVE ( 'NONE', #14021, #14792, #23113, .T. ) ;
#5749 = CARTESIAN_POINT ( 'NONE',  ( -5.361385120510000490, 31.61859227569999931, 222.0000000000000000 ) ) ;
#5750 = CARTESIAN_POINT ( 'NONE',  ( -18.95046173579999760, -18.95046173579999760, 93.21714158839999698 ) ) ;
#5751 = CARTESIAN_POINT ( 'NONE',  ( 0.4125558677674681096, -28.49726274111934998, 6.095949245000009675 ) ) ;
#5752 = VERTEX_POINT ( 'NONE', #8876 ) ;
#5753 = CARTESIAN_POINT ( 'NONE',  ( 24.98081130624543889, 13.71897605842228529, 4.999998581000003384 ) ) ;
#5754 = SURFACE_STYLE_USAGE ( .BOTH. , #29677 ) ;
#5755 = FACE_OUTER_BOUND ( 'NONE', #30389, .T. ) ;
#5756 = DIRECTION ( 'NONE',  ( 0.000000000000000000, 0.000000000000000000, 1.000000000000000000 ) ) ;
#5757 = VECTOR ( 'NONE', #21437, 1000.000000000000000 ) ;
#5758 = CARTESIAN_POINT ( 'NONE',  ( 1.815007998551255941, 5.706838904126064094, -60.46492395752500215 ) ) ;
#5759 = VECTOR ( 'NONE', #1006, 1000.000000000000000 ) ;
#5760 = ORIENTED_EDGE ( 'NONE', *, *, #13547, .F. ) ;
#5761 = EDGE_CURVE ( 'NONE', #4001, #26442, #28546, .T. ) ;
#5762 = ORIENTED_EDGE ( 'NONE', *, *, #16574, .T. ) ;
#5763 = CARTESIAN_POINT ( 'NONE',  ( 13.88796284031055706, -26.65861513498057178, 0.02487559100000646950 ) ) ;
#5764 = ORIENTED_EDGE ( 'NONE', *, *, #27686, .T. ) ;
#5765 = CARTESIAN_POINT ( 'NONE',  ( 9.999999999979825915, -27.78524365354916981, -31.32191802991157914 ) ) ;
#5766 = CARTESIAN_POINT ( 'NONE',  ( -23.68723484211243147, -12.53725850803311914, 225.4947892886579552 ) ) ;
#5767 = CARTESIAN_POINT ( 'NONE',  ( -22.90527192528401201, 16.36193184990112570, 5.200000000000009948 ) ) ;
#5768 = B_SPLINE_CURVE_WITH_KNOTS ( 'NONE', 3,
 ( #13471, #13949, #27954, #11736 ),
 .UNSPECIFIED., .F., .F.,
 ( 4, 4 ),
 ( 0.000000000000000000, 1.000000000000000000 ),
 .UNSPECIFIED. ) ;
#5769 = CARTESIAN_POINT ( 'NONE',  ( 8.700000000279912271, -18.16707915929421446, -36.73187106089413589 ) ) ;
#5770 = DIRECTION ( 'NONE',  ( -1.000000000000000000, 5.687698019339887572E-16, -6.771501495046482653E-12 ) ) ;
#5771 = VECTOR ( 'NONE', #15372, 1000.000000000000000 ) ;
#5772 = CYLINDRICAL_SURFACE ( 'NONE', #29592, 1.099999999999999867 ) ;
#5773 = ORIENTED_EDGE ( 'NONE', *, *, #18876, .F. ) ;
#5774 = CARTESIAN_POINT ( 'NONE',  ( 2.725151615585481135, -3.829855452310775288, -44.10000000002499121 ) ) ;
#5775 = EDGE_CURVE ( 'NONE', #22456, #368, #25732, .T. ) ;
#5776 = CARTESIAN_POINT ( 'NONE',  ( 3.805567437367120665, -2.527735466695482991, -0.7070437319000487664 ) ) ;
#5777 = ADVANCED_FACE ( 'NONE', ( #2119 ), #9164, .F. ) ;
#5778 = CARTESIAN_POINT ( 'NONE',  ( 4.081868536579633222, 3.119100555900671257, -24.30477430109999659 ) ) ;
#5779 = CARTESIAN_POINT ( 'NONE',  ( 9.799999999997906386, -15.94902145823454198, -35.53273252495090873 ) ) ;
#5780 = CARTESIAN_POINT ( 'NONE',  ( -27.23548386990000125, 3.335274659649999582E-15, 188.3395398260000206 ) ) ;
#5781 =( NAMED_UNIT ( * ) SI_UNIT ( $, .STERADIAN. ) SOLID_ANGLE_UNIT ( ) );
#5782 = AXIS2_PLACEMENT_3D ( 'NONE', #13214, #20305, #1278 ) ;
#5783 = DIRECTION ( 'NONE',  ( 0.000000000000000000, 0.000000000000000000, -1.000000000000000000 ) ) ;
#5784 = CARTESIAN_POINT ( 'NONE',  ( -3.948109860491266776, 2.321589337205137937, -44.44354844312501029 ) ) ;
#5785 = EDGE_CURVE ( 'NONE', #23190, #24264, #26503, .T. ) ;
#5786 = B_SPLINE_CURVE_WITH_KNOTS ( 'NONE', 3,
 ( #4054, #23255, #1385, #10980, #30497, #6561 ),
 .UNSPECIFIED., .F., .F.,
 ( 4, 2, 4 ),
 ( 0.000000000000000000, 0.5000000000000000000, 1.000000000000000000 ),
 .UNSPECIFIED. ) ;
#5788 = CARTESIAN_POINT ( 'NONE',  ( 13.00000000000000000, 23.81663212713006672, -62.33813991915980779 ) ) ;
#5787 = B_SPLINE_CURVE_WITH_KNOTS ( 'NONE', 1,
 ( #22291, #27461 ),
 .UNSPECIFIED., .F., .F.,
 ( 2, 2 ),
 ( -2.557517344899999924E-06, 0.7000000000009999335 ),
 .UNSPECIFIED. ) ;
#5789 = DIRECTION ( 'NONE',  ( 0.9316362575375356503, 0.3633921898465274913, 0.000000000000000000 ) ) ;
#5790 = CARTESIAN_POINT ( 'NONE',  ( -18.57884138570541310, 20.00001926002121166, 230.6254606444483386 ) ) ;
#5791 = CARTESIAN_POINT ( 'NONE',  ( -24.76914019444431858, -10.23375669952357470, 43.21714158839954933 ) ) ;
#5792 = CARTESIAN_POINT ( 'NONE',  ( 9.543143524407904366, -25.04338540923419743, 26.16054379342799052 ) ) ;
#5793 = ORIENTED_EDGE ( 'NONE', *, *, #106, .T. ) ;
#5794 = CARTESIAN_POINT ( 'NONE',  ( 4.417684705200791484, 4.247747620870205409, -35.32341724620000178 ) ) ;
#5795 = ADVANCED_FACE ( 'NONE', ( #9184, #1816 ), #11246, .F. ) ;
#5796 = EDGE_LOOP ( 'NONE', ( #6690, #14912, #10472, #17055 ) ) ;
#5797 = CYLINDRICAL_SURFACE ( 'NONE', #10273, 10.00000000000001421 ) ;
#5798 = CARTESIAN_POINT ( 'NONE',  ( -5.649653782182448403, -1.974543963569185046, -50.40743646232499486 ) ) ;
#5799 = ORIENTED_EDGE ( 'NONE', *, *, #12141, .F. ) ;
#5800 = ORIENTED_EDGE ( 'NONE', *, *, #9438, .T. ) ;
#5801 = DIRECTION ( 'NONE',  ( 1.204160931909535721E-17, -1.000000000000000000, -4.194226097600296644E-17 ) ) ;
#5802 = ORIENTED_EDGE ( 'NONE', *, *, #13633, .T. ) ;
#5803 = ORIENTED_EDGE ( 'NONE', *, *, #412, .T. ) ;
#5804 = CARTESIAN_POINT ( 'NONE',  ( 24.43659368183839931, 14.66646236428692340, 3.899998581000013509 ) ) ;
#5805 = EDGE_CURVE ( 'NONE', #3582, #14877, #27871, .T. ) ;
#5806 = CARTESIAN_POINT ( 'NONE',  ( 0.2237522039478089808, -27.79962635424878314, 6.073211979320773501 ) ) ;
#5807 = CARTESIAN_POINT ( 'NONE',  ( 4.455580650938469667, 2.746354562282469214, -35.69999999999999574 ) ) ;
#5808 = FACE_OUTER_BOUND ( 'NONE', #3876, .T. ) ;
#5809 = CARTESIAN_POINT ( 'NONE',  ( -22.36167894509999954, 17.71395549689999882, 224.0000000000000000 ) ) ;
#5810 = CARTESIAN_POINT ( 'NONE',  ( -4.772771908274402008, 1.289969644746177035, -0.6999999999999992895 ) ) ;
#5811 = CARTESIAN_POINT ( 'NONE',  ( 2.445722248254770026, -3.773326582131152573, 0.7715606116999971231 ) ) ;
#5812 = CARTESIAN_POINT ( 'NONE',  ( -10.00000000021355184, -29.62135916506342070, -29.91085694111316329 ) ) ;
#5813 = CARTESIAN_POINT ( 'NONE',  ( -22.97723753882890918, 16.89265275057793403, 7.000000021000013284 ) ) ;
#5814 = B_SPLINE_CURVE_WITH_KNOTS ( 'NONE', 5,
 ( #17636, #27248, #3021, #12613, #8188, #22225, #3323, #12928, #7885, #983, #10573, #25045 ),
 .UNSPECIFIED., .F., .F.,
 ( 6, 3, 3, 6 ),
 ( 2.782752057450000205, 3.293393370880000059, 4.940089941930000172, 5.565010780509999755 ),
 .UNSPECIFIED. ) ;
#5815 = CARTESIAN_POINT ( 'NONE',  ( -0.6370991518874352666, 4.292107257743940529, -10.86772091660000150 ) ) ;
#5816 = CARTESIAN_POINT ( 'NONE',  ( -5.864216825196034932, 1.669623860970033347, -31.30158078969999380 ) ) ;
#5817 = CARTESIAN_POINT ( 'NONE',  ( -13.99999999968414777, 21.69999999999800622, -58.04802220338182650 ) ) ;
#5818 = DIRECTION ( 'NONE',  ( -1.000000000000000000, 0.000000000000000000, 0.000000000000000000 ) ) ;
#5819 = CARTESIAN_POINT ( 'NONE',  ( 14.60916111670818474, -28.04296597385482315, 1.000000000000000888 ) ) ;
#5820 = CARTESIAN_POINT ( 'NONE',  ( 0.2402089773019999985, -27.79941220630000132, 226.0797949779999954 ) ) ;
#5821 = CARTESIAN_POINT ( 'NONE',  ( -3.253989917302559043, -2.899813084402115049, -24.84101932450000305 ) ) ;
#5822 = CARTESIAN_POINT ( 'NONE',  ( 24.50249477284852517, 13.82460068605435666, -0.5592437529999827461 ) ) ;
#5823 = CARTESIAN_POINT ( 'NONE',  ( 27.75695160380879045, 2.618790587931635994, 1.000000000000000888 ) ) ;
#5824 = ORIENTED_EDGE ( 'NONE', *, *, #27706, .T. ) ;
#5825 = ORIENTED_EDGE ( 'NONE', *, *, #18275, .T. ) ;
#5826 = DIRECTION ( 'NONE',  ( 0.000000000000000000, 1.000000000000000000, 0.000000000000000000 ) ) ;
#5827 = CARTESIAN_POINT ( 'NONE',  ( 0.000000000000000000, 0.000000000000000000, 40.00000000000000000 ) ) ;
#5828 = VERTEX_POINT ( 'NONE', #16121 ) ;
#5829 = CARTESIAN_POINT ( 'NONE',  ( -7.999999999655180716, -13.66682223735657864, -36.55330428419717492 ) ) ;
#5830 = CARTESIAN_POINT ( 'NONE',  ( 7.999488503669390127, -115.5102744061023543, 21.08394882064870401 ) ) ;
#5831 = EDGE_CURVE ( 'NONE', #27161, #20099, #26801, .T. ) ;
#5832 = VERTEX_POINT ( 'NONE', #21627 ) ;
#5833 = CARTESIAN_POINT ( 'NONE',  ( -0.6805621215738131280, -26.79155678488164938, 4.123352033172330344 ) ) ;
#5834 = VERTEX_POINT ( 'NONE', #23837 ) ;
#5835 = EDGE_LOOP ( 'NONE', ( #4195, #17599, #15897, #3887 ) ) ;
#5836 = EDGE_CURVE ( 'NONE', #25912, #6569, #26119, .T. ) ;
#5837 = EDGE_LOOP ( 'NONE', ( #13417, #29365, #182, #23435 ) ) ;
#5838 = CARTESIAN_POINT ( 'NONE',  ( 9.897162125403639266, -25.37356426577971646, 41.66046017469999896 ) ) ;
#5839 = EDGE_CURVE ( 'NONE', #13159, #9489, #388, .T. ) ;
#5840 = DIRECTION ( 'NONE',  ( 1.000000000000000000, -1.224606353819999582E-16, 0.000000000000000000 ) ) ;
#5841 = CARTESIAN_POINT ( 'NONE',  ( 2.020725942159999899, 3.500000000000000000, 230.8412452700000017 ) ) ;
#5842 = CARTESIAN_POINT ( 'NONE',  ( 8.999999999770000869, 20.99999999999999645, -56.09999999999999432 ) ) ;
#5843 =( LENGTH_UNIT ( ) NAMED_UNIT ( * ) SI_UNIT ( .MILLI., .METRE. ) );
#5844 = CARTESIAN_POINT ( 'NONE',  ( -24.23284209150707369, -13.62399916074796202, 5.732688422242026682 ) ) ;
#5845 = CARTESIAN_POINT ( 'NONE',  ( 19.80526555982327608, 19.50877392092707296, 0.9260799790000162623 ) ) ;
#5846 = CARTESIAN_POINT ( 'NONE',  ( 2.100000000115434418, -0.2748893566605633554, 226.6412452697800575 ) ) ;
#5847 = CARTESIAN_POINT ( 'NONE',  ( 6.105340317846409626, -0.2107885887935728730, -2.685409721200002320 ) ) ;
#5848 = CARTESIAN_POINT ( 'NONE',  ( 3.244870203142138809, 3.966006825147196047, -19.31872222229999991 ) ) ;
#5849 = CARTESIAN_POINT ( 'NONE',  ( 3.550686847520000117E-05, -28.50022181210000127, 223.9000014189999774 ) ) ;
#5850 = CARTESIAN_POINT ( 'NONE',  ( -0.1477568774490881365, -27.50000000000000711, 6.100000000000010303 ) ) ;
#5851 = CARTESIAN_POINT ( 'NONE',  ( 25.11738521000000190, -13.46751580659999981, 224.3193205009999929 ) ) ;
#5852 = CARTESIAN_POINT ( 'NONE',  ( -27.29823224869999976, 4.602902183869999497, 230.6577119970000069 ) ) ;
#5853 = DIRECTION ( 'NONE',  ( 0.000000000000000000, 0.000000000000000000, -1.000000000000000000 ) ) ;
#5854 = CARTESIAN_POINT ( 'NONE',  ( 27.79999999980000069, -7.282770092339999835, 222.0000000000000000 ) ) ;
#5855 = CARTESIAN_POINT ( 'NONE',  ( -25.89944370639999960, -7.563310173900000599, 230.6999999999999886 ) ) ;
#5856 = CARTESIAN_POINT ( 'NONE',  ( 3.861721477338983632, 0.2146938847481238977, -40.92168819670553148 ) ) ;
#5857 = ORIENTED_EDGE ( 'NONE', *, *, #21179, .F. ) ;
#5858 = CARTESIAN_POINT ( 'NONE',  ( -5.463799992266447525, -1.435916617982112342, -56.45102360502500005 ) ) ;
#5859 = CARTESIAN_POINT ( 'NONE',  ( -9.738910687886855655, -24.96785170200598714, 36.78285841123146582 ) ) ;
#5860 = CARTESIAN_POINT ( 'NONE',  ( 1.942707423728255778, -5.758494596869851989, -15.26414732020000464 ) ) ;
#5861 = EDGE_LOOP ( 'NONE', ( #18459, #27736, #10262, #9953 ) ) ;
#5862 = CARTESIAN_POINT ( 'NONE',  ( 26.97469346668950152, -9.357175201752722771, -0.6999999999999784173 ) ) ;
#5863 = CARTESIAN_POINT ( 'NONE',  ( -4.248672686832829726, 0.9089880553856074519, -68.10000000002501963 ) ) ;
#5864 = VERTEX_POINT ( 'NONE', #19572 ) ;
#5865 = ORIENTED_EDGE ( 'NONE', *, *, #713, .F. ) ;
#5866 = ORIENTED_EDGE ( 'NONE', *, *, #8704, .T. ) ;
#5867 = CARTESIAN_POINT ( 'NONE',  ( 3.401975299758845050, 1.201107343883199841, -91.64589571366730070 ) ) ;
#5868 = VERTEX_POINT ( 'NONE', #12475 ) ;
#5869 = CARTESIAN_POINT ( 'NONE',  ( -7.797918471980000099, -130.0000000000000000, -43.60208152801600079 ) ) ;
#5870 = EDGE_CURVE ( 'NONE', #23873, #9948, #21938, .T. ) ;
#5871 = DIRECTION ( 'NONE',  ( 0.3633921898465291567, 0.9316362575375349842, 0.000000000000000000 ) ) ;
#5872 = CARTESIAN_POINT ( 'NONE',  ( -5.973670867983248201, -0.3179945487330332332, -65.56421022022500722 ) ) ;
#5873 = CARTESIAN_POINT ( 'NONE',  ( -27.79999999970000246, -10.21376199200000201, 229.1414213560000235 ) ) ;
#5874 = CIRCLE ( 'NONE', #4384, 2.999999999999998668 ) ;
#5875 = AXIS2_PLACEMENT_3D ( 'NONE', #8947, #18546, #15710 ) ;
#5876 = CARTESIAN_POINT ( 'NONE',  ( -27.64451936256318376, 4.252886846324511083, -0.5592437529999827461 ) ) ;
#5877 = CARTESIAN_POINT ( 'NONE',  ( 10.69999999930000101, -24.87867965640000278, -26.27867965640000136 ) ) ;
#5878 =( GEOMETRIC_REPRESENTATION_CONTEXT ( 3 ) GLOBAL_UNCERTAINTY_ASSIGNED_CONTEXT ( ( #22617 ) ) GLOBAL_UNIT_ASSIGNED_CONTEXT ( ( #10311, #3213, #8081 ) ) REPRESENTATION_CONTEXT ( 'NONE', 'WORKASPACE' ) );
#5879 = DIRECTION ( 'NONE',  ( 1.000000000000000000, 0.000000000000000000, 0.000000000000000000 ) ) ;
#5880 = DIRECTION ( 'NONE',  ( -0.8660254037843290176, 0.5000000000001899592, -1.018673689593249976E-32 ) ) ;
#5881 = EDGE_LOOP ( 'NONE', ( #22589, #5212, #22489, #7323, #423 ) ) ;
#5882 = CARTESIAN_POINT ( 'NONE',  ( -5.299969906037439671, -1.662641516789540086, -9.023230888999997035 ) ) ;
#5883 = CARTESIAN_POINT ( 'NONE',  ( -10.00000000000000000, 20.99999999999999645, -64.10000000019999788 ) ) ;
#5884 = CARTESIAN_POINT ( 'NONE',  ( -11.50000000044500048, -30.20000000000000284, -28.40000000000542002 ) ) ;
#5885 = ORIENTED_EDGE ( 'NONE', *, *, #3172, .T. ) ;
#5886 = FACE_OUTER_BOUND ( 'NONE', #2256, .T. ) ;
#5887 = CARTESIAN_POINT ( 'NONE',  ( -24.47278419579111386, -14.60601539740217092, 6.095965388000001539 ) ) ;
#5888 = CARTESIAN_POINT ( 'NONE',  ( -28.50000000000000000, 4.144832625269998950E-15, 229.0000000000000000 ) ) ;
#5889 = CARTESIAN_POINT ( 'NONE',  ( 23.95030481189679605, 13.51304758006065043, 0.000000000000000000 ) ) ;
#5890 = CARTESIAN_POINT ( 'NONE',  ( 16.40303402077768169, -9.791839085275103827, 0.000000000000000000 ) ) ;
#5891 = CARTESIAN_POINT ( 'NONE',  ( -6.340437944841875506, 0.6332316896323284539, -47.62737393802499497 ) ) ;
#5892 = AXIS2_PLACEMENT_3D ( 'NONE', #22649, #8622, #10540 ) ;
#5893 = CARTESIAN_POINT ( 'NONE',  ( 27.79999999999999716, 2.355804440410000085E-11, 229.0000000000000000 ) ) ;
#5894 = DIRECTION ( 'NONE',  ( 1.000000000000000000, -1.843431230198065828E-12, 2.650498504953516580E-12 ) ) ;
#5895 = VERTEX_POINT ( 'NONE', #19728 ) ;
#5896 = CARTESIAN_POINT ( 'NONE',  ( 23.77947513710800109, -14.40125623032519719, 4.791564337000009388 ) ) ;
#5897 = CARTESIAN_POINT ( 'NONE',  ( -21.16705332929999983, 21.30254446269999846, 222.0000000000000000 ) ) ;
#5898 = ADVANCED_FACE ( 'NONE', ( #548 ), #4938, .F. ) ;
#5899 = STYLED_ITEM ( 'NONE', ( #19168 ), #11026 ) ;
#5900 = AXIS2_PLACEMENT_3D ( 'NONE', #14288, #24651, #14748 ) ;
#5901 = CARTESIAN_POINT ( 'NONE',  ( -22.81399828927099449, -14.09994392937125518, 93.21714158846111786 ) ) ;
#5902 = CARTESIAN_POINT ( 'NONE',  ( -1.903575822388091643, -3.411965078385457595, -68.10000000002500542 ) ) ;
#5903 = CARTESIAN_POINT ( 'NONE',  ( -9.999999999959999997, -36.62914859500000375, -26.86371135770000151 ) ) ;
#5904 =( LENGTH_UNIT ( ) NAMED_UNIT ( * ) SI_UNIT ( .MILLI., .METRE. ) );
#5905 = CARTESIAN_POINT ( 'NONE',  ( 14.78499923084739720, -23.58415079274018566, -32.20104664978513398 ) ) ;
#5906 = CYLINDRICAL_SURFACE ( 'NONE', #31053, 1.000000000000000888 ) ;
#5907 = CARTESIAN_POINT ( 'NONE',  ( -1.494970809075166329, -6.161113191638062148, -61.94311227092499195 ) ) ;
#5908 = EDGE_LOOP ( 'NONE', ( #6312, #25168, #14333, #14844 ) ) ;
#5909 = CARTESIAN_POINT ( 'NONE',  ( 18.59546134273585594, 19.99999462727945243, 230.6223120414987875 ) ) ;
#5910 = VECTOR ( 'NONE', #28995, 1000.000000000000000 ) ;
#5911 = VERTEX_POINT ( 'NONE', #14393 ) ;
#5912 = CIRCLE ( 'NONE', #420, 4.000000000000000888 ) ;
#5913 = CARTESIAN_POINT ( 'NONE',  ( 13.96766655902600185, -26.81162144411387160, 0.08279888700002402402 ) ) ;
#5914 = ORIENTED_EDGE ( 'NONE', *, *, #4289, .T. ) ;
#5915 = EDGE_CURVE ( 'NONE', #11396, #3695, #9973, .T. ) ;
#5916 = DIRECTION ( 'NONE',  ( 0.000000000000000000, -2.257145581549999994E-12, -1.000000000000000000 ) ) ;
#5917 = CARTESIAN_POINT ( 'NONE',  ( -23.31771987846477145, -13.21065015015469868, 226.0876905690154786 ) ) ;
#5918 = CARTESIAN_POINT ( 'NONE',  ( -23.25788685383075460, -13.43083806724684770, 143.2171415880000040 ) ) ;
#5919 = AXIS2_PLACEMENT_3D ( 'NONE', #9127, #13387, #20469 ) ;
#5920 = FACE_OUTER_BOUND ( 'NONE', #14485, .T. ) ;
#5921 = AXIS2_PLACEMENT_3D ( 'NONE', #14394, #14699, #28846 ) ;
#5922 = CARTESIAN_POINT ( 'NONE',  ( -24.49999999589999788, 3.000285566369999841E-15, 90.00000000000000000 ) ) ;
#5923 = DIRECTION ( 'NONE',  ( 1.000000000000000000, 0.000000000000000000, 0.000000000000000000 ) ) ;
#5924 = ORIENTED_EDGE ( 'NONE', *, *, #5060, .T. ) ;
#5925 = LINE ( 'NONE', #22934, #27556 ) ;
#5926 = CARTESIAN_POINT ( 'NONE',  ( -15.44356573478999906, -26.99999999999999289, -28.40000000003211866 ) ) ;
#5927 = EDGE_CURVE ( 'NONE', #1828, #4237, #14232, .T. ) ;
#5928 = CARTESIAN_POINT ( 'NONE',  ( 3.375516224911109031, -2.766870103071180420, -24.49674734060000247 ) ) ;
#5929 = FACE_OUTER_BOUND ( 'NONE', #24195, .T. ) ;
#5930 = CARTESIAN_POINT ( 'NONE',  ( 19.80538173989999962, 19.50875420239999869, 227.7999999360000061 ) ) ;
#5931 =( NAMED_UNIT ( * ) PLANE_ANGLE_UNIT ( ) SI_UNIT ( $, .RADIAN. ) );
#5932 = CARTESIAN_POINT ( 'NONE',  ( -23.93349116070633542, -14.14448167692421876, 226.0729041749974044 ) ) ;
#5933 = CARTESIAN_POINT ( 'NONE',  ( 0.7970308137830555140, -5.845159207773487076, -48.96468436622500775 ) ) ;
#5934 = EDGE_CURVE ( 'NONE', #25869, #27389, #7332, .T. ) ;
#5935 = CONICAL_SURFACE ( 'NONE', #5446, 1.472846691535505848, 0.3390887027916915653 ) ;
#5936 = DIRECTION ( 'NONE',  ( 0.000000000000000000, 0.000000000000000000, -1.000000000000000000 ) ) ;
#5937 = DIRECTION ( 'NONE',  ( 1.000000000000000000, -1.843431230208684678E-12, 2.650498504958264790E-12 ) ) ;
#5938 = CARTESIAN_POINT ( 'NONE',  ( -19.88589761007506596, 20.00023699978923730, 229.9605059376604856 ) ) ;
#5939 = FACE_OUTER_BOUND ( 'NONE', #10917, .T. ) ;
#5940 = CARTESIAN_POINT ( 'NONE',  ( 18.13765659380263884, -9.536403318364705228, -4.336808689942018722E-16 ) ) ;
#5941 = VERTEX_POINT ( 'NONE', #21470 ) ;
#5942 = CARTESIAN_POINT ( 'NONE',  ( -3.554763430470064822, 2.566410659217317924, -34.46696136359999940 ) ) ;
#5943 = AXIS2_PLACEMENT_3D ( 'NONE', #15885, #13838, #6747 ) ;
#5944 = VERTEX_POINT ( 'NONE', #19260 ) ;
#5945 = EDGE_CURVE ( 'NONE', #28212, #16979, #16737, .T. ) ;
#5946 = DIRECTION ( 'NONE',  ( 1.000000000000000000, 5.998481157687279274E-24, -2.257150022441830001E-12 ) ) ;
#5947 = CARTESIAN_POINT ( 'NONE',  ( 4.545032752014868116, -0.3361547907463890428, -49.52442242802500516 ) ) ;
#5948 = ORIENTED_EDGE ( 'NONE', *, *, #8522, .T. ) ;
#5949 = EDGE_CURVE ( 'NONE', #24427, #1634, #21992, .T. ) ;
#5950 = PRODUCT_CONTEXT ( 'NONE', #26256, 'mechanical' ) ;
#5951 = VERTEX_POINT ( 'NONE', #10734 ) ;
#5952 = VERTEX_POINT ( 'NONE', #12791 ) ;
#5953 = CARTESIAN_POINT ( 'NONE',  ( 24.97472003062369694, 13.73006752330286595, 4.791638082000004850 ) ) ;
#5954 = CARTESIAN_POINT ( 'NONE',  ( 16.06675444873834380, 10.97998838177521286, -1.000005633855494125E-09 ) ) ;
#5955 = CARTESIAN_POINT ( 'NONE',  ( 1.854139248850241950, 4.609273058799894685, -35.69999999999998153 ) ) ;
#5956 = AXIS2_PLACEMENT_3D ( 'NONE', #7784, #9688, #19291 ) ;
#5957 = EDGE_CURVE ( 'NONE', #19471, #4565, #29772, .T. ) ;
#5958 = FACE_OUTER_BOUND ( 'NONE', #26778, .T. ) ;
#5959 = DIRECTION ( 'NONE',  ( 1.224606353819999829E-16, 1.000000000000000000, 0.000000000000000000 ) ) ;
#5960 = CARTESIAN_POINT ( 'NONE',  ( -4.214204818414113873, 2.192735554227209338, -0.6999999999999992895 ) ) ;
#5961 = CARTESIAN_POINT ( 'NONE',  ( -1.949381390262891589, -5.750991590113663676, -0.5756305127000010957 ) ) ;
#5962 = CARTESIAN_POINT ( 'NONE',  ( -4.041451884379999804, 9.156941871420000667E-11, 227.9588918784999976 ) ) ;
#5963 = LINE ( 'NONE', #10690, #12487 ) ;
#5964 = ORIENTED_EDGE ( 'NONE', *, *, #14825, .T. ) ;
#5965 = CARTESIAN_POINT ( 'NONE',  ( 5.459923716313909381, 2.263110678531865094, -12.49261350019999384 ) ) ;
#5966 = CARTESIAN_POINT ( 'NONE',  ( 0.08264113651937701754, -4.780899355463231970, -32.47360030499999795 ) ) ;
#5968 = EDGE_CURVE ( 'NONE', #25254, #9917, #22841, .T. ) ;
#5967 = VECTOR ( 'NONE', #22471, 1000.000000000000000 ) ;
#5969 = DIRECTION ( 'NONE',  ( -1.000000000000000000, 1.224606353819999829E-16, 0.000000000000000000 ) ) ;
#5970 = DIRECTION ( 'NONE',  ( 0.2815395311429195746, 0.9595496299847261490, 0.000000000000000000 ) ) ;
#5971 =( LENGTH_UNIT ( ) NAMED_UNIT ( * ) SI_UNIT ( .MILLI., .METRE. ) );
#5972 = CARTESIAN_POINT ( 'NONE',  ( -9.738910687886855655, -24.96785170200598714, 202.0000000000000000 ) ) ;
#5973 = CARTESIAN_POINT ( 'NONE',  ( 3.157381476932438868, -2.999772911539577702, -30.05126389020000488 ) ) ;
#5974 = CARTESIAN_POINT ( 'NONE',  ( 18.94276248278926289, 21.23709850769745699, 0.5017677510000262409 ) ) ;
#5975 = CARTESIAN_POINT ( 'NONE',  ( 4.041451884379999804, -9.156941871420000667E-11, 229.2412452703699728 ) ) ;
#5976 = CARTESIAN_POINT ( 'NONE',  ( -27.76135144259999876, 3.399672736729999754E-15, 92.33858589269999584 ) ) ;
#5977 = ORIENTED_EDGE ( 'NONE', *, *, #7255, .T. ) ;
#5978 = EDGE_LOOP ( 'NONE', ( #26617, #17970, #3199, #30382 ) ) ;
#5979 = EDGE_CURVE ( 'NONE', #9833, #25397, #28002, .T. ) ;
#5980 = AXIS2_PLACEMENT_3D ( 'NONE', #20850, #23681, #4322 ) ;
#5981 = CARTESIAN_POINT ( 'NONE',  ( 23.81776757409229361, 15.65134803726813217, 5.104183903999998329 ) ) ;
#5982 = DIRECTION ( 'NONE',  ( -0.5000000000001898481, -0.8660254037843291286, 0.000000000000000000 ) ) ;
#5983 = ORIENTED_EDGE ( 'NONE', *, *, #22188, .F. ) ;
#5984 = CARTESIAN_POINT ( 'NONE',  ( -1.086409579022823424, -3.500000000000000000, 227.7407790647054071 ) ) ;
#5985 = CARTESIAN_POINT ( 'NONE',  ( 0.000000000000000000, 0.000000000000000000, 20.00000000000000355 ) ) ;
#5986 = ORIENTED_EDGE ( 'NONE', *, *, #24795, .T. ) ;
#5987 = B_SPLINE_CURVE_WITH_KNOTS ( 'NONE', 5,
 ( #16472, #26086, #4525, #14123, #23731, #4837, #16779, #24492, #12214 ),
 .UNSPECIFIED., .F., .F.,
 ( 6, 3, 6 ),
 ( 0.000000000000000000, 2.405120303529999948, 3.339306057039999498 ),
 .UNSPECIFIED. ) ;
#5988 = CARTESIAN_POINT ( 'NONE',  ( -7.365079183348027136, -26.49619795852260040, 21.94317657039426805 ) ) ;
#5989 = VERTEX_POINT ( 'NONE', #22399 ) ;
#5990 = ORIENTED_EDGE ( 'NONE', *, *, #9420, .T. ) ;
#5991 = AXIS2_PLACEMENT_3D ( 'NONE', #20058, #1171, #12968 ) ;
#5992 = ORIENTED_EDGE ( 'NONE', *, *, #1511, .F. ) ;
#5993 = CARTESIAN_POINT ( 'NONE',  ( 26.58011360040000071, 9.308772197099999701, 230.5592437530000041 ) ) ;
#5994 = EDGE_CURVE ( 'NONE', #669, #12725, #29624, .T. ) ;
#5995 = DIRECTION ( 'NONE',  ( -3.868433351431744750E-13, 0.9784859933254772546, 0.2063132590645932463 ) ) ;
#5996 = DIRECTION ( 'NONE',  ( 0.9880370573969196046, -0.1542166437529877976, 0.000000000000000000 ) ) ;
#5997 = CYLINDRICAL_SURFACE ( 'NONE', #13318, 1.099999999999999201 ) ;
#5998 = CARTESIAN_POINT ( 'NONE',  ( -24.82164231762110163, 12.51999568251545369, 5.310645680000003921 ) ) ;
#5999 = CARTESIAN_POINT ( 'NONE',  ( 0.1352650258312465548, -28.50015511220833986, 3.957670871000018575 ) ) ;
#6000 = CARTESIAN_POINT ( 'NONE',  ( 4.182178350032534908, -27.18131967880234257, 209.7454400431937813 ) ) ;
#6001 = CARTESIAN_POINT ( 'NONE',  ( 23.80349752545914654, -14.36153883977784140, 4.640418250294272795 ) ) ;
#6002 = B_SPLINE_CURVE_WITH_KNOTS ( 'NONE', 5,
 ( #17944, #30080, #12933, #27707, #10577, #12782, #17641, #27254, #5691 ),
 .UNSPECIFIED., .F., .F.,
 ( 6, 3, 6 ),
 ( 0.000000000000000000, 0.6973066785939999734, 1.117931991880000142 ),
 .UNSPECIFIED. ) ;
#6003 = CARTESIAN_POINT ( 'NONE',  ( -1.392415278799817635, -4.107851135794773789, -0.5756305127000010957 ) ) ;
#6004 = CARTESIAN_POINT ( 'NONE',  ( -4.219802143827443786, -3.088637908559965339, -17.87254627010000263 ) ) ;
#6005 = CARTESIAN_POINT ( 'NONE',  ( -5.414213562369999622, -30.60492699607083722, -82.14596754238048959 ) ) ;
#6006 = EDGE_CURVE ( 'NONE', #1635, #10372, #13792, .T. ) ;
#6007 = DIRECTION ( 'NONE',  ( 0.000000000000000000, 0.3420201433259318358, -0.9396926207858125046 ) ) ;
#6008 = CARTESIAN_POINT ( 'NONE',  ( 1.827447710699809269, -4.834880234507621388, -93.88815951138720095 ) ) ;
#6009 = CARTESIAN_POINT ( 'NONE',  ( -22.55348085480000364, 18.07310466269999694, 229.2404163060000144 ) ) ;
#6010 = CARTESIAN_POINT ( 'NONE',  ( -2.235010648674410128, -0.3719431525293064866, -97.67120874165279076 ) ) ;
#6011 = CARTESIAN_POINT ( 'NONE',  ( -10.69999999930000101, -127.2537437101000108, -34.36317024006000054 ) ) ;
#6012 = EDGE_CURVE ( 'NONE', #24262, #24608, #17459, .T. ) ;
#6013 = AXIS2_PLACEMENT_3D ( 'NONE', #4887, #12114, #14492 ) ;
#6014 = CARTESIAN_POINT ( 'NONE',  ( -27.79999999970000246, -10.21376199200000201, 229.0000000000000000 ) ) ;
#6015 = CARTESIAN_POINT ( 'NONE',  ( 14.81012440339999969, 10.71727884689999932, 230.6999999999999886 ) ) ;
#6016 = CARTESIAN_POINT ( 'NONE',  ( 5.112097824811119295, -8.183944344857142283, -33.48759281112634056 ) ) ;
#6017 = ORIENTED_EDGE ( 'NONE', *, *, #25247, .F. ) ;
#6018 = CARTESIAN_POINT ( 'NONE',  ( -3.174852331340443534, -3.764700477890503549, -58.42407541852500685 ) ) ;
#6019 = LINE ( 'NONE', #15464, #19342 ) ;
#6020 = ORIENTED_EDGE ( 'NONE', *, *, #7319, .F. ) ;
#6021 = CARTESIAN_POINT ( 'NONE',  ( 4.080592064764562821, -5.083854566021194010, -3.105321867100004241 ) ) ;
#6022 = ORIENTED_EDGE ( 'NONE', *, *, #6408, .F. ) ;
#6023 = CARTESIAN_POINT ( 'NONE',  ( 20.30405755279999980, 20.00000000000000000, 226.9999998930000231 ) ) ;
#6024 = CARTESIAN_POINT ( 'NONE',  ( -3.732454924695358223, -1.410253583585163284, -68.10000000002500542 ) ) ;
#6025 = ORIENTED_EDGE ( 'NONE', *, *, #4423, .T. ) ;
#6026 = ORIENTED_EDGE ( 'NONE', *, *, #16439, .F. ) ;
#6027 = ORIENTED_EDGE ( 'NONE', *, *, #26769, .T. ) ;
#6028 = DIRECTION ( 'NONE',  ( 0.000000000000000000, 0.3420201433259318913, -0.9396926207858126157 ) ) ;
#6029 = ORIENTED_EDGE ( 'NONE', *, *, #19187, .F. ) ;
#6030 = CARTESIAN_POINT ( 'NONE',  ( -24.43008698341936835, 14.67811372381255630, 4.492876031000014869 ) ) ;
#6031 = DIRECTION ( 'NONE',  ( 0.000000000000000000, -0.3420201433259318913, 0.9396926207858126157 ) ) ;
#6032 = CARTESIAN_POINT ( 'NONE',  ( -1.219854050253892153, 4.750520449216608654, -65.80876360982500728 ) ) ;
#6033 = CARTESIAN_POINT ( 'NONE',  ( -26.80000000000000071, 3.552713678799999608E-15, 230.0000000000000000 ) ) ;
#6034 = VECTOR ( 'NONE', #10154, 1000.000000000000114 ) ;
#6035 = DIRECTION ( 'NONE',  ( 0.000000000000000000, -0.9396926207858125046, -0.3420201433259318358 ) ) ;
#6036 = CARTESIAN_POINT ( 'NONE',  ( 10.45989669369999930, 19.99999999999999645, -43.32262108698500214 ) ) ;
#6037 = CARTESIAN_POINT ( 'NONE',  ( -23.25801811775868799, -13.31593093575191666, 6.100000000003494627 ) ) ;
#6038 = CARTESIAN_POINT ( 'NONE',  ( -24.95427444319612675, 13.76797446832583560, 3.899998581000013509 ) ) ;
#6039 = ORIENTED_EDGE ( 'NONE', *, *, #19098, .F. ) ;
#6040 = CARTESIAN_POINT ( 'NONE',  ( 0.3986823046148949556, -5.109930552333694642, -8.455884211800000827 ) ) ;
#6041 = CARTESIAN_POINT ( 'NONE',  ( -26.80000000069999899, 3.281945028329999726E-15, 42.88981852279999885 ) ) ;
#6042 = PRODUCT ( 'Bolt M6', 'Bolt M6', '', ( #10996 ) ) ;
#6043 = EDGE_CURVE ( 'NONE', #14251, #28953, #22326, .T. ) ;
#6044 = FACE_OUTER_BOUND ( 'NONE', #18135, .T. ) ;
#6045 = EDGE_LOOP ( 'NONE', ( #25766, #10380, #17849, #10213 ) ) ;
#6046 = B_SPLINE_CURVE_WITH_KNOTS ( 'NONE', 5,
 ( #12948, #18282, #1143, #10737, #1002, #20652, #20336, #17957, #8058, #15459, #22557, #8362, #30250, #29934, #27725, #20183, #8680, #6015, #27889, #6333, #29775, #1618, #15930, #15613 ),
 .UNSPECIFIED., .F., .F.,
 ( 6, 3, 3, 3, 3, 3, 3, 6 ),
 ( 0.000000000000000000, 11.88805619960000115, 23.77581072610000135, 35.66412938380000242, 47.55143485110000512, 59.43964151330000334, 71.32790854499999966, 76.96280491019999204 ),
 .UNSPECIFIED. ) ;
#6047 = CARTESIAN_POINT ( 'NONE',  ( -10.69999999996683826, -29.94027628697359944, -27.70856505396162106 ) ) ;
#6048 = LINE ( 'NONE', #1340, #23357 ) ;
#6049 = CARTESIAN_POINT ( 'NONE',  ( -23.69119896560000171, -20.94188573509999785, 229.0000000000000000 ) ) ;
#6050 = CARTESIAN_POINT ( 'NONE',  ( 24.47471931349485530, 13.80892463682978999, 0.2686738749999861842 ) ) ;
#6051 = CARTESIAN_POINT ( 'NONE',  ( 8.000000000270995670, -18.23122067931581114, -34.51216076560703527 ) ) ;
#6052 = EDGE_CURVE ( 'NONE', #18608, #17864, #27606, .T. ) ;
#6053 = CARTESIAN_POINT ( 'NONE',  ( 1.728540313474559387, 5.648005006634932990, -51.46125421262499344 ) ) ;
#6054 = CARTESIAN_POINT ( 'NONE',  ( -11.37440858360000107, -24.37257237719999736, -1.450121501800003099 ) ) ;
#6056 = EDGE_CURVE ( 'NONE', #7318, #6778, #15151, .T. ) ;
#6055 = CARTESIAN_POINT ( 'NONE',  ( -14.39562240800000126, -9.581487064249998298, 5.000000000000000000 ) ) ;
#6057 = ORIENTED_EDGE ( 'NONE', *, *, #27575, .T. ) ;
#6058 = CARTESIAN_POINT ( 'NONE',  ( -9.000000000229999131, 21.70000000000000284, -45.10000000000000142 ) ) ;
#6059 = CARTESIAN_POINT ( 'NONE',  ( 27.79999999999999716, -2.355749216199999846E-11, 224.8000000000000114 ) ) ;
#6060 = B_SPLINE_CURVE_WITH_KNOTS ( 'NONE', 3,
 ( #17411, #3093, #13153, #907, #20100, #1211 ),
 .UNSPECIFIED., .F., .F.,
 ( 4, 2, 4 ),
 ( 0.000000000000000000, 0.5000000000000000000, 1.000000000000000000 ),
 .UNSPECIFIED. ) ;
#6061 = B_SPLINE_CURVE_WITH_KNOTS ( 'NONE', 3,
 ( #18556, #20604, #18400, #6290, #20925, #4395, #11328, #23453, #3932, #11482, #16044, #1883, #9261, #1579 ),
 .UNSPECIFIED., .F., .F.,
 ( 4, 2, 2, 2, 2, 2, 4 ),
 ( 0.000000000000000000, 0.2499999999999984457, 0.3749999999999976130, 0.4374999999999976130, 0.4999999999999976685, 0.7499999999999988898, 1.000000000000000000 ),
 .UNSPECIFIED. ) ;
#6062 = CARTESIAN_POINT ( 'NONE',  ( 2.530566566541730289, -4.038018835116537808, -68.10000000002500542 ) ) ;
#6063 = CARTESIAN_POINT ( 'NONE',  ( 3.254826447334524087, -1.366018022763357376, -0.6999999999999783062 ) ) ;
#6064 = CARTESIAN_POINT ( 'NONE',  ( -3.736258300216923178, -1.388188646204749910, -44.10000000002499121 ) ) ;
#6065 = AXIS2_PLACEMENT_3D ( 'NONE', #11875, #6682, #25899 ) ;
#6066 = CARTESIAN_POINT ( 'NONE',  ( 14.84842474946499280, -24.30580232298240517, -32.61831005400841121 ) ) ;
#6067 = CARTESIAN_POINT ( 'NONE',  ( -5.296314592117303377, -2.692763687817543161, -62.84424626872499431 ) ) ;
#6068 = VERTEX_POINT ( 'NONE', #22859 ) ;
#6069 = CARTESIAN_POINT ( 'NONE',  ( 20.30405755288911251, 20.00000000000103384, 229.0659093385340839 ) ) ;
#6070 = VERTEX_POINT ( 'NONE', #24752 ) ;
#6071 = CARTESIAN_POINT ( 'NONE',  ( -4.523585141650849017, -29.97671968535647835, 0.000000000000000000 ) ) ;
#6072 = ORIENTED_EDGE ( 'NONE', *, *, #12590, .F. ) ;
#6073 = LINE ( 'NONE', #27173, #13682 ) ;
#6074 = EDGE_CURVE ( 'NONE', #1905, #17033, #8360, .T. ) ;
#6075 = CARTESIAN_POINT ( 'NONE',  ( -12.29999999991583337, -26.21475634692216161, -31.32191803020494802 ) ) ;
#6076 = CARTESIAN_POINT ( 'NONE',  ( 0.000000000000000000, -50.49316738903675628, -43.39999999999999858 ) ) ;
#6077 = CARTESIAN_POINT ( 'NONE',  ( -27.16374144401319057, 6.594388859764479527, 8.000000000000007105 ) ) ;
#6078 = CARTESIAN_POINT ( 'NONE',  ( -16.50769779712623730, -10.05824544944950105, 0.000000000000000000 ) ) ;
#6079 = CARTESIAN_POINT ( 'NONE',  ( -13.99999999969999820, 20.99999999999999645, -58.51619611000000276 ) ) ;
#6080 = VERTEX_POINT ( 'NONE', #17955 ) ;
#6081 = CARTESIAN_POINT ( 'NONE',  ( 25.77914806503467560, 15.40383291000323318, 1.000000000000000888 ) ) ;
#6082 = CARTESIAN_POINT ( 'NONE',  ( -27.23548387060000309, 7.105427357599999217E-15, 141.6604601749999972 ) ) ;
#6083 = DIRECTION ( 'NONE',  ( 5.962915006522623408E-16, 0.4383711467890811231, 0.8987940462991652613 ) ) ;
#6084 = CARTESIAN_POINT ( 'NONE',  ( -3.072394438959999974, -1.678456730820000020, 230.8356432492296619 ) ) ;
#6085 = CARTESIAN_POINT ( 'NONE',  ( -8.699999999660043670, -18.28443321518998133, -36.42483785847389299 ) ) ;
#6086 = DIRECTION ( 'NONE',  ( 0.000000000000000000, 0.000000000000000000, 1.000000000000000000 ) ) ;
#6087 = LINE ( 'NONE', #30650, #23847 ) ;
#6088 = CARTESIAN_POINT ( 'NONE',  ( -17.94252184376523118, 10.97464310239704410, -1.400000000000001910 ) ) ;
#6089 = CARTESIAN_POINT ( 'NONE',  ( 4.545032752014868116, -0.3361547907463890428, -48.72442242802500090 ) ) ;
#6090 = DIRECTION ( 'NONE',  ( 0.000000000000000000, 0.000000000000000000, 1.000000000000000000 ) ) ;
#6091 = DIRECTION ( 'NONE',  ( 1.000000000000000000, -9.219545062029677348E-13, 4.710284450064082408E-12 ) ) ;
#6092 = CARTESIAN_POINT ( 'NONE',  ( 18.23252704358327847, 11.30736579158651445, -4.336808689942018722E-16 ) ) ;
#6093 = CARTESIAN_POINT ( 'NONE',  ( -10.69999999969999926, -27.00000000000000000, -28.40000000000000213 ) ) ;
#6094 = CARTESIAN_POINT ( 'NONE',  ( 10.00000000000000000, 21.35000000040000145, -64.10000000000000853 ) ) ;
#6095 = VERTEX_POINT ( 'NONE', #25060 ) ;
#6096 = CARTESIAN_POINT ( 'NONE',  ( 0.1051796283266584475, -6.084780997910130829, -33.41110030499999795 ) ) ;
#6097 = VERTEX_POINT ( 'NONE', #17805 ) ;
#6098 = EDGE_CURVE ( 'NONE', #9489, #16174, #12628, .T. ) ;
#6099 = FACE_OUTER_BOUND ( 'NONE', #15198, .T. ) ;
#6100 = CARTESIAN_POINT ( 'NONE',  ( 0.7970308137830555140, -5.845159207773487076, -50.56468436622500917 ) ) ;
#6101 = ORIENTED_EDGE ( 'NONE', *, *, #21414, .T. ) ;
#6102 = ADVANCED_FACE ( 'NONE', ( #20491 ), #15003, .F. ) ;
#6103 = SHAPE_DEFINITION_REPRESENTATION ( #27251, #8955 ) ;
#6104 = AXIS2_PLACEMENT_3D ( 'NONE', #26389, #9694, #19298 ) ;
#6105 = ORIENTED_EDGE ( 'NONE', *, *, #27878, .F. ) ;
#6106 = ORIENTED_EDGE ( 'NONE', *, *, #4704, .T. ) ;
#6107 = VECTOR ( 'NONE', #372, 1000.000000000000000 ) ;
#6108 = VECTOR ( 'NONE', #9491, 1000.000000000000114 ) ;
#6109 = DIRECTION ( 'NONE',  ( -2.965499939100700266E-25, -1.000000000000000000, 2.257145581549900232E-12 ) ) ;
#6110 = EDGE_CURVE ( 'NONE', #15341, #3911, #20093, .T. ) ;
#6111 = CARTESIAN_POINT ( 'NONE',  ( -8.699999999691694796, -25.92947359974585098, -31.20249410827203107 ) ) ;
#6112 = DIRECTION ( 'NONE',  ( -1.000000000000000000, 0.000000000000000000, 0.000000000000000000 ) ) ;
#6113 = B_SPLINE_CURVE_WITH_KNOTS ( 'NONE', 3,
 ( #6587, #20437, #10684, #6280, #3919, #20280, #3595, #25322, #8623, #15709, #25163, #3764, #18391, #1411 ),
 .UNSPECIFIED., .F., .F.,
 ( 4, 2, 2, 2, 2, 2, 4 ),
 ( 0.000000000000000000, 0.2500000000000006106, 0.3750000000000009992, 0.4375000000000012768, 0.5000000000000015543, 0.7500000000000006661, 1.000000000000000000 ),
 .UNSPECIFIED. ) ;
#6114 = CARTESIAN_POINT ( 'NONE',  ( 20.64716981389999972, -20.77933506589999979, 222.0000000000000000 ) ) ;
#6115 = FACE_OUTER_BOUND ( 'NONE', #9634, .T. ) ;
#6116 = CARTESIAN_POINT ( 'NONE',  ( -3.769085236058943966, 1.982792781023759332, -0.6999999999999992895 ) ) ;
#6117 = CARTESIAN_POINT ( 'NONE',  ( 4.080592064681261455, -5.083854565965863159, -3.105321867100004241 ) ) ;
#6118 = CARTESIAN_POINT ( 'NONE',  ( 12.41421356240000051, 25.87105682045942245, -59.46203493729375822 ) ) ;
#6119 = CARTESIAN_POINT ( 'NONE',  ( 25.07525408169050607, -13.54704387006805533, 6.073823031490324098 ) ) ;
#6120 = VERTEX_POINT ( 'NONE', #25694 ) ;
#6121 = CARTESIAN_POINT ( 'NONE',  ( 4.945711323160860928, -2.526642934800090945, -12.91474735220000269 ) ) ;
#6122 = CARTESIAN_POINT ( 'NONE',  ( 4.198532171036193361, 1.238783022255082189, -35.03159726780000938 ) ) ;
#6123 = CARTESIAN_POINT ( 'NONE',  ( 5.899424784619999862, 0.1656472027260000035, 226.6412452697800006 ) ) ;
#6124 = EDGE_CURVE ( 'NONE', #2408, #22757, #13883, .T. ) ;
#6125 = DIRECTION ( 'NONE',  ( 1.000000000000000000, -1.843431230198065424E-12, 2.650498504953516580E-12 ) ) ;
#6126 = CARTESIAN_POINT ( 'NONE',  ( -20.77600556904588913, -21.68409854326813146, 1.000000000000000888 ) ) ;
#6127 = CARTESIAN_POINT ( 'NONE',  ( 23.81569860410000317, -13.75000000000000000, 6.099999999630000502 ) ) ;
#6128 = CARTESIAN_POINT ( 'NONE',  ( -2.582034095436241738, 2.527463138869748160, 227.7116136946786753 ) ) ;
#6129 = AXIS2_PLACEMENT_3D ( 'NONE', #4364, #18038, #9077 ) ;
#6130 = CARTESIAN_POINT ( 'NONE',  ( 22.47598016381227737, 18.14223004260798078, 0.7595836940000044724 ) ) ;
#6131 = CARTESIAN_POINT ( 'NONE',  ( -11.00000000000000000, 27.10555629988041204, -61.14106941751904856 ) ) ;
#6132 = CARTESIAN_POINT ( 'NONE',  ( 0.1059454459540000032, -28.50005195860000029, 223.9040507550000143 ) ) ;
#6133 = ORIENTED_EDGE ( 'NONE', *, *, #1528, .T. ) ;
#6134 = ORIENTED_EDGE ( 'NONE', *, *, #12507, .T. ) ;
#6135 = LINE ( 'NONE', #18084, #16791 ) ;
#6136 = CARTESIAN_POINT ( 'NONE',  ( 2.788509597084857461, 2.169696472159977851, 230.8175759419343365 ) ) ;
#6137 = VERTEX_POINT ( 'NONE', #30718 ) ;
#6138 = CARTESIAN_POINT ( 'NONE',  ( 0.7993620173054750699, -3.500000000000000000, 227.6978496355018251 ) ) ;
#6139 = CARTESIAN_POINT ( 'NONE',  ( 3.072394438959999974, 1.678456730820000020, 227.6468472915199754 ) ) ;
#6140 = CARTESIAN_POINT ( 'NONE',  ( 1.353354617599272114, -4.954529841709273796, -0.7000097220332744952 ) ) ;
#6141 = VERTEX_POINT ( 'NONE', #30415 ) ;
#6142 = CARTESIAN_POINT ( 'NONE',  ( -2.639108104135487576, -27.37825522961219704, 20.00000000000000355 ) ) ;
#6143 = ORIENTED_EDGE ( 'NONE', *, *, #29397, .F. ) ;
#6144 = VERTEX_POINT ( 'NONE', #8834 ) ;
#6145 = ORIENTED_EDGE ( 'NONE', *, *, #23406, .F. ) ;
#6146 = CARTESIAN_POINT ( 'NONE',  ( -0.9902521520970002378, -27.78273347009999839, 224.4935097720000101 ) ) ;
#6147 = ORIENTED_EDGE ( 'NONE', *, *, #6885, .T. ) ;
#6148 = VECTOR ( 'NONE', #5394, 1000.000000000000000 ) ;
#6149 = CARTESIAN_POINT ( 'NONE',  ( -24.30742244210000180, -13.49161940289999961, 226.0028092389999870 ) ) ;
#6150 = CARTESIAN_POINT ( 'NONE',  ( -18.29999999989999893, -27.00000000000000000, -28.39999999989999679 ) ) ;
#6151 = EDGE_CURVE ( 'NONE', #12805, #5070, #18596, .T. ) ;
#6152 = CARTESIAN_POINT ( 'NONE',  ( 3.575086008624668299, 1.232431556331196054, -35.69999999999999574 ) ) ;
#6153 = DIRECTION ( 'NONE',  ( 0.000000000000000000, 0.000000000000000000, 1.000000000000000000 ) ) ;
#6154 = CARTESIAN_POINT ( 'NONE',  ( 2.639108104135504007, -27.37825522961219704, 210.0000000000000853 ) ) ;
#6155 = CARTESIAN_POINT ( 'NONE',  ( 2.116742336517584366, -3.333694726622333793, 227.9034567869041155 ) ) ;
#6156 = CARTESIAN_POINT ( 'NONE',  ( 27.23548387060000309, -1.776356839399999804E-15, 188.3395398250000028 ) ) ;
#6157 = ORIENTED_EDGE ( 'NONE', *, *, #10467, .F. ) ;
#6158 = CARTESIAN_POINT ( 'NONE',  ( 4.797053106898050423, -0.1656196055093784036, -3.622909721200002764 ) ) ;
#6159 = CARTESIAN_POINT ( 'NONE',  ( -1.782928038406565774, 3.983823234458339080, -22.73780126169999605 ) ) ;
#6160 = CARTESIAN_POINT ( 'NONE',  ( -4.696583076644003540, -27.09716880376585380, 209.5942911595222995 ) ) ;
#6161 = CARTESIAN_POINT ( 'NONE',  ( -17.83931601680000156, 20.00000000000000000, 230.7000111870000012 ) ) ;
#6162 = CARTESIAN_POINT ( 'NONE',  ( 3.195834452880789822, -1.520253115373796149, -90.91470530330329325 ) ) ;
#6163 = ADVANCED_FACE ( 'NONE', ( #9147 ), #6654, .T. ) ;
#6164 = CARTESIAN_POINT ( 'NONE',  ( -28.04325408099999706, 4.728524333599999352, 230.2432540810000319 ) ) ;
#6165 = CARTESIAN_POINT ( 'NONE',  ( 17.33115445853015046, 9.902812560049827795, -0.6999999999999783062 ) ) ;
#6166 = CARTESIAN_POINT ( 'NONE',  ( -24.22223838309999877, -15.01863363589999878, 225.6808321819999890 ) ) ;
#6167 = EDGE_CURVE ( 'NONE', #20581, #11717, #12720, .T. ) ;
#6168 = CARTESIAN_POINT ( 'NONE',  ( 22.97559295455008765, 15.65128684778802715, 8.000000000000007105 ) ) ;
#6169 = EDGE_CURVE ( 'NONE', #9481, #2437, #12617, .T. ) ;
#6170 = CARTESIAN_POINT ( 'NONE',  ( -11.38367146589999912, -24.46198237100000128, 230.6999999999999886 ) ) ;
#6171 = CARTESIAN_POINT ( 'NONE',  ( 2.247213954888706677, -3.736744008551091678, -38.99444316444944292 ) ) ;
#6172 = ORIENTED_EDGE ( 'NONE', *, *, #2101, .F. ) ;
#6173 = CARTESIAN_POINT ( 'NONE',  ( -1.989652436383612555, 4.808159600214577445, -56.34652090042499850 ) ) ;
#6174 = CIRCLE ( 'NONE', #6692, 3.199999983039998774 ) ;
#6175 = CARTESIAN_POINT ( 'NONE',  ( 0.000000000000000000, 4.811145170119999648, -67.12721591429999535 ) ) ;
#6176 = EDGE_LOOP ( 'NONE', ( #21367, #1483, #5030, #2983 ) ) ;
#6177 = EDGE_CURVE ( 'NONE', #2338, #27018, #1776, .T. ) ;
#6178 = CARTESIAN_POINT ( 'NONE',  ( -3.510061880997908279, 5.032561185093348044, -1.627651354100000169 ) ) ;
#6179 = VERTEX_POINT ( 'NONE', #15926 ) ;
#6180 = CARTESIAN_POINT ( 'NONE',  ( 7.638687372243862406, -6.912605514289321462, -37.44547201132905911 ) ) ;
#6181 = CARTESIAN_POINT ( 'NONE',  ( 23.25788685383077592, -13.43083806724684948, 186.7828584119999391 ) ) ;
#6182 = EDGE_LOOP ( 'NONE', ( #18605, #369, #6813, #14908, #20275 ) ) ;
#6183 = CARTESIAN_POINT ( 'NONE',  ( 10.73600574249999973, 19.99999999999999645, -2.108020795500001210 ) ) ;
#6184 = ORIENTED_EDGE ( 'NONE', *, *, #10047, .T. ) ;
#6185 = ORIENTED_EDGE ( 'NONE', *, *, #27154, .T. ) ;
#6186 = CARTESIAN_POINT ( 'NONE',  ( 5.114250173089999407, 17.43050732989999929, 231.6999999999999886 ) ) ;
#6187 = ORIENTED_EDGE ( 'NONE', *, *, #30828, .T. ) ;
#6188 = CARTESIAN_POINT ( 'NONE',  ( 24.39135169777336287, -14.74223403354865347, 5.310643619999999565 ) ) ;
#6189 = EDGE_CURVE ( 'NONE', #12912, #13582, #23794, .T. ) ;
#6190 = FACE_OUTER_BOUND ( 'NONE', #19033, .T. ) ;
#6191 = VECTOR ( 'NONE', #8041, 1000.000000000000000 ) ;
#6192 = CARTESIAN_POINT ( 'NONE',  ( -2.911316102860724175, -3.927725552502973727, -65.13409070562501313 ) ) ;
#6193 = VECTOR ( 'NONE', #27523, 1000.000000000000000 ) ;
#6194 = CARTESIAN_POINT ( 'NONE',  ( -13.32567267019999946, -26.75623947960000137, 230.0000000000000000 ) ) ;
#6195 = CARTESIAN_POINT ( 'NONE',  ( -19.80526803560000104, 19.50877411510000314, 227.0000000000000000 ) ) ;
#6196 = CARTESIAN_POINT ( 'NONE',  ( 10.20952265640000078, 19.99999999999999645, -43.61772437372000155 ) ) ;
#6197 = VECTOR ( 'NONE', #24314, 1000.000000000000000 ) ;
#6198 = CARTESIAN_POINT ( 'NONE',  ( -17.49199711315135986, -24.60220466956999985, -24.01086508779000184 ) ) ;
#6199 = EDGE_CURVE ( 'NONE', #18476, #3989, #19373, .T. ) ;
#6200 = CARTESIAN_POINT ( 'NONE',  ( -25.45799949038170240, 12.81261085762170815, 4.791562840999991302 ) ) ;
#6201 = CARTESIAN_POINT ( 'NONE',  ( 5.067327387632984959, 4.072231104569050686, -7.754586408000002429 ) ) ;
#6202 = CARTESIAN_POINT ( 'NONE',  ( 25.94128158184369681, -6.955966684932006316, 0.000000000000000000 ) ) ;
#6203 = CARTESIAN_POINT ( 'NONE',  ( 19.06862361850000198, 19.69237242210000005, 229.7996270940000159 ) ) ;
#6204 = ORIENTED_EDGE ( 'NONE', *, *, #3704, .F. ) ;
#6205 = CARTESIAN_POINT ( 'NONE',  ( 24.50046877880000196, -13.13673243530000079, 224.3193205009999929 ) ) ;
#6206 = CARTESIAN_POINT ( 'NONE',  ( -22.70032920229352769, -14.24644155152564373, 4.508626839105193795 ) ) ;
#6207 = CARTESIAN_POINT ( 'NONE',  ( -23.80092421055088892, -14.36517094966330710, 6.099998581000020792 ) ) ;
#6208 = CARTESIAN_POINT ( 'NONE',  ( 24.69145217640891232, 13.93120638769218367, 0.7069220679999932422 ) ) ;
#6209 = PLANE ( 'NONE',  #17535 ) ;
#6210 = CARTESIAN_POINT ( 'NONE',  ( 5.782578939028539367, 2.564649547393091478, -51.87998794302499306 ) ) ;
#6211 = DIRECTION ( 'NONE',  ( 0.000000000000000000, 0.3420201433259318913, -0.9396926207858126157 ) ) ;
#6212 = CARTESIAN_POINT ( 'NONE',  ( 27.69999999930000101, -3.392159599989999961E-15, 140.0000000000000000 ) ) ;
#6213 = ORIENTED_EDGE ( 'NONE', *, *, #4502, .F. ) ;
#6214 = CARTESIAN_POINT ( 'NONE',  ( 24.49145441566124148, -14.57548795709913847, 4.319167818000013703 ) ) ;
#6215 = FACE_OUTER_BOUND ( 'NONE', #26942, .T. ) ;
#6216 = VECTOR ( 'NONE', #9116, 1000.000000000000114 ) ;
#6217 = VECTOR ( 'NONE', #2, 1000.000000000000227 ) ;
#6218 = CIRCLE ( 'NONE', #17262, 27.23548387100000312 ) ;
#6219 = CARTESIAN_POINT ( 'NONE',  ( 2.876589613553454772, -3.520147964197292811, -68.10000000002500542 ) ) ;
#6220 = DIRECTION ( 'NONE',  ( 0.000000000000000000, 0.000000000000000000, -1.000000000000000000 ) ) ;
#6221 = CARTESIAN_POINT ( 'NONE',  ( -24.33346004068009449, -12.81155130651987406, 225.2867514112106733 ) ) ;
#6222 = DIRECTION ( 'NONE',  ( -1.000000000000000000, 0.000000000000000000, 0.000000000000000000 ) ) ;
#6223 = CARTESIAN_POINT ( 'NONE',  ( -8.915308721984681384, -8.516764330229598556, 232.6627637660201628 ) ) ;
#6224 = ADVANCED_FACE ( 'NONE', ( #13055 ), #29738, .T. ) ;
#6225 = CARTESIAN_POINT ( 'NONE',  ( -5.505147662666007413, -0.2930537997861774602, -66.36421022022500438 ) ) ;
#6226 = ORIENTED_EDGE ( 'NONE', *, *, #30860, .T. ) ;
#6227 = CARTESIAN_POINT ( 'NONE',  ( 18.28303642507142968, 20.00000852599190537, 230.6738034682653904 ) ) ;
#6228 = EDGE_CURVE ( 'NONE', #5171, #5374, #14245, .T. ) ;
#6229 = ORIENTED_EDGE ( 'NONE', *, *, #17891, .F. ) ;
#6230 = EDGE_CURVE ( 'NONE', #13263, #20656, #685, .T. ) ;
#6231 = CARTESIAN_POINT ( 'NONE',  ( -19.29867024690000221, 19.63492390480000083, 229.6953880050000123 ) ) ;
#6232 = EDGE_CURVE ( 'NONE', #19159, #2499, #31018, .T. ) ;
#6233 = ORIENTED_EDGE ( 'NONE', *, *, #12323, .F. ) ;
#6235 = CARTESIAN_POINT ( 'NONE',  ( 24.66410523950000311, -14.28055064019999953, 226.1000014189999945 ) ) ;
#6234 = AXIS2_PLACEMENT_3D ( 'NONE', #22906, #1346, #10940 ) ;
#6236 = FACE_OUTER_BOUND ( 'NONE', #13002, .T. ) ;
#6237 = AXIS2_PLACEMENT_3D ( 'NONE', #25466, #16012, #28277 ) ;
#6238 = CARTESIAN_POINT ( 'NONE',  ( 25.46368747440213198, -12.80129684534102807, 4.895780544000027490 ) ) ;
#6239 = FACE_OUTER_BOUND ( 'NONE', #11323, .T. ) ;
#6240 = UNCERTAINTY_MEASURE_WITH_UNIT (LENGTH_MEASURE( 1.000000000000000082E-05 ), #17142, 'distance_accuracy_value', 'NONE');
#6241 = CIRCLE ( 'NONE', #16793, 3.000000000000001332 ) ;
#6242 = B_SPLINE_CURVE_WITH_KNOTS ( 'NONE', 3,
 ( #24673, #7977, #15379, #22626, #24977, #3413, #13015, #1067, #10657, #20248, #23251, #15529, #16006, #6405 ),
 .UNSPECIFIED., .F., .F.,
 ( 4, 2, 2, 2, 2, 2, 4 ),
 ( 0.000000000000000000, 0.2500000000000003331, 0.3750000000000004996, 0.4375000000000000000, 0.4999999999999995559, 0.7499999999999997780, 1.000000000000000000 ),
 .UNSPECIFIED. ) ;
#6243 = CARTESIAN_POINT ( 'NONE',  ( -28.49528339128749366, -0.5184828350247780993, 8.000000000000007105 ) ) ;
#6244 = B_SPLINE_CURVE_WITH_KNOTS ( 'NONE', 1,
 ( #18878, #11491 ),
 .UNSPECIFIED., .F., .F.,
 ( 2, 2 ),
 ( -2.557520719980000135E-06, 0.7000000000009999335 ),
 .UNSPECIFIED. ) ;
#6245 = LINE ( 'NONE', #11284, #29513 ) ;
#6246 = CARTESIAN_POINT ( 'NONE',  ( 10.00000000000000000, 20.99999999999999645, -64.10000000019999788 ) ) ;
#6247 = ORIENTED_EDGE ( 'NONE', *, *, #10579, .F. ) ;
#6248 = CARTESIAN_POINT ( 'NONE',  ( -24.06826084733133797, 20.50742046740553093, 8.000000000000007105 ) ) ;
#6249 = CARTESIAN_POINT ( 'NONE',  ( 24.71241344867332046, 12.80597785358207297, 8.000000000000007105 ) ) ;
#6250 = CARTESIAN_POINT ( 'NONE',  ( 1.346291201779999946, -4.118494162357343669, -70.37733883405731206 ) ) ;
#6251 = CARTESIAN_POINT ( 'NONE',  ( -2.020725942269999909, -3.500000000000000000, 230.5235986622430175 ) ) ;
#6252 = CARTESIAN_POINT ( 'NONE',  ( -24.09883371379999772, -15.21565466309999870, 225.1042187089999800 ) ) ;
#6253 = CARTESIAN_POINT ( 'NONE',  ( 0.000000000000000000, 0.000000000000000000, 227.6412452700500069 ) ) ;
#6254 = CARTESIAN_POINT ( 'NONE',  ( -25.46368746804859740, 12.80129684245613575, 4.895780543000022078 ) ) ;
#6255 = CARTESIAN_POINT ( 'NONE',  ( -26.79556473285982321, -0.4875557887250224209, 0.000000000000000000 ) ) ;
#6256 = CARTESIAN_POINT ( 'NONE',  ( 4.894650655971835462, -0.3620128515310818140, -48.37442242802500658 ) ) ;
#6257 = CARTESIAN_POINT ( 'NONE',  ( -10.00000000020000002, -25.00000000000000000, -2.357243106799994159 ) ) ;
#6258 = CARTESIAN_POINT ( 'NONE',  ( 27.79539923781684507, 0.5057481689249130330, 1.000000000000000888 ) ) ;
#6259 = CARTESIAN_POINT ( 'NONE',  ( -20.30396346370000060, 20.00000000000000000, 229.0000000000000000 ) ) ;
#6260 = LINE ( 'NONE', #20902, #8769 ) ;
#6261 = AXIS2_PLACEMENT_3D ( 'NONE', #14325, #2512, #12250 ) ;
#6262 = VECTOR ( 'NONE', #17732, 1000.000000000000114 ) ;
#6263 = AXIS2_PLACEMENT_3D ( 'NONE', #20529, #5584, #12832 ) ;
#6264 = CARTESIAN_POINT ( 'NONE',  ( -24.13062658854171971, -13.18986347145018634, 224.0869147258247835 ) ) ;
#6265 = ORIENTED_EDGE ( 'NONE', *, *, #2619, .F. ) ;
#6266 = CARTESIAN_POINT ( 'NONE',  ( 3.155489075140828437, 3.034105443485042741, -35.32341724620001600 ) ) ;
#6267 = VERTEX_POINT ( 'NONE', #22516 ) ;
#6268 = CARTESIAN_POINT ( 'NONE',  ( -4.213298386693987041, 4.800796338109710071, -54.46587006832499611 ) ) ;
#6269 = VERTEX_POINT ( 'NONE', #24566 ) ;
#6270 = CONTEXT_DEPENDENT_SHAPE_REPRESENTATION ( #27662, #8138 ) ;
#6271 = EDGE_LOOP ( 'NONE', ( #9137, #25470, #19827, #22708 ) ) ;
#6272 = ADVANCED_FACE ( 'NONE', ( #27225 ), #5667, .F. ) ;
#6273 = ORIENTED_EDGE ( 'NONE', *, *, #12374, .T. ) ;
#6274 = AXIS2_PLACEMENT_3D ( 'NONE', #16492, #4232, #27987 ) ;
#6275 = STYLED_ITEM ( 'NONE', ( #14374 ), #21175 ) ;
#6276 = SURFACE_SIDE_STYLE ('',( #13508 ) ) ;
#6277 = CARTESIAN_POINT ( 'NONE',  ( 3.510330247560000227, 1.917702154400000136, -43.40000000037299799 ) ) ;
#6278 = FACE_OUTER_BOUND ( 'NONE', #9523, .T. ) ;
#6279 = CARTESIAN_POINT ( 'NONE',  ( 8.000000000839076364, -16.52148444845764885, -38.01532054216111334 ) ) ;
#6280 = CARTESIAN_POINT ( 'NONE',  ( -1.019043872447617405, -27.48159911132789901, 4.579737331571473113 ) ) ;
#6281 = CARTESIAN_POINT ( 'NONE',  ( -1.419173393149999842E-06, -27.80022181310000207, 226.1000014189999945 ) ) ;
#6282 = CARTESIAN_POINT ( 'NONE',  ( -3.673964118181757943, -4.849481262180703744, -3.128945369300001111 ) ) ;
#6283 = CARTESIAN_POINT ( 'NONE',  ( 1.746192186286341652, -1.009653006786209506, 230.8412452700000301 ) ) ;
#6284 = CARTESIAN_POINT ( 'NONE',  ( 2.070461221339999991, 7.056594471000000368, 228.3912452697800006 ) ) ;
#6285 = CIRCLE ( 'NONE', #8724, 26.80000000000000071 ) ;
#6286 = CARTESIAN_POINT ( 'NONE',  ( -2.345194346458623347, -4.011532291445385923, -16.18182079289999820 ) ) ;
#6287 = CARTESIAN_POINT ( 'NONE',  ( -3.910239773549598397, 2.823051725158805425, -33.52946136360000651 ) ) ;
#6288 = DIRECTION ( 'NONE',  ( -1.000000000000000000, 0.000000000000000000, -2.257144471330000330E-12 ) ) ;
#6289 = EDGE_CURVE ( 'NONE', #10995, #6418, #23900, .T. ) ;
#6290 = CARTESIAN_POINT ( 'NONE',  ( -1.018916986544576408, -26.78112380547544547, 5.420582067115832459 ) ) ;
#6291 = CARTESIAN_POINT ( 'NONE',  ( 0.1033071333860000052, -27.80005613160000166, 223.9040507550000143 ) ) ;
#6292 = CARTESIAN_POINT ( 'NONE',  ( -27.22236205671638842, -6.258747753008545800, 8.000000000000007105 ) ) ;
#6293 = CARTESIAN_POINT ( 'NONE',  ( -28.50000000000000000, 1.776356839399999922E-14, 222.0000000000000000 ) ) ;
#6294 = CARTESIAN_POINT ( 'NONE',  ( 25.29825173858419873, 14.27357626363527920, 0.5017677510000262409 ) ) ;
#6295 = B_SPLINE_CURVE_WITH_KNOTS ( 'NONE', 3,
 ( #13469, #20555, #14950, #24547, #24856, #6393 ),
 .UNSPECIFIED., .F., .F.,
 ( 4, 2, 4 ),
 ( 0.000000000000000000, 0.5000000000000000000, 1.000000000000000000 ),
 .UNSPECIFIED. ) ;
#6296 = CARTESIAN_POINT ( 'NONE',  ( -8.699999999662320960, -13.45909514929641304, -35.92961830801370127 ) ) ;
#6297 = CARTESIAN_POINT ( 'NONE',  ( -9.892226903239841107, 20.00000000000001066, -42.92198665947150715 ) ) ;
#6298 = AXIS2_PLACEMENT_3D ( 'NONE', #29767, #10583, #19724 ) ;
#6299 = ORIENTED_EDGE ( 'NONE', *, *, #3172, .F. ) ;
#6300 = MECHANICAL_DESIGN_GEOMETRIC_PRESENTATION_REPRESENTATION (  '', ( #23411 ), #24903 ) ;
#6301 = EDGE_CURVE ( 'NONE', #5952, #19818, #27798, .T. ) ;
#6302 = CARTESIAN_POINT ( 'NONE',  ( -1.346291201779999946, -4.118494162357343669, -70.37733883405731206 ) ) ;
#6303 = ORIENTED_EDGE ( 'NONE', *, *, #15465, .T. ) ;
#6304 = CARTESIAN_POINT ( 'NONE',  ( 2.020725942159999899, -3.500000000000000000, 227.9588918784999976 ) ) ;
#6305 = CARTESIAN_POINT ( 'NONE',  ( -25.17394274020000111, -13.36230406159999973, 224.4928762930000232 ) ) ;
#6306 = CARTESIAN_POINT ( 'NONE',  ( -18.95046173579999760, -18.95046173579999760, 115.0000000000000000 ) ) ;
#6307 = ORIENTED_EDGE ( 'NONE', *, *, #19701, .F. ) ;
#6308 = CARTESIAN_POINT ( 'NONE',  ( -6.756062549273579521, -26.65810324902504291, 21.45434275270897118 ) ) ;
#6309 = VERTEX_POINT ( 'NONE', #25963 ) ;
#6310 = EDGE_LOOP ( 'NONE', ( #22793, #6814, #18130, #25347 ) ) ;
#6311 = APPLICATION_PROTOCOL_DEFINITION ( 'draft international standard', 'automotive_design', 1998, #23649 ) ;
#6312 = ORIENTED_EDGE ( 'NONE', *, *, #17697, .T. ) ;
#6313 = CARTESIAN_POINT ( 'NONE',  ( 21.39276574850000046, 17.15274395180000155, 230.6999999999999886 ) ) ;
#6314 = ORIENTED_EDGE ( 'NONE', *, *, #6228, .F. ) ;
#6315 = CARTESIAN_POINT ( 'NONE',  ( -19.80526744909999692, 19.50877353739999975, 229.0000000010000178 ) ) ;
#6316 = CARTESIAN_POINT ( 'NONE',  ( -24.07583586439999834, -13.90018868249999962, 226.1000014189999945 ) ) ;
#6317 = CARTESIAN_POINT ( 'NONE',  ( 1.182563860066578654, 3.920765007589456452, -35.70000000000000284 ) ) ;
#6318 = CARTESIAN_POINT ( 'NONE',  ( 0.03635086285233400660, -28.50041301604787947, 3.997479608999987555 ) ) ;
#6319 = CARTESIAN_POINT ( 'NONE',  ( -26.93395402219999824, 3.298349122909999612E-15, 137.7567592739999895 ) ) ;
#6320 = CARTESIAN_POINT ( 'NONE',  ( 23.63627835225026530, -12.63201688062175698, 5.666076084815439451 ) ) ;
#6321 = EDGE_CURVE ( 'NONE', #24088, #11396, #14004, .T. ) ;
#6322 = CARTESIAN_POINT ( 'NONE',  ( 27.06563796010000189, -3.314475221599999482E-15, 188.0597313979999967 ) ) ;
#6323 = ORIENTED_EDGE ( 'NONE', *, *, #10187, .F. ) ;
#6324 = CARTESIAN_POINT ( 'NONE',  ( 1.699015317690025118, 6.330513620609809600, -2.053410702900000828 ) ) ;
#6325 = CARTESIAN_POINT ( 'NONE',  ( -0.6320852424383932577, 6.069672320066970883, -25.88903409330001182 ) ) ;
#6326 = CARTESIAN_POINT ( 'NONE',  ( -3.163284386374744628, -27.32243547426060815, 209.9517032567745503 ) ) ;
#6327 = LINE ( 'NONE', #20645, #14528 ) ;
#6328 = CARTESIAN_POINT ( 'NONE',  ( 25.17364887440000132, -13.36205984489999921, 224.4930265309999982 ) ) ;
#6329 = CARTESIAN_POINT ( 'NONE',  ( -7.260640027187754697, -115.1289678868684803, 21.93662520831884066 ) ) ;
#6330 = FACE_OUTER_BOUND ( 'NONE', #1432, .T. ) ;
#6331 = DIRECTION ( 'NONE',  ( -0.9316362575375349842, 0.3633921898465292122, -0.000000000000000000 ) ) ;
#6332 = FACE_BOUND ( 'NONE', #17815, .T. ) ;
#6333 = CARTESIAN_POINT ( 'NONE',  ( 12.00334263380000088, 13.78333882559999957, 230.6999999999999886 ) ) ;
#6334 = CARTESIAN_POINT ( 'NONE',  ( -17.93324555120827668, 10.97998838178171432, -0.6999999999999784173 ) ) ;
#6335 = ORIENTED_EDGE ( 'NONE', *, *, #23334, .F. ) ;
#6336 = CARTESIAN_POINT ( 'NONE',  ( 4.317698767220935707, -2.252650425851481675, -60.56790713612500809 ) ) ;
#6337 = CARTESIAN_POINT ( 'NONE',  ( 2.664535259099999805E-15, 2.694277338339796213, -67.89769279494430521 ) ) ;
#6338 = ORIENTED_EDGE ( 'NONE', *, *, #19187, .T. ) ;
#6339 = EDGE_CURVE ( 'NONE', #18717, #19721, #16047, .T. ) ;
#6340 = CARTESIAN_POINT ( 'NONE',  ( 0.7420639427752478978, -6.011517603930927045, -18.37054674910000429 ) ) ;
#6341 = ORIENTED_EDGE ( 'NONE', *, *, #2339, .F. ) ;
#6342 = CARTESIAN_POINT ( 'NONE',  ( -3.262900226955093519, -2.198300220329731935, -68.10000000002501963 ) ) ;
#6343 = ORIENTED_EDGE ( 'NONE', *, *, #8047, .F. ) ;
#6344 = FILL_AREA_STYLE ('',( #28777 ) ) ;
#6345 = ORIENTED_EDGE ( 'NONE', *, *, #16479, .F. ) ;
#6346 = ORIENTED_EDGE ( 'NONE', *, *, #22972, .F. ) ;
#6347 = CARTESIAN_POINT ( 'NONE',  ( 24.28117756997326637, -12.91036561242075997, 4.443835645643864574 ) ) ;
#6348 = FILL_AREA_STYLE_COLOUR ( '', #6768 ) ;
#6349 = VERTEX_POINT ( 'NONE', #23140 ) ;
#6350 = CARTESIAN_POINT ( 'NONE',  ( -13.12132034329999897, 20.99999999990000887, -69.22132034359999864 ) ) ;
#6351 = CARTESIAN_POINT ( 'NONE',  ( -8.699999999628824199, -19.62590121859827619, -40.87657246514151410 ) ) ;
#6352 = EDGE_CURVE ( 'NONE', #53, #15258, #5481, .T. ) ;
#6353 = CARTESIAN_POINT ( 'NONE',  ( -5.434147616959247529, -3.211087428728324866, -67.84382590962499648 ) ) ;
#6354 = DIRECTION ( 'NONE',  ( 1.000000000000000000, 0.000000000000000000, 0.000000000000000000 ) ) ;
#6355 = EDGE_CURVE ( 'NONE', #9043, #29282, #11122, .T. ) ;
#6356 = APPLICATION_CONTEXT ( 'automotive_design' ) ;
#6357 = DIRECTION ( 'NONE',  ( 0.000000000000000000, -1.000000000000000000, 0.000000000000000000 ) ) ;
#6358 = CARTESIAN_POINT ( 'NONE',  ( -11.69999999989999928, 19.99999999999999645, -1.399999999999998579 ) ) ;
#6359 = CARTESIAN_POINT ( 'NONE',  ( 8.699999999974050269, -116.8589940799748632, 11.34037320843244956 ) ) ;
#6360 = ORIENTED_EDGE ( 'NONE', *, *, #16373, .T. ) ;
#6361 = LINE ( 'NONE', #17834, #26071 ) ;
#6362 = EDGE_CURVE ( 'NONE', #23901, #29453, #8801, .T. ) ;
#6363 = CARTESIAN_POINT ( 'NONE',  ( -4.799781135534763266, 0.1424267153701331001, -12.24554957890000040 ) ) ;
#6364 = DIRECTION ( 'NONE',  ( 0.000000000000000000, 0.9396926207858125046, 0.3420201433259318358 ) ) ;
#6365 = CARTESIAN_POINT ( 'NONE',  ( 8.999999999770000869, 20.99999999999999645, -58.10000000000000142 ) ) ;
#6366 = ORIENTED_EDGE ( 'NONE', *, *, #24765, .F. ) ;
#6367 = CARTESIAN_POINT ( 'NONE',  ( -10.69999999996466755, -29.52945879161127252, -26.74930136228349298 ) ) ;
#6368 = DIRECTION ( 'NONE',  ( 0.000000000000000000, -1.000000000000000000, 2.257145581549999994E-12 ) ) ;
#6369 = CARTESIAN_POINT ( 'NONE',  ( -8.999999999710000864, 20.70710678120000381, -44.39289321881399530 ) ) ;
#6370 = CARTESIAN_POINT ( 'NONE',  ( 15.49562240950000103, -7.676231176589999983, 225.0000000000000000 ) ) ;
#6371 = CARTESIAN_POINT ( 'NONE',  ( 10.99289321870000080, -24.65831413369999936, -1.692893218799999877 ) ) ;
#6372 = CARTESIAN_POINT ( 'NONE',  ( -3.297371880451163584, -3.946021304934626883, -44.16141975532499941 ) ) ;
#6373 = EDGE_CURVE ( 'NONE', #14204, #24890, #8637, .T. ) ;
#6374 = CARTESIAN_POINT ( 'NONE',  ( -11.69999999989999928, -24.11120071670000087, -0.6999999999999992895 ) ) ;
#6375 = DIRECTION ( 'NONE',  ( 1.000000000000000000, 0.000000000000000000, 0.000000000000000000 ) ) ;
#6376 = EDGE_LOOP ( 'NONE', ( #30642, #24221, #20913, #22140, #27423, #205, #27783 ) ) ;
#6377 = CYLINDRICAL_SURFACE ( 'NONE', #3221, 2.000000000000000000 ) ;
#6378 = DIRECTION ( 'NONE',  ( 0.9316362575375356503, 0.3633921898465274913, 0.000000000000000000 ) ) ;
#6379 = CARTESIAN_POINT ( 'NONE',  ( 2.613153378155294693, -3.469718638663583654, -68.10000000002500542 ) ) ;
#6380 = ADVANCED_FACE ( 'NONE', ( #27842 ), #11435, .F. ) ;
#6381 = CIRCLE ( 'NONE', #31004, 3.200000004570001888 ) ;
#6382 = DIRECTION ( 'NONE',  ( 0.000000000000000000, 0.000000000000000000, -1.000000000000000000 ) ) ;
#6383 = CARTESIAN_POINT ( 'NONE',  ( -4.308414154086193548, 1.093458695205176801, -44.10000000002497700 ) ) ;
#6384 = CARTESIAN_POINT ( 'NONE',  ( -14.00000000000000000, 20.99999999999999645, -62.80809805499999499 ) ) ;
#6385 = CARTESIAN_POINT ( 'NONE',  ( 0.2854594907656595737, 4.304903296723256112, -39.57881079955906500 ) ) ;
#6386 = COLOUR_RGB ( '', 0.66274510, 0.83137255, 0.94901961) ;
#6387 = CARTESIAN_POINT ( 'NONE',  ( 1.304267357873228894, -5.326741986703369847, -65.50397119102498777 ) ) ;
#6388 = ORIENTED_EDGE ( 'NONE', *, *, #13396, .F. ) ;
#6389 = LINE ( 'NONE', #13782, #2373 ) ;
#6390 = ORIENTED_EDGE ( 'NONE', *, *, #9589, .F. ) ;
#6391 = CARTESIAN_POINT ( 'NONE',  ( -3.224145675551910895, -2.281186089468392186, -44.28462724592499455 ) ) ;
#6392 = VERTEX_POINT ( 'NONE', #19496 ) ;
#6393 = CARTESIAN_POINT ( 'NONE',  ( -13.12132034329999897, 20.99999999990000887, -69.22132034359999864 ) ) ;
#6394 = CARTESIAN_POINT ( 'NONE',  ( 27.50000000000000000, -6.735334946019999940E-15, 36.39444872359999295 ) ) ;
#6395 = CARTESIAN_POINT ( 'NONE',  ( -3.858789587622685868, -0.3163803785149745251, 230.6290587881455849 ) ) ;
#6396 = CARTESIAN_POINT ( 'NONE',  ( -0.3775595308767857317, -28.49777658967402871, 4.319846982000025370 ) ) ;
#6397 = DIRECTION ( 'NONE',  ( 0.8660254037843290176, 0.5000000000001899592, 0.000000000000000000 ) ) ;
#6398 = FACE_OUTER_BOUND ( 'NONE', #4184, .T. ) ;
#6399 = ORIENTED_EDGE ( 'NONE', *, *, #12685, .F. ) ;
#6400 = DIRECTION ( 'NONE',  ( 0.000000000000000000, 0.3420201433259318913, -0.9396926207858126157 ) ) ;
#6401 = CARTESIAN_POINT ( 'NONE',  ( 23.60106408278174328, 14.73312039574607901, 8.000000000000007105 ) ) ;
#6402 = CARTESIAN_POINT ( 'NONE',  ( 17.99586598600000187, 19.96083381589999917, 229.9999934530000019 ) ) ;
#6403 = MECHANICAL_DESIGN_GEOMETRIC_PRESENTATION_REPRESENTATION (  '', ( #25502 ), #3383 ) ;
#6404 = CARTESIAN_POINT ( 'NONE',  ( 2.746585479520242742E-10, -5.287238790993575854, -26.38853270457268607 ) ) ;
#6405 = CARTESIAN_POINT ( 'NONE',  ( 23.20948082139999968, -13.40000000000000036, 3.900000000369999942 ) ) ;
#6406 = DIRECTION ( 'NONE',  ( -1.000000000000000000, 2.463770379189999939E-24, 2.257150022439999944E-12 ) ) ;
#6407 = AXIS2_PLACEMENT_3D ( 'NONE', #541, #28421, #26219 ) ;
#6408 = EDGE_CURVE ( 'NONE', #16559, #16947, #5017, .T. ) ;
#6409 = DIRECTION ( 'NONE',  ( 0.000000000000000000, 0.000000000000000000, -1.000000000000000000 ) ) ;
#6410 = DIRECTION ( 'NONE',  ( 0.000000000000000000, 0.000000000000000000, -1.000000000000000000 ) ) ;
#6411 = CARTESIAN_POINT ( 'NONE',  ( 5.943504367937093136, -0.4395870339238064362, -49.12442242802499948 ) ) ;
#6412 = ADVANCED_FACE ( 'NONE', ( #6905 ), #24590, .T. ) ;
#6413 = EDGE_CURVE ( 'NONE', #68, #24422, #1489, .T. ) ;
#6414 = CARTESIAN_POINT ( 'NONE',  ( -20.30396346370000060, 20.00000000000000000, 227.8000000000000114 ) ) ;
#6415 = CARTESIAN_POINT ( 'NONE',  ( 14.40197535836999876, -26.99999999999984368, -34.17350269180000311 ) ) ;
#6416 = DIRECTION ( 'NONE',  ( 0.000000000000000000, -1.000000000000000000, 0.000000000000000000 ) ) ;
#6417 = CARTESIAN_POINT ( 'NONE',  ( -0.4908581392059040982, -27.49541710664062677, 224.0051167709335402 ) ) ;
#6418 = VERTEX_POINT ( 'NONE', #2266 ) ;
#6419 = CARTESIAN_POINT ( 'NONE',  ( 10.69999999997431672, -25.48863729555974444, -31.02111648952697820 ) ) ;
#6420 = EDGE_LOOP ( 'NONE', ( #24916, #18299, #5948 ) ) ;
#6421 = CARTESIAN_POINT ( 'NONE',  ( -1.293561172433232986, -6.216321778783836294, -52.92706695232499925 ) ) ;
#6422 = EDGE_LOOP ( 'NONE', ( #22173, #27738 ) ) ;
#6423 = VECTOR ( 'NONE', #12768, 1000.000000000000114 ) ;
#6424 = APPLICATION_PROTOCOL_DEFINITION ( 'draft international standard', 'automotive_design', 1998, #8545 ) ;
#6425 = ORIENTED_EDGE ( 'NONE', *, *, #29890, .T. ) ;
#6426 = AXIS2_PLACEMENT_3D ( 'NONE', #9446, #19049, #28648 ) ;
#6427 = B_SPLINE_CURVE_WITH_KNOTS ( 'NONE', 3,
 ( #26684, #9853, #7792, #21975, #7490, #19765, #12669, #2469, #12207, #21665 ),
 .UNSPECIFIED., .F., .F.,
 ( 4, 2, 2, 2, 4 ),
 ( 0.000000000000000000, 0.2500000000000000000, 0.5000000000000000000, 0.7500000000000000000, 1.000000000000000000 ),
 .UNSPECIFIED. ) ;
#6428 = ORIENTED_EDGE ( 'NONE', *, *, #23291, .T. ) ;
#6429 = DIRECTION ( 'NONE',  ( 1.000000000000000000, 0.000000000000000000, 0.000000000000000000 ) ) ;
#6430 = CARTESIAN_POINT ( 'NONE',  ( -17.39611244578981797, -30.63332389908853770, -24.72419783949291627 ) ) ;
#6431 = CARTESIAN_POINT ( 'NONE',  ( -5.509622826249999328, -10.91334849979999966, 232.6627648150000027 ) ) ;
#6432 = CARTESIAN_POINT ( 'NONE',  ( 8.000000000660609345, -13.38331437764704113, -35.60411298974170080 ) ) ;
#6433 = CARTESIAN_POINT ( 'NONE',  ( -16.17354070529352583, 11.89178602531050899, -4.336808689942018722E-16 ) ) ;
#6434 = CARTESIAN_POINT ( 'NONE',  ( -5.440024667461782037, 2.837840394948672351, -0.8187643563000029934 ) ) ;
#6435 = CARTESIAN_POINT ( 'NONE',  ( 2.000067258429029771, -0.2648802556752501425, 230.8412452700000301 ) ) ;
#6436 = CARTESIAN_POINT ( 'NONE',  ( 25.45015930260169412, -12.82831286325064823, 5.290680261490429359 ) ) ;
#6437 = AXIS2_PLACEMENT_3D ( 'NONE', #30816, #27984, #25794 ) ;
#6438 = CARTESIAN_POINT ( 'NONE',  ( 4.630235822890138131, 0.3309221515414816350, -15.14454535870000917 ) ) ;
#6439 = CARTESIAN_POINT ( 'NONE',  ( 3.155489075140835542, 3.034105443485036968, -34.82341724620000889 ) ) ;
#6440 = FACE_OUTER_BOUND ( 'NONE', #1933, .T. ) ;
#6441 = CARTESIAN_POINT ( 'NONE',  ( -8.000000000196104466, -28.90964379102386062, -30.74680062216425469 ) ) ;
#6442 = DIRECTION ( 'NONE',  ( -2.764840495839172514E-12, -0.9128796883888952163, 0.4082287037029530552 ) ) ;
#6443 = CARTESIAN_POINT ( 'NONE',  ( -18.35216541603009688, -21.08443583241201935, 8.000000000000007105 ) ) ;
#6444 = CARTESIAN_POINT ( 'NONE',  ( -3.610091233028032587, 0.7466883238378643206, 227.7538236713938602 ) ) ;
#6445 = EDGE_CURVE ( 'NONE', #21330, #3666, #2432, .T. ) ;
#6446 = CARTESIAN_POINT ( 'NONE',  ( 7.260640027522912376, -5.583405280045696806, -27.05081923603077243 ) ) ;
#6447 = CARTESIAN_POINT ( 'NONE',  ( 0.000000000000000000, 0.000000000000000000, 115.0000000000000000 ) ) ;
#6448 = CARTESIAN_POINT ( 'NONE',  ( -17.93586506597758046, 11.12395421520594851, -4.336808689942017736E-16 ) ) ;
#6449 = EDGE_CURVE ( 'NONE', #27396, #1557, #5425, .T. ) ;
#6450 = CARTESIAN_POINT ( 'NONE',  ( 27.63177356790000161, -3.383804547859999682E-15, 187.3605236429999934 ) ) ;
#6451 = VERTEX_POINT ( 'NONE', #211 ) ;
#6452 = B_SPLINE_CURVE_WITH_KNOTS ( 'NONE', 3,
 ( #22055, #506, #4753, #22199, #2392, #10090 ),
 .UNSPECIFIED., .F., .F.,
 ( 4, 2, 4 ),
 ( 0.000000000000000000, 0.5000000000000000000, 1.000000000000000000 ),
 .UNSPECIFIED. ) ;
#6453 = CARTESIAN_POINT ( 'NONE',  ( -0.6215321086153002828, -3.499999999999999556, 227.6701688388543516 ) ) ;
#6454 = CARTESIAN_POINT ( 'NONE',  ( -25.00949650980000172, -13.66806287920000074, 224.0985996330000205 ) ) ;
#6455 = CARTESIAN_POINT ( 'NONE',  ( 9.999999999953960383, -32.32189936811070652, -22.79484972463425052 ) ) ;
#6456 = ORIENTED_EDGE ( 'NONE', *, *, #3237, .F. ) ;
#6457 = CARTESIAN_POINT ( 'NONE',  ( 8.700000000285857737, -13.61366271048277277, -34.64064744186795508 ) ) ;
#6458 = VERTEX_POINT ( 'NONE', #14531 ) ;
#6459 = ORIENTED_EDGE ( 'NONE', *, *, #3637, .T. ) ;
#6460 = FILL_AREA_STYLE_COLOUR ( '', #7316 ) ;
#6461 = ORIENTED_EDGE ( 'NONE', *, *, #130, .F. ) ;
#6462 = PLANE ( 'NONE',  #28029 ) ;
#6463 = VERTEX_POINT ( 'NONE', #26947 ) ;
#6464 = CARTESIAN_POINT ( 'NONE',  ( -26.95773188389999930, 8.656139546040000354, 229.0000000000000000 ) ) ;
#6465 = SURFACE_STYLE_FILL_AREA ( #18424 ) ;
#6466 = DIRECTION ( 'NONE',  ( 0.000000000000000000, -0.7113488923935513686, 0.7028390664230806939 ) ) ;
#6467 = DIRECTION ( 'NONE',  ( -1.000000000000000000, 1.224606353819999829E-16, 0.000000000000000000 ) ) ;
#6468 = CARTESIAN_POINT ( 'NONE',  ( 8.700000000278096834, -14.92844969908683517, -33.25053330388887218 ) ) ;
#6469 = AXIS2_PLACEMENT_3D ( 'NONE', #19802, #29388, #24674 ) ;
#6470 = DIRECTION ( 'NONE',  ( 0.9316362575375356503, 0.3633921898465274913, 0.000000000000000000 ) ) ;
#6471 = CARTESIAN_POINT ( 'NONE',  ( -10.69999999999999929, -29.12132034360000077, -30.52132034359999935 ) ) ;
#6472 = CYLINDRICAL_SURFACE ( 'NONE', #31088, 1.700000000000000178 ) ;
#6473 = VERTEX_POINT ( 'NONE', #16713 ) ;
#6474 = ADVANCED_FACE ( 'NONE', ( #26330, #9640, #14378 ), #24125, .F. ) ;
#6475 = CARTESIAN_POINT ( 'NONE',  ( 2.773795135624238295, 4.340636736956414943, -6.138467428499996714 ) ) ;
#6476 = CARTESIAN_POINT ( 'NONE',  ( 0.1206012444329082195, -5.909053133798479962, -23.41888333260001431 ) ) ;
#6477 = CARTESIAN_POINT ( 'NONE',  ( -7.919194817802633679, -26.33574556704115466, 207.5082310198851019 ) ) ;
#6478 = CARTESIAN_POINT ( 'NONE',  ( -3.444197479758565272, 0.6290193758906742483, -91.21022354329026882 ) ) ;
#6479 = CARTESIAN_POINT ( 'NONE',  ( -7.707106781243226123, -115.2381289094444128, 21.69251968763726879 ) ) ;
#6480 = LINE ( 'NONE', #26153, #5593 ) ;
#6481 = CARTESIAN_POINT ( 'NONE',  ( -23.50695179570000093, -14.84192241259999889, 225.1042187089999800 ) ) ;
#6482 = AXIS2_PLACEMENT_3D ( 'NONE', #23568, #11592, #16308 ) ;
#6483 = CARTESIAN_POINT ( 'NONE',  ( 10.06596365874881194, -25.80632433378973900, 140.0000000000000000 ) ) ;
#6484 = CARTESIAN_POINT ( 'NONE',  ( 0.000000000000000000, 4.811145170119999648, -67.12721591429999535 ) ) ;
#6485 = CARTESIAN_POINT ( 'NONE',  ( 0.000000000000000000, 0.000000000000000000, 91.66046017469999185 ) ) ;
#6486 = ORIENTED_EDGE ( 'NONE', *, *, #13199, .T. ) ;
#6487 = CARTESIAN_POINT ( 'NONE',  ( -4.050122923326508584, -2.059172231882750559, -62.36424626872499033 ) ) ;
#6488 = CARTESIAN_POINT ( 'NONE',  ( -23.94793942741029724, -15.45149538080513452, 5.679609021710654737 ) ) ;
#6489 = VERTEX_POINT ( 'NONE', #17032 ) ;
#6490 = ORIENTED_EDGE ( 'NONE', *, *, #24998, .T. ) ;
#6491 = CARTESIAN_POINT ( 'NONE',  ( -3.674376064820711107, -26.54820124389934577, 20.19531595841323579 ) ) ;
#6492 = CARTESIAN_POINT ( 'NONE',  ( -5.430430790592723156, -2.746024268427175841, -27.96472909260000606 ) ) ;
#6493 = CIRCLE ( 'NONE', #26113, 27.23548387100000312 ) ;
#6494 = ORIENTED_EDGE ( 'NONE', *, *, #1629, .F. ) ;
#6495 = LINE ( 'NONE', #8531, #769 ) ;
#6496 = DIRECTION ( 'NONE',  ( 0.000000000000000000, 0.000000000000000000, 1.000000000000000000 ) ) ;
#6497 = AXIS2_PLACEMENT_3D ( 'NONE', #3326, #29297, #7889 ) ;
#6498 = VERTEX_POINT ( 'NONE', #12316 ) ;
#6499 = ORIENTED_EDGE ( 'NONE', *, *, #17874, .F. ) ;
#6500 = ORIENTED_EDGE ( 'NONE', *, *, #740, .F. ) ;
#6501 = CARTESIAN_POINT ( 'NONE',  ( 4.041451884329999800, 2.701186720849999812E-16, 227.9588918784999976 ) ) ;
#6502 = SURFACE_SIDE_STYLE ('',( #18139 ) ) ;
#6503 = ORIENTED_EDGE ( 'NONE', *, *, #9442, .T. ) ;
#6504 = CARTESIAN_POINT ( 'NONE',  ( -8.699999999650465554, -17.26991458595691142, -37.68063167936340108 ) ) ;
#6505 = CARTESIAN_POINT ( 'NONE',  ( 10.00000000000000000, 20.99999999990000887, -70.10000000019999788 ) ) ;
#6506 = CARTESIAN_POINT ( 'NONE',  ( 3.264631907946181855, 4.440493141956372902, -65.84226422542499790 ) ) ;
#6507 = ADVANCED_FACE ( 'NONE', ( #26635 ), #7736, .F. ) ;
#6508 = CARTESIAN_POINT ( 'NONE',  ( -13.75032424529999986, -27.60893268180000248, 229.0000000050000040 ) ) ;
#6509 = CARTESIAN_POINT ( 'NONE',  ( 0.000000000000000000, 0.000000000000000000, 230.8412452696274499 ) ) ;
#6510 = CARTESIAN_POINT ( 'NONE',  ( 26.49877067279999920, -8.898240373709999318, 222.0000000000000000 ) ) ;
#6511 = CARTESIAN_POINT ( 'NONE',  ( -23.52681767331053919, -12.83507605119044293, 5.909812226101280430 ) ) ;
#6512 = ORIENTED_EDGE ( 'NONE', *, *, #6232, .T. ) ;
#6513 = EDGE_CURVE ( 'NONE', #30472, #3626, #6934, .T. ) ;
#6514 = CARTESIAN_POINT ( 'NONE',  ( -20.12248395285567071, 20.00008950071413238, 0.3491021030798783231 ) ) ;
#6515 = STYLED_ITEM ( 'NONE', ( #23239 ), #688 ) ;
#6516 = AXIS2_PLACEMENT_3D ( 'NONE', #2830, #19364, #21419 ) ;
#6517 = CARTESIAN_POINT ( 'NONE',  ( -2.929853409778804263, 3.622264489389750874, -13.60352819869999763 ) ) ;
#6518 = CARTESIAN_POINT ( 'NONE',  ( 18.28658402242479397, 10.97998838177520931, -1.452769935612311825 ) ) ;
#6519 = CARTESIAN_POINT ( 'NONE',  ( 8.915309161273842875, 8.516764744512210328, 232.6627635626987853 ) ) ;
#6520 = EDGE_LOOP ( 'NONE', ( #374, #6390, #6388, #12606, #16024, #14058, #26207 ) ) ;
#6521 = CARTESIAN_POINT ( 'NONE',  ( 24.80399018339999628, -14.03663607480000053, 223.9201473980000117 ) ) ;
#6522 = CARTESIAN_POINT ( 'NONE',  ( 7.105427357599999217E-15, 3.552713678799999608E-15, 43.21714158840000408 ) ) ;
#6523 = CARTESIAN_POINT ( 'NONE',  ( -28.50000000000000000, 0.8733855473370000233, 222.0000000000000000 ) ) ;
#6524 = CARTESIAN_POINT ( 'NONE',  ( 9.799563951679273188, -25.69477015992459101, 26.17015415056619432 ) ) ;
#6525 = CARTESIAN_POINT ( 'NONE',  ( 23.20948082139999968, -13.40000000000000036, 3.900000000369999942 ) ) ;
#6526 = CLOSED_SHELL ( 'NONE', ( #18054, #16934, #28376, #11467, #18348, #10191, #23767, #24652, #26952, #25198, #12769, #11206, #30071, #13435, #3996, #7098, #8104, #19469, #29345, #1365, #14132, #29016 ) ) ;
#6527 = CARTESIAN_POINT ( 'NONE',  ( -17.52404053647086002, -8.139513033930352748, 0.000000000000000000 ) ) ;
#6528 = CARTESIAN_POINT ( 'NONE',  ( -11.04680313119999902, -24.61949706369999902, -1.636966784999999147 ) ) ;
#6529 = CYLINDRICAL_SURFACE ( 'NONE', #12771, 2.000000000000000000 ) ;
#6530 = VERTEX_POINT ( 'NONE', #22077 ) ;
#6531 = EDGE_CURVE ( 'NONE', #22923, #6605, #12559, .T. ) ;
#6532 = DIRECTION ( 'NONE',  ( 1.000000000000000000, -9.219999999999999084E-13, 4.710999999999999616E-12 ) ) ;
#6533 = CARTESIAN_POINT ( 'NONE',  ( -8.699999999997119815, -117.4706889483893377, 13.80759369055796526 ) ) ;
#6534 = CARTESIAN_POINT ( 'NONE',  ( 2.212761947522928985, -3.601507522846123077, -68.10000000002500542 ) ) ;
#6535 = CARTESIAN_POINT ( 'NONE',  ( -0.1113126278295802629, -20.50181238077258783, -27.47976714835654732 ) ) ;
#6536 = CARTESIAN_POINT ( 'NONE',  ( -3.961961208831939363, -0.8145944572358391200, -44.10000000002499121 ) ) ;
#6537 = VERTEX_POINT ( 'NONE', #19242 ) ;
#6538 = CARTESIAN_POINT ( 'NONE',  ( -8.516764330228012270, 8.915308721986194840, 232.6627637660202765 ) ) ;
#6539 = CARTESIAN_POINT ( 'NONE',  ( -5.001751348353093540, 2.318407806459778175, -66.57526299442500317 ) ) ;
#6540 = ORIENTED_EDGE ( 'NONE', *, *, #16660, .T. ) ;
#6541 = DIRECTION ( 'NONE',  ( -1.000000000000000000, 0.000000000000000000, 0.000000000000000000 ) ) ;
#6543 = ADVANCED_FACE ( 'NONE', ( #373 ), #2415, .F. ) ;
#6542 = CARTESIAN_POINT ( 'NONE',  ( -0.5564057544751848106, -3.564787113710755850, -88.52261276293012315 ) ) ;
#6544 = ORIENTED_EDGE ( 'NONE', *, *, #13679, .T. ) ;
#6545 = CARTESIAN_POINT ( 'NONE',  ( 19.80538212960000166, 19.50875458629999670, 229.0000000010000178 ) ) ;
#6546 = CARTESIAN_POINT ( 'NONE',  ( -10.69999999999999929, -127.2537393281999982, -34.36317439833000265 ) ) ;
#6547 = CARTESIAN_POINT ( 'NONE',  ( 10.45000000009999930, -23.82317073171000033, -28.39999999989999679 ) ) ;
#6548 = CARTESIAN_POINT ( 'NONE',  ( -3.350725639047746007, 1.107490566396344356, 0.000000000000000000 ) ) ;
#6549 = EDGE_CURVE ( 'NONE', #10339, #22309, #3244, .T. ) ;
#6550 = CARTESIAN_POINT ( 'NONE',  ( -0.6094664100040195764, -28.49364619262437870, 4.999998581000003384 ) ) ;
#6551 = CARTESIAN_POINT ( 'NONE',  ( -12.75378086759999796, -22.00000000000000000, -25.51324865357000249 ) ) ;
#6552 = CARTESIAN_POINT ( 'NONE',  ( 8.700000000236576270, -29.80249410823907752, -29.47052640017699687 ) ) ;
#6553 = ORIENTED_EDGE ( 'NONE', *, *, #23556, .F. ) ;
#6554 = CYLINDRICAL_SURFACE ( 'NONE', #22542, 3.000000000000002220 ) ;
#6555 = CARTESIAN_POINT ( 'NONE',  ( 10.69999999999999929, -27.00000000000000000, -25.39999999999999858 ) ) ;
#6556 = CARTESIAN_POINT ( 'NONE',  ( 18.41899666859999840, 20.00000949010000184, 230.6632774530000063 ) ) ;
#6557 = CARTESIAN_POINT ( 'NONE',  ( -17.91528966515560484, -8.768795348586470695, 0.000000000000000000 ) ) ;
#6558 = LINE ( 'NONE', #18368, #605 ) ;
#6559 = CARTESIAN_POINT ( 'NONE',  ( -1.015151870880000029, -28.48229306780000059, 225.5064930660000186 ) ) ;
#6560 = CARTESIAN_POINT ( 'NONE',  ( 10.35667741062603397, -26.55163333981976592, 140.0000000000000000 ) ) ;
#6561 = CARTESIAN_POINT ( 'NONE',  ( -16.06988921239048551, -8.208160914692745891, -0.6999999999999784173 ) ) ;
#6562 = CARTESIAN_POINT ( 'NONE',  ( 5.066518387468507356, -3.138291312573631586, -49.33324460762499797 ) ) ;
#6563 = EDGE_CURVE ( 'NONE', #22118, #27093, #29447, .T. ) ;
#6564 = FACE_OUTER_BOUND ( 'NONE', #13866, .T. ) ;
#6565 = CARTESIAN_POINT ( 'NONE',  ( -7.521481332671076103, -6.600127069647881761, -34.26007211057947899 ) ) ;
#6566 = CARTESIAN_POINT ( 'NONE',  ( -1.505510951065242020, -9.645525760189025632, -102.7632020892250040 ) ) ;
#6567 = B_SPLINE_CURVE_WITH_KNOTS ( 'NONE', 3,
 ( #10098, #7421, #24420, #22371, #28978, #2552 ),
 .UNSPECIFIED., .F., .F.,
 ( 4, 2, 4 ),
 ( 0.000000000000000000, 0.5000000000000000000, 1.000000000000000000 ),
 .UNSPECIFIED. ) ;
#6568 = DIRECTION ( 'NONE',  ( 2.415891560877031462E-12, -0.9341647027306021478, -0.3568421334038983650 ) ) ;
#6569 = VERTEX_POINT ( 'NONE', #15289 ) ;
#6570 = B_SPLINE_CURVE_WITH_KNOTS ( 'NONE', 3,
 ( #17552, #24802, #23546, #23225, #25436, #6063, #1667, #4339, #21171, #1826, #25267, #25746, #16131, #23394, #11264, #11107, #11417, #18338 ),
 .UNSPECIFIED., .F., .F.,
 ( 4, 2, 2, 2, 2, 2, 2, 2, 4 ),
 ( 0.000000000000000000, 0.1250000000000000000, 0.2500000000000000000, 0.3750000000000000000, 0.5000000000000000000, 0.6250000000000000000, 0.7500000000000000000, 0.8750000000000000000, 1.000000000000000000 ),
 .UNSPECIFIED. ) ;
#6571 = CARTESIAN_POINT ( 'NONE',  ( -23.95524095760000094, -14.10746636989999914, 223.9201349020000009 ) ) ;
#6572 = ORIENTED_EDGE ( 'NONE', *, *, #15208, .F. ) ;
#6573 = CARTESIAN_POINT ( 'NONE',  ( -1.192105394233154314, -5.728767129463715690, -53.72706695232499641 ) ) ;
#6574 = EDGE_LOOP ( 'NONE', ( #6808, #13904, #23389, #20459 ) ) ;
#6575 = SHAPE_DEFINITION_REPRESENTATION ( #4378, #24039 ) ;
#6576 = ORIENTED_EDGE ( 'NONE', *, *, #3135, .T. ) ;
#6577 = APPLICATION_CONTEXT ( 'automotive_design' ) ;
#6579 = EDGE_CURVE ( 'NONE', #19663, #28945, #22318, .T. ) ;
#6578 = CYLINDRICAL_SURFACE ( 'NONE', #4548, 3.000000000000000444 ) ;
#6580 = ORIENTED_EDGE ( 'NONE', *, *, #21512, .F. ) ;
#6581 = CARTESIAN_POINT ( 'NONE',  ( 14.80403571755123870, -30.27061049443689456, -24.51513120827885217 ) ) ;
#6582 = DIRECTION ( 'NONE',  ( -1.000000000000000000, 1.646361269960000031E-16, 1.110223024630000146E-15 ) ) ;
#6583 = FACE_BOUND ( 'NONE', #13743, .T. ) ;
#6584 = EDGE_CURVE ( 'NONE', #22335, #19928, #12774, .T. ) ;
#6585 = AXIS2_PLACEMENT_3D ( 'NONE', #9296, #7252, #11663 ) ;
#6586 = CARTESIAN_POINT ( 'NONE',  ( -8.999999999710000864, 21.35000000010000321, -45.09999999954499827 ) ) ;
#6587 = CARTESIAN_POINT ( 'NONE',  ( -1.100000000000000089, -27.47799119230000287, 5.000000000000000000 ) ) ;
#6588 = CARTESIAN_POINT ( 'NONE',  ( 27.50000000000000000, -3.367667472999999580E-15, 93.28090191849999258 ) ) ;
#6589 = CARTESIAN_POINT ( 'NONE',  ( 1.699015317690025118, 6.330513620609809600, -2.053410702900000828 ) ) ;
#6590 = CARTESIAN_POINT ( 'NONE',  ( 26.80000000000000071, -7.020799968500000432, 230.6999999999999886 ) ) ;
#6591 = ORIENTED_EDGE ( 'NONE', *, *, #16433, .F. ) ;
#6592 = PLANE ( 'NONE',  #5943 ) ;
#6593 = EDGE_CURVE ( 'NONE', #6773, #12147, #11301, .T. ) ;
#6594 = CARTESIAN_POINT ( 'NONE',  ( 3.904356169178446745, -3.871725997715349532, -16.06112212870000633 ) ) ;
#6595 = CARTESIAN_POINT ( 'NONE',  ( -5.496316421720869982, 0.7952554554161578304, -33.25783976330001224 ) ) ;
#6596 = DIRECTION ( 'NONE',  ( -0.000000000000000000, -0.000000000000000000, 1.000000000000000000 ) ) ;
#6597 = CARTESIAN_POINT ( 'NONE',  ( 0.9902601295740001142, -27.78262976010000074, 224.4935313260000100 ) ) ;
#6598 = CARTESIAN_POINT ( 'NONE',  ( 8.737549905436626574, -27.40075442753056478, 8.000000000000007105 ) ) ;
#6599 = CARTESIAN_POINT ( 'NONE',  ( -10.00000000000000000, 21.70000000000000284, -62.10000000019999788 ) ) ;
#6600 = FACE_OUTER_BOUND ( 'NONE', #6420, .T. ) ;
#6601 = CARTESIAN_POINT ( 'NONE',  ( 0.3786683407719231842, -3.509503079120984026, 226.6412452697750268 ) ) ;
#6602 = CARTESIAN_POINT ( 'NONE',  ( 8.999999999770000869, 21.00000000069999473, -48.10000000000000142 ) ) ;
#6603 = DIRECTION ( 'NONE',  ( 0.000000000000000000, 0.000000000000000000, 1.000000000000000000 ) ) ;
#6604 = AXIS2_PLACEMENT_3D ( 'NONE', #26883, #29701, #25136 ) ;
#6605 = VERTEX_POINT ( 'NONE', #20012 ) ;
#6606 = CARTESIAN_POINT ( 'NONE',  ( 5.228182028002445136, -31.46370949612416723, -80.33018326515686169 ) ) ;
#6607 = CARTESIAN_POINT ( 'NONE',  ( 2.317629466759838053, -2.355760913644644461, -36.33018780266829850 ) ) ;
#6608 = CARTESIAN_POINT ( 'NONE',  ( -2.813083154009999692E-14, -26.79999999949999889, 3.899999999999999911 ) ) ;
#6609 = EDGE_LOOP ( 'NONE', ( #8458, #14631, #10183, #3130, #4610, #7151, #8339, #24576, #13958, #4070, #18935, #17773 ) ) ;
#6610 = CARTESIAN_POINT ( 'NONE',  ( 3.498556269673057884, -2.323812390827893815, -44.10875473022500159 ) ) ;
#6611 = ORIENTED_EDGE ( 'NONE', *, *, #23730, .T. ) ;
#6612 = ORIENTED_EDGE ( 'NONE', *, *, #20386, .T. ) ;
#6613 = ORIENTED_EDGE ( 'NONE', *, *, #21500, .F. ) ;
#6614 = DIRECTION ( 'NONE',  ( 0.000000000000000000, 0.000000000000000000, -1.000000000000000000 ) ) ;
#6615 = EDGE_CURVE ( 'NONE', #26866, #22866, #830, .T. ) ;
#6616 = ORIENTED_EDGE ( 'NONE', *, *, #22230, .F. ) ;
#6617 = CARTESIAN_POINT ( 'NONE',  ( -4.276011752264103016, -42.94729992905724458, -9.547410993472157159 ) ) ;
#6618 = CARTESIAN_POINT ( 'NONE',  ( -8.699999998940043611, -18.28443321518998133, -36.42483785847389299 ) ) ;
#6619 =( NAMED_UNIT ( * ) SI_UNIT ( $, .STERADIAN. ) SOLID_ANGLE_UNIT ( ) );
#6620 = EDGE_CURVE ( 'NONE', #29101, #29098, #10420, .T. ) ;
#6621 = EDGE_CURVE ( 'NONE', #28198, #23146, #5814, .T. ) ;
#6622 = CARTESIAN_POINT ( 'NONE',  ( 0.4478609109089253248, -28.49673184309138918, 3.901345920999998995 ) ) ;
#6623 = ADVANCED_FACE ( 'NONE', ( #13074 ), #17790, .T. ) ;
#6624 = CARTESIAN_POINT ( 'NONE',  ( 21.09633121001184719, -16.56519925036682039, -1.399999999999998579 ) ) ;
#6625 = CARTESIAN_POINT ( 'NONE',  ( -26.80000000110000613, -1.759504892044711388, -0.000000000000000000 ) ) ;
#6626 = CARTESIAN_POINT ( 'NONE',  ( -18.15350094950000326, 19.92137095469999863, 229.9929676959999938 ) ) ;
#6627 = ORIENTED_EDGE ( 'NONE', *, *, #795, .T. ) ;
#6628 = AXIS2_PLACEMENT_3D ( 'NONE', #9584, #2507, #16507 ) ;
#6629 = CARTESIAN_POINT ( 'NONE',  ( 5.506451109007332256, 0.7220432749125509364, -6.626979598400000171 ) ) ;
#6630 = CARTESIAN_POINT ( 'NONE',  ( 4.725722714813314518, -3.873618144263061946, -23.99674734060000603 ) ) ;
#6631 = CARTESIAN_POINT ( 'NONE',  ( 27.92857142860000152, -3.116236426490000064E-16, 42.06031501460000044 ) ) ;
#6632 = PRODUCT_DEFINITION_SHAPE ( 'NONE', 'NONE',  #15768 ) ;
#6633 = FACE_OUTER_BOUND ( 'NONE', #17150, .T. ) ;
#6634 = CARTESIAN_POINT ( 'NONE',  ( -1.833239707770263127, 3.499999999998122391, 227.9047692640812670 ) ) ;
#6635 = CARTESIAN_POINT ( 'NONE',  ( -25.39337327098795072, 12.94027895355586288, 5.560810202636621291 ) ) ;
#6636 = CARTESIAN_POINT ( 'NONE',  ( -8.903108651239966420, -22.82508830966961000, 90.00000000000000000 ) ) ;
#6637 = CARTESIAN_POINT ( 'NONE',  ( 23.83325788290921565, -14.31210125041407899, 5.496144292502794571 ) ) ;
#6638 = FACE_OUTER_BOUND ( 'NONE', #4743, .T. ) ;
#6639 = CARTESIAN_POINT ( 'NONE',  ( 8.699999999499924641, -28.07052640022601864, -25.59750589169981438 ) ) ;
#6640 = ORIENTED_EDGE ( 'NONE', *, *, #3084, .T. ) ;
#6641 = CARTESIAN_POINT ( 'NONE',  ( -5.623491485972666126, 3.092612689740418919, -59.81908057272499946 ) ) ;
#6642 = CARTESIAN_POINT ( 'NONE',  ( -24.37821945910799926, 14.76389285725497125, 5.208432825000025801 ) ) ;
#6643 = EDGE_LOOP ( 'NONE', ( #25826, #25096, #22427, #14606 ) ) ;
#6644 = ORIENTED_EDGE ( 'NONE', *, *, #2166, .T. ) ;
#6645 = CARTESIAN_POINT ( 'NONE',  ( 0.6243462152986178904, -28.49342029039284085, 3.904048352000033528 ) ) ;
#6646 = CARTESIAN_POINT ( 'NONE',  ( 5.972505199797514486, -1.290950946386169917, -23.79036215650000230 ) ) ;
#6647 = ORIENTED_EDGE ( 'NONE', *, *, #27996, .F. ) ;
#6648 = CARTESIAN_POINT ( 'NONE',  ( -24.25452752885752261, 13.58678145142700622, 3.899998581000042819 ) ) ;
#6649 = CARTESIAN_POINT ( 'NONE',  ( -1.976074114793839431, 0.3084332875059758727, 229.1412452697749984 ) ) ;
#6651 = ORIENTED_EDGE ( 'NONE', *, *, #18385, .T. ) ;
#6650 = CIRCLE ( 'NONE', #15180, 2.000000000000000000 ) ;
#6652 = ORIENTED_EDGE ( 'NONE', *, *, #7023, .F. ) ;
#6653 = ORIENTED_EDGE ( 'NONE', *, *, #1113, .T. ) ;
#6654 = B_SPLINE_SURFACE_WITH_KNOTS ( 'NONE', 5, 1, ( 
 ( #8996, #18748 ),
 ( #28037, #6481 ),
 ( #11366, #21273 ),
 ( #28351, #30569 ),
 ( #23645, #6796 ),
 ( #6166, #18278 ),
 ( #25850, #4126 ),
 ( #13569, #11674 ),
 ( #20649, #9307 ),
 ( #23333, #11205 ),
 ( #30877, #11057 ),
 ( #1615, #25999 ),
 ( #28193, #13722 ),
 ( #4441, #27722 ),
 ( #25381, #23492 ) ),
 .UNSPECIFIED., .F., .F., .F.,
 ( 6, 3, 3, 3, 6 ),
 ( 2, 2 ),
 ( 0.000000000000000000, 0.5239055193870000293, 1.047811038780000148, 1.571716558160000110, 1.746351731290000098 ),
 ( -0.7000000000009999335, 2.557291473029999731E-06 ),
 .UNSPECIFIED. ) ;
#6655 = ORIENTED_EDGE ( 'NONE', *, *, #30577, .T. ) ;
#6656 = FACE_OUTER_BOUND ( 'NONE', #29148, .T. ) ;
#6657 = DIRECTION ( 'NONE',  ( -1.000000000000000000, 0.000000000000000000, -2.257144471330000330E-12 ) ) ;
#6658 = CARTESIAN_POINT ( 'NONE',  ( 5.384875807261761516, 2.601783486389667832, -66.85315453642499506 ) ) ;
#6659 = CARTESIAN_POINT ( 'NONE',  ( 6.585786437629999490, -16.41511111490214603, -74.85294138696069410 ) ) ;
#6660 = B_SPLINE_CURVE_WITH_KNOTS ( 'NONE', 3,
 ( #1378, #5356, #27068, #14961, #13327, #10088, #27639, #12588 ),
 .UNSPECIFIED., .F., .F.,
 ( 4, 2, 2, 4 ),
 ( 0.000000000000000000, 0.2499999999999985567, 0.4999999999999971134, 1.000000000000000000 ),
 .UNSPECIFIED. ) ;
#6661 = CARTESIAN_POINT ( 'NONE',  ( -8.000000000444114079, -28.22468611108740788, -31.13863906519029001 ) ) ;
#6663 = TOROIDAL_SURFACE ( 'NONE', #24253, 29.80000000000000071, 3.000000000000000000 ) ;
#6662 = CARTESIAN_POINT ( 'NONE',  ( 20.95194113719999862, -19.55023117750000239, 222.0000000000000000 ) ) ;
#6664 = DIRECTION ( 'NONE',  ( 0.6343890248118319031, 0.7730139489027950672, 0.000000000000000000 ) ) ;
#6665 = EDGE_LOOP ( 'NONE', ( #19155, #19826, #14563, #18782 ) ) ;
#6666 = CARTESIAN_POINT ( 'NONE',  ( -18.93738424706367951, 20.00019831485299093, -0.5298795608970631177 ) ) ;
#6667 = CARTESIAN_POINT ( 'NONE',  ( 1.086829820489895848, 5.988658659452708477, -13.42400681849999877 ) ) ;
#6668 = CARTESIAN_POINT ( 'NONE',  ( -9.897162125403683675, -25.37356426577969870, 41.66046017469999896 ) ) ;
#6669 = LINE ( 'NONE', #6365, #19566 ) ;
#6670 = AXIS2_PLACEMENT_3D ( 'NONE', #17509, #24605, #24290 ) ;
#6671 = ORIENTED_EDGE ( 'NONE', *, *, #15437, .F. ) ;
#6672 = CARTESIAN_POINT ( 'NONE',  ( -23.23277431133845994, -15.26692929363520257, 4.999998581000003384 ) ) ;
#6673 = FACE_OUTER_BOUND ( 'NONE', #8686, .T. ) ;
#6674 = CARTESIAN_POINT ( 'NONE',  ( -27.76736547790000031, 1.703869260230000071, 222.0000000000000000 ) ) ;
#6675 = CARTESIAN_POINT ( 'NONE',  ( 7.919194817802646114, -26.33574556704115111, 22.49176898011488035 ) ) ;
#6676 = CARTESIAN_POINT ( 'NONE',  ( -16.83342759582943060, -8.999999999996580513, -0.6999999999999784173 ) ) ;
#6677 = DIRECTION ( 'NONE',  ( 0.000000000000000000, 0.000000000000000000, 1.000000000000000000 ) ) ;
#6678 = CARTESIAN_POINT ( 'NONE',  ( 24.98081130624543889, 13.71897605842228529, 4.999998581000003384 ) ) ;
#6679 = CARTESIAN_POINT ( 'NONE',  ( -7.534632680830990026, -7.897185061638417380, -36.96526048005145526 ) ) ;
#6680 = ORIENTED_EDGE ( 'NONE', *, *, #8815, .T. ) ;
#6681 = ADVANCED_FACE ( 'NONE', ( #1127 ), #10718, .T. ) ;
#6682 = DIRECTION ( 'NONE',  ( 0.000000000000000000, 0.000000000000000000, 1.000000000000000000 ) ) ;
#6683 = B_SPLINE_CURVE_WITH_KNOTS ( 'NONE', 3,
 ( #20839, #25722, #13750, #9024, #18622, #25879 ),
 .UNSPECIFIED., .F., .F.,
 ( 4, 2, 4 ),
 ( 0.000000000000000000, 0.5000000000000000000, 1.000000000000000000 ),
 .UNSPECIFIED. ) ;
#6684 = CARTESIAN_POINT ( 'NONE',  ( 2.410831077383560839, -3.533047124804223671, -68.10000000002500542 ) ) ;
#6685 = ADVANCED_FACE ( 'NONE', ( #20318 ), #29918, .T. ) ;
#6686 = CARTESIAN_POINT ( 'NONE',  ( 4.665340848529999640, 5.684798146329999469, 228.3912452697800006 ) ) ;
#6687 = CARTESIAN_POINT ( 'NONE',  ( -3.771147929147382172, -1.309395846178109668, -44.10000000002499121 ) ) ;
#6688 = AXIS2_PLACEMENT_3D ( 'NONE', #30384, #15736, #8969 ) ;
#6689 = B_SPLINE_CURVE_WITH_KNOTS ( 'NONE', 3,
 ( #4123, #30715, #21431, #9144, #13880, #13719, #18745, #23330, #28502, #16541 ),
 .UNSPECIFIED., .F., .F.,
 ( 4, 2, 2, 2, 4 ),
 ( 0.000000000000000000, 0.2500000000000000000, 0.5000000000000000000, 0.7500000000000000000, 1.000000000000000000 ),
 .UNSPECIFIED. ) ;
#6690 = ORIENTED_EDGE ( 'NONE', *, *, #503, .F. ) ;
#6691 = CARTESIAN_POINT ( 'NONE',  ( -10.00000000057657878, -24.00000000000020250, -28.00730091830135393 ) ) ;
#6692 = AXIS2_PLACEMENT_3D ( 'NONE', #28664, #2085, #26311 ) ;
#6693 = CARTESIAN_POINT ( 'NONE',  ( 3.264631907946181855, 4.440493141956372902, -67.44226422552499400 ) ) ;
#6694 = VERTEX_POINT ( 'NONE', #13224 ) ;
#6695 = FACE_OUTER_BOUND ( 'NONE', #19854, .T. ) ;
#6696 = CARTESIAN_POINT ( 'NONE',  ( -3.521042344302073079, -0.5632927345592675383, -88.52261276306772686 ) ) ;
#6697 = ORIENTED_EDGE ( 'NONE', *, *, #29829, .F. ) ;
#6698 = LINE ( 'NONE', #9364, #9530 ) ;
#6699 = DIRECTION ( 'NONE',  ( -1.595945597898660305E-12, -0.7071067811865475727, 0.7071067811865475727 ) ) ;
#6700 = CARTESIAN_POINT ( 'NONE',  ( -27.50000000000000000, 3.367667473009999970E-15, 115.0000000010000036 ) ) ;
#6701 = CARTESIAN_POINT ( 'NONE',  ( -9.738910687886855655, -24.96785170200598714, 36.78285841123146582 ) ) ;
#6702 = CYLINDRICAL_SURFACE ( 'NONE', #29379, 3.000000000000003997 ) ;
#6703 = CARTESIAN_POINT ( 'NONE',  ( -16.71067332636193115, -10.09794851200387278, 0.000000000000000000 ) ) ;
#6704 = DIRECTION ( 'NONE',  ( 1.000000000000000000, -0.000000000000000000, -2.257150022439999944E-12 ) ) ;
#6705 = EDGE_CURVE ( 'NONE', #21828, #8486, #4524, .T. ) ;
#6706 = ORIENTED_EDGE ( 'NONE', *, *, #23158, .F. ) ;
#6707 = CARTESIAN_POINT ( 'NONE',  ( 21.17669550445266680, 18.05242248062137023, 5.000000000000004441 ) ) ;
#6708 = CARTESIAN_POINT ( 'NONE',  ( 9.993285220779439371, -25.61999708228226069, 115.0000000000000000 ) ) ;
#6709 = VECTOR ( 'NONE', #30806, 1000.000000000000114 ) ;
#6710 = CARTESIAN_POINT ( 'NONE',  ( -1.776417072969999733, 11.98130592599999922, 231.9999989789999972 ) ) ;
#6711 = CARTESIAN_POINT ( 'NONE',  ( -2.748065355775931806, -2.239845275112382961, 230.8106057538883249 ) ) ;
#6712 = CARTESIAN_POINT ( 'NONE',  ( -12.31403527400738085, -29.89465053769069414, -32.50227542495312605 ) ) ;
#6713 = TOROIDAL_SURFACE ( 'NONE', #11748, 29.80000000000000071, 3.000000000000000000 ) ;
#6714 = FACE_OUTER_BOUND ( 'NONE', #22956, .T. ) ;
#6715 = CARTESIAN_POINT ( 'NONE',  ( 9.999999999970887288, -23.99999999999979394, -28.79269908193450789 ) ) ;
#6716 = CARTESIAN_POINT ( 'NONE',  ( 1.070950144331349163, -27.77958776724596746, 224.7107472884561048 ) ) ;
#6717 = CARTESIAN_POINT ( 'NONE',  ( 3.615638736154061839, -2.931608942551765740, -54.65923804942499942 ) ) ;
#6718 = CARTESIAN_POINT ( 'NONE',  ( -27.79539923781770483, -0.5057481688778011630, 1.000000000000000888 ) ) ;
#6719 = CARTESIAN_POINT ( 'NONE',  ( -6.851801499143887142, -7.170286489046357126, -33.98198678106104609 ) ) ;
#6720 = DIRECTION ( 'NONE',  ( 0.000000000000000000, -2.257145581549999994E-12, -1.000000000000000000 ) ) ;
#6721 = EDGE_CURVE ( 'NONE', #28711, #25555, #15591, .T. ) ;
#6722 = CARTESIAN_POINT ( 'NONE',  ( -23.92402432643254073, -13.56054118780705231, 223.9122931972334811 ) ) ;
#6723 = CARTESIAN_POINT ( 'NONE',  ( -24.62906106470000012, -14.34164290000000008, 223.9040321109999923 ) ) ;
#6724 = AXIS2_PLACEMENT_3D ( 'NONE', #17954, #14891, #29187 ) ;
#6725 = ORIENTED_EDGE ( 'NONE', *, *, #6052, .T. ) ;
#6726 = CARTESIAN_POINT ( 'NONE',  ( 4.390418465364303025, -3.559810858781688125, -55.88923804942498919 ) ) ;
#6727 = VECTOR ( 'NONE', #24335, 1000.000000000000000 ) ;
#6728 = ORIENTED_EDGE ( 'NONE', *, *, #24020, .F. ) ;
#6729 = CIRCLE ( 'NONE', #20827, 1.099999999570000497 ) ;
#6730 = B_SPLINE_CURVE_WITH_KNOTS ( 'NONE', 3,
 ( #26367, #12494, #2300, #10145, #4813, #11883, #21487, #19744, #7162, #16749, #14408, #2449 ),
 .UNSPECIFIED., .F., .F.,
 ( 4, 2, 2, 2, 2, 4 ),
 ( 0.000000000000000000, 0.2500000000000005551, 0.5000000000000011102, 0.6250000000000004441, 0.7499999999999998890, 1.000000000000000000 ),
 .UNSPECIFIED. ) ;
#6731 = AXIS2_PLACEMENT_3D ( 'NONE', #13960, #19761, #22120 ) ;
#6732 = VERTEX_POINT ( 'NONE', #20471 ) ;
#6733 = DIRECTION ( 'NONE',  ( 1.000000000000000000, -3.980999999999999294E-12, 1.940999999999999504E-12 ) ) ;
#6734 = ORIENTED_EDGE ( 'NONE', *, *, #633, .T. ) ;
#6735 = EDGE_CURVE ( 'NONE', #15021, #9398, #9556, .T. ) ;
#6736 = CARTESIAN_POINT ( 'NONE',  ( -28.49528339128749366, -0.5184828350247674411, 1.000000000000000888 ) ) ;
#6737 = CARTESIAN_POINT ( 'NONE',  ( -15.73360964037622622, -8.979988381802643360, -0.6999999999999784173 ) ) ;
#6738 = DIRECTION ( 'NONE',  ( -0.7071067811896790678, -0.6355433650254203037, 0.3099752105697111682 ) ) ;
#6739 = EDGE_CURVE ( 'NONE', #13665, #24204, #18423, .T. ) ;
#6740 = CARTESIAN_POINT ( 'NONE',  ( -4.962952493270000431, -10.92748134360000023, 231.9999991140000191 ) ) ;
#6741 = CARTESIAN_POINT ( 'NONE',  ( -10.00000000000000000, 3.868893114322062843, -67.47016761578689170 ) ) ;
#6742 = CARTESIAN_POINT ( 'NONE',  ( -9.414213562409999625, -15.31419272936388687, -74.45223986426802298 ) ) ;
#6743 = CARTESIAN_POINT ( 'NONE',  ( 3.194067125856711264, 4.998308969841025906, -4.200967428500002931 ) ) ;
#6744 = PRESENTATION_LAYER_ASSIGNMENT (  '', '', ( #30882 ) ) ;
#6745 = CARTESIAN_POINT ( 'NONE',  ( 5.334905827900000119, -31.46243374959999883, 229.7625741969999922 ) ) ;
#6746 = ORIENTED_EDGE ( 'NONE', *, *, #10073, .F. ) ;
#6747 = DIRECTION ( 'NONE',  ( -1.000000000000000000, 0.000000000000000000, 0.000000000000000000 ) ) ;
#6748 = EDGE_CURVE ( 'NONE', #29523, #23857, #18582, .T. ) ;
#6749 = CARTESIAN_POINT ( 'NONE',  ( 3.390625094264292372, -3.362288366427768072, -15.99862212869999922 ) ) ;
#6750 = CARTESIAN_POINT ( 'NONE',  ( -0.3280975466111886174, 4.681158999438242319, -34.39518930510001127 ) ) ;
#6751 = AXIS2_PLACEMENT_3D ( 'NONE', #17434, #29706, #5328 ) ;
#6752 = CARTESIAN_POINT ( 'NONE',  ( 8.000000000354901886, -27.70368077928761252, -25.45737431365605019 ) ) ;
#6753 = CARTESIAN_POINT ( 'NONE',  ( -24.09302906149999757, -13.87041066189999938, 223.9000014189999774 ) ) ;
#6754 = CIRCLE ( 'NONE', #25334, 2.000000000000002220 ) ;
#6755 = CARTESIAN_POINT ( 'NONE',  ( -7.999999999628144565, -17.92644052945513522, -41.00309170034211093 ) ) ;
#6756 = CARTESIAN_POINT ( 'NONE',  ( -3.947708767128641938, 0.1623678418503206877, 227.9047692640809544 ) ) ;
#6757 = AXIS2_PLACEMENT_3D ( 'NONE', #4766, #201, #19393 ) ;
#6758 = AXIS2_PLACEMENT_3D ( 'NONE', #21733, #23641, #2078 ) ;
#6759 = DIRECTION ( 'NONE',  ( 0.4353787270609797422, 0.9002473904559573636, 0.000000000000000000 ) ) ;
#6760 = CARTESIAN_POINT ( 'NONE',  ( 11.50000000000000000, 21.72305290929948640, -60.97178489257708378 ) ) ;
#6761 = CARTESIAN_POINT ( 'NONE',  ( -24.34663841809999951, -12.78636765230000094, 225.0000000000000000 ) ) ;
#6762 = EDGE_CURVE ( 'NONE', #17135, #28330, #22706, .T. ) ;
#6763 = CARTESIAN_POINT ( 'NONE',  ( 2.590102362141937675, 2.513801395321815679, 230.7730491447829877 ) ) ;
#6764 = ORIENTED_EDGE ( 'NONE', *, *, #27337, .T. ) ;
#6765 = CARTESIAN_POINT ( 'NONE',  ( -11.54917764160000004, 19.99999999999999645, -0.6999999992999966780 ) ) ;
#6766 =( REPRESENTATION_RELATIONSHIP ('NONE','NONE', #2712, #20626 ) REPRESENTATION_RELATIONSHIP_WITH_TRANSFORMATION ( #13981 )SHAPE_REPRESENTATION_RELATIONSHIP( ) );
#6767 = DIRECTION ( 'NONE',  ( 0.000000000000000000, 0.3420201433259318913, -0.9396926207858126157 ) ) ;
#6768 = COLOUR_RGB ( '', 0.31764706, 0.68627451, 0.89019608) ;
#6769 = ORIENTED_EDGE ( 'NONE', *, *, #13506, .T. ) ;
#6770 = CARTESIAN_POINT ( 'NONE',  ( -3.948109860491266776, 2.321589337205137937, -44.84354844312500177 ) ) ;
#6771 = VERTEX_POINT ( 'NONE', #1908 ) ;
#6772 = EDGE_CURVE ( 'NONE', #13384, #18572, #26827, .T. ) ;
#6773 = VERTEX_POINT ( 'NONE', #18730 ) ;
#6774 = CARTESIAN_POINT ( 'NONE',  ( 0.000000000000000000, 0.000000000000000000, 0.000000000000000000 ) ) ;
#6775 = VERTEX_POINT ( 'NONE', #6617 ) ;
#6776 = CARTESIAN_POINT ( 'NONE',  ( 18.17096580360000146, 20.37181511329999850, 230.6577119970000069 ) ) ;
#6777 = CIRCLE ( 'NONE', #28390, 1.700000000000000178 ) ;
#6778 = VERTEX_POINT ( 'NONE', #13708 ) ;
#6779 = B_SPLINE_CURVE_WITH_KNOTS ( 'NONE', 5,
 ( #28665, #2396, #13886, #2246, #11836, #6798, #4291, #21436, #31030 ),
 .UNSPECIFIED., .F., .F.,
 ( 6, 3, 6 ),
 ( 0.000000000000000000, 1.472643962950000329, 1.642768356969999788 ),
 .UNSPECIFIED. ) ;
#6780 = CARTESIAN_POINT ( 'NONE',  ( -25.00949650969999993, -13.66806287920000074, 225.9014032059999977 ) ) ;
#6781 = CARTESIAN_POINT ( 'NONE',  ( 23.57322167201500562, 14.73624931484498291, 3.997250016000014838 ) ) ;
#6782 = DIRECTION ( 'NONE',  ( 0.000000000000000000, 0.000000000000000000, -1.000000000000000000 ) ) ;
#6783 = CARTESIAN_POINT ( 'NONE',  ( 1.789657965652164728, 3.567538649943624129, -35.69999999999999574 ) ) ;
#6784 = CARTESIAN_POINT ( 'NONE',  ( 18.06290775522712977, 19.99992683950017636, -0.6936597257213343859 ) ) ;
#6785 = CARTESIAN_POINT ( 'NONE',  ( -9.000000000000000000, -54.99999999999998579, -42.39999999999999858 ) ) ;
#6786 = CARTESIAN_POINT ( 'NONE',  ( 3.361916939940001292, -1.176989049201372595, 227.6811464142205068 ) ) ;
#6787 = CARTESIAN_POINT ( 'NONE',  ( -18.80718603000000044, 20.00000136549999752, 230.5856263059999947 ) ) ;
#6788 = ORIENTED_EDGE ( 'NONE', *, *, #19672, .F. ) ;
#6789 = CARTESIAN_POINT ( 'NONE',  ( 4.347198243976404974, 0.5700341643805826308, -5.626979598400000171 ) ) ;
#6790 = CARTESIAN_POINT ( 'NONE',  ( -0.4966384047618531139, 4.769028251466922441, -24.95153409330000116 ) ) ;
#6791 = PLANE ( 'NONE',  #14356 ) ;
#6792 = MECHANICAL_DESIGN_GEOMETRIC_PRESENTATION_REPRESENTATION (  '', ( #5295 ), #16853 ) ;
#6793 = FACE_BOUND ( 'NONE', #28632, .T. ) ;
#6794 = CARTESIAN_POINT ( 'NONE',  ( -1.291648043291917070, 3.499742528936139241, 227.7788113689714464 ) ) ;
#6795 = CARTESIAN_POINT ( 'NONE',  ( -27.30231674030000022, 6.653883447060000123, 222.0000000000000000 ) ) ;
#6796 = CARTESIAN_POINT ( 'NONE',  ( -23.56565371579999990, -14.74874063789999923, 225.5071239680000303 ) ) ;
#6797 = PLANE ( 'NONE',  #18729 ) ;
#6798 = CARTESIAN_POINT ( 'NONE',  ( 7.350552255519282596, -6.527378230651997626, -34.29555409013811129 ) ) ;
#6799 = CARTESIAN_POINT ( 'NONE',  ( -7.999999999884559898, -60.75400889059668685, -3.446705952702470377 ) ) ;
#6800 = ADVANCED_FACE ( 'NONE', ( #30856 ), #1888, .F. ) ;
#6801 = ORIENTED_EDGE ( 'NONE', *, *, #18098, .F. ) ;
#6802 = CARTESIAN_POINT ( 'NONE',  ( -4.240613917342963113, -1.711409762446096439, -59.38491726642499202 ) ) ;
#6803 = CARTESIAN_POINT ( 'NONE',  ( -27.77512470410000134, 4.683313577610000777, 229.2930777930000090 ) ) ;
#6804 = ORIENTED_EDGE ( 'NONE', *, *, #11275, .T. ) ;
#6805 = EDGE_CURVE ( 'NONE', #15932, #15963, #20946, .T. ) ;
#6806 = CARTESIAN_POINT ( 'NONE',  ( 0.000000000000000000, 0.000000000000000000, 190.0000000000000000 ) ) ;
#6807 = CARTESIAN_POINT ( 'NONE',  ( 0.1332961122732720383, -6.531058726825651028, -24.41888333260000365 ) ) ;
#6808 = ORIENTED_EDGE ( 'NONE', *, *, #20808, .T. ) ;
#6809 = EDGE_CURVE ( 'NONE', #10105, #2499, #30550, .T. ) ;
#6810 = CARTESIAN_POINT ( 'NONE',  ( -22.03726251081861065, 17.02871019621900217, 223.6666666666666572 ) ) ;
#6811 = CARTESIAN_POINT ( 'NONE',  ( -2.664535259099999568E-14, -26.80000000000000071, 115.0000000000000000 ) ) ;
#6812 = ORIENTED_EDGE ( 'NONE', *, *, #23979, .F. ) ;
#6813 = ORIENTED_EDGE ( 'NONE', *, *, #20390, .T. ) ;
#6814 = ORIENTED_EDGE ( 'NONE', *, *, #14790, .T. ) ;
#6815 = ORIENTED_EDGE ( 'NONE', *, *, #15252, .T. ) ;
#6816 = DIRECTION ( 'NONE',  ( 1.000000000000000000, -1.843431230200084908E-12, 2.650498504963248473E-12 ) ) ;
#6817 = PRODUCT_DEFINITION_FORMATION_WITH_SPECIFIED_SOURCE ( 'ANY', '', #24741, .NOT_KNOWN. ) ;
#6818 = CARTESIAN_POINT ( 'NONE',  ( 28.45300238704230367, 0.5177135156027677931, 0.5017677510000262409 ) ) ;
#6819 = CARTESIAN_POINT ( 'NONE',  ( -4.185763533044374540, 4.163314928055855901, -68.46322600552500148 ) ) ;
#6820 = CARTESIAN_POINT ( 'NONE',  ( 5.125960221229999725, -30.23021873609999943, 229.9172029869999960 ) ) ;
#6821 = CARTESIAN_POINT ( 'NONE',  ( -18.97090238746602964, 21.26865671882813302, 1.000000000000000888 ) ) ;
#6822 = CARTESIAN_POINT ( 'NONE',  ( -3.423281690950000122, -28.45174682580000081, 222.0000000000000000 ) ) ;
#6823 = CARTESIAN_POINT ( 'NONE',  ( 3.599369630949024845, -3.224860595692283116, -0.6998634107611361177 ) ) ;
#6824 = ORIENTED_EDGE ( 'NONE', *, *, #25923, .T. ) ;
#6825 = CARTESIAN_POINT ( 'NONE',  ( -14.76964124820000102, 19.99999999999999645, -1.399999999299995856 ) ) ;
#6826 = CARTESIAN_POINT ( 'NONE',  ( 3.082386449366550707, -3.056625787687244689, -14.56112212870000810 ) ) ;
#6827 = DIRECTION ( 'NONE',  ( 0.000000000000000000, 0.000000000000000000, 1.000000000000000000 ) ) ;
#6828 = CARTESIAN_POINT ( 'NONE',  ( 8.516764494467457425, -8.915308899531273923, 232.6627636846916403 ) ) ;
#6829 = EDGE_LOOP ( 'NONE', ( #3469, #3015, #517, #6490 ) ) ;
#6830 = CARTESIAN_POINT ( 'NONE',  ( -23.24877830753397490, -15.24265806274975787, 4.710689436884310410 ) ) ;
#6831 = CARTESIAN_POINT ( 'NONE',  ( 1.413941964909729787, -28.46527362969750996, 4.319830470999985295 ) ) ;
#6832 = DIRECTION ( 'NONE',  ( 0.000000000000000000, 0.000000000000000000, 1.000000000000000000 ) ) ;
#6833 = CARTESIAN_POINT ( 'NONE',  ( 1.127732790480000080, -28.47784299079999926, 225.0000014190000002 ) ) ;
#6834 = CARTESIAN_POINT ( 'NONE',  ( 11.20000000009999930, -27.00000000000000000, -28.39999999989999679 ) ) ;
#6835 = CARTESIAN_POINT ( 'NONE',  ( -5.427432314178970429, 2.515719109140460041, -65.77526299442500601 ) ) ;
#6836 = DIRECTION ( 'NONE',  ( -3.924189347185962345E-12, 0.4082287037029530552, 0.9128796883888953273 ) ) ;
#6837 = DIRECTION ( 'NONE',  ( -1.000000000000000000, 0.000000000000000000, 0.000000000000000000 ) ) ;
#6838 = EDGE_LOOP ( 'NONE', ( #27624, #2869, #28249, #29286 ) ) ;
#6839 = CARTESIAN_POINT ( 'NONE',  ( -10.69999999999999929, -24.47788622780000267, -30.04435323410000080 ) ) ;
#6840 = DIRECTION ( 'NONE',  ( -0.7071067811870488384, 0.000000000000000000, 0.7071067811860461960 ) ) ;
#6841 = CARTESIAN_POINT ( 'NONE',  ( 1.909765729747931351, -4.496882425974528807, -68.10000000002501963 ) ) ;
#6842 = EDGE_CURVE ( 'NONE', #14134, #12603, #18579, .T. ) ;
#6843 = CARTESIAN_POINT ( 'NONE',  ( 2.091444806099476583, 2.888061030883168456, -88.52261276238974119 ) ) ;
#6844 = CARTESIAN_POINT ( 'NONE',  ( -4.561137155964747336, 0.9634438910280386237, -44.10000000002499121 ) ) ;
#6845 =( NAMED_UNIT ( * ) PLANE_ANGLE_UNIT ( ) SI_UNIT ( $, .RADIAN. ) );
#6846 = ORIENTED_EDGE ( 'NONE', *, *, #22710, .T. ) ;
#6847 = CARTESIAN_POINT ( 'NONE',  ( -9.999999999969999109, -24.00000000000000000, -28.40000000000000213 ) ) ;
#6848 = CARTESIAN_POINT ( 'NONE',  ( -3.508509149563535434, -4.733412845334678209, -65.93409070562501029 ) ) ;
#6849 = ORIENTED_EDGE ( 'NONE', *, *, #8074, .F. ) ;
#6850 = CARTESIAN_POINT ( 'NONE',  ( 11.08346179031907930, -28.41490585489482257, 186.3944487249999895 ) ) ;
#6851 = CARTESIAN_POINT ( 'NONE',  ( -2.901540723753613715, -2.679228086972462730, -44.22295181582499168 ) ) ;
#6852 = ORIENTED_EDGE ( 'NONE', *, *, #8582, .T. ) ;
#6853 = CARTESIAN_POINT ( 'NONE',  ( -5.240471012809999607, -2.862882362280000148, 226.6412452697800006 ) ) ;
#6854 = DIRECTION ( 'NONE',  ( -1.000000000000000000, 1.662859514859999923E-15, -6.790296706416999781E-12 ) ) ;
#6855 = DIRECTION ( 'NONE',  ( 0.000000000000000000, 0.000000000000000000, -1.000000000000000000 ) ) ;
#6856 = CARTESIAN_POINT ( 'NONE',  ( -10.69999999999999929, -27.00000000000000000, -28.40000000000000213 ) ) ;
#6857 = CARTESIAN_POINT ( 'NONE',  ( -4.041451884379999804, 9.156941871420000667E-11, 230.5235986622430175 ) ) ;
#6858 = DIRECTION ( 'NONE',  ( 1.000000000000000000, -1.634095982650525115E-15, 6.790302532597771964E-12 ) ) ;
#6859 = ORIENTED_EDGE ( 'NONE', *, *, #21955, .F. ) ;
#6860 = CARTESIAN_POINT ( 'NONE',  ( 21.70992212615148986, 18.50697891487987334, 5.000000000000004441 ) ) ;
#6861 = CARTESIAN_POINT ( 'NONE',  ( 24.48837202150000181, -14.58033361329999877, 226.0424736289999714 ) ) ;
#6862 = ADVANCED_FACE ( 'NONE', ( #5183 ), #19047, .T. ) ;
#6863 = CARTESIAN_POINT ( 'NONE',  ( 19.56378028550000181, 19.56885116670000357, 229.4995147189999898 ) ) ;
#6864 = LINE ( 'NONE', #28890, #3714 ) ;
#6865 = CARTESIAN_POINT ( 'NONE',  ( -12.39529267485836428, -30.57814011873969307, -32.10766253134598003 ) ) ;
#6866 = CARTESIAN_POINT ( 'NONE',  ( 11.08631338020000001, 4.914038141549999850, 230.6412452697800006 ) ) ;
#6867 = DIRECTION ( 'NONE',  ( -1.000000000000000000, 1.467383017310000131E-15, -6.771000000000000128E-12 ) ) ;
#6868 = DIRECTION ( 'NONE',  ( 0.7198537139083028835, -0.6941258031311204890, 0.000000000000000000 ) ) ;
#6869 = CARTESIAN_POINT ( 'NONE',  ( 2.990129296507525680, -3.859048371143013245, -51.75430438132499944 ) ) ;
#6870 = CARTESIAN_POINT ( 'NONE',  ( 4.175165894169885483, -50.49316738903675628, -44.10000000000000142 ) ) ;
#6871 = CARTESIAN_POINT ( 'NONE',  ( -26.94142135619999934, -1.740902259209999758E-13, 230.0000000000000000 ) ) ;
#6872 = CARTESIAN_POINT ( 'NONE',  ( 2.385041915132713353, -2.868471282680012724, 230.7036791710386296 ) ) ;
#6873 = ORIENTED_EDGE ( 'NONE', *, *, #27097, .T. ) ;
#6874 = LINE ( 'NONE', #11761, #17764 ) ;
#6875 = CARTESIAN_POINT ( 'NONE',  ( -24.15901410609999900, -15.12012600329999934, 224.4928788709999878 ) ) ;
#6876 = CARTESIAN_POINT ( 'NONE',  ( -3.221934060409654688, 3.671197199744478112, -54.38587006832499071 ) ) ;
#6877 = ORIENTED_EDGE ( 'NONE', *, *, #20808, .F. ) ;
#6878 = ITEM_DEFINED_TRANSFORMATION ( 'NONE', 'NONE', #19377,  #17722 ) ;
#6879 = EDGE_LOOP ( 'NONE', ( #6147, #20671, #13740, #28139 ) ) ;
#6880 = CARTESIAN_POINT ( 'NONE',  ( -17.47798013194552524, -29.94181156654346054, -32.47511133710052889 ) ) ;
#6881 = VERTEX_POINT ( 'NONE', #31009 ) ;
#6882 = CARTESIAN_POINT ( 'NONE',  ( -8.699999999977865883, -116.4387282385435185, 10.14683980286297604 ) ) ;
#6883 = CARTESIAN_POINT ( 'NONE',  ( 4.680451711962687611, -10.51223169637473376, -35.68981701567106768 ) ) ;
#6884 = CARTESIAN_POINT ( 'NONE',  ( 8.999999999540001738, -130.0000000000000000, -43.75000000008299850 ) ) ;
#6885 = EDGE_CURVE ( 'NONE', #19970, #16882, #16993, .T. ) ;
#6886 = AXIS2_PLACEMENT_3D ( 'NONE', #12318, #17344, #7129 ) ;
#6887 = ORIENTED_EDGE ( 'NONE', *, *, #1804, .F. ) ;
#6888 = CIRCLE ( 'NONE', #27484, 4.000000000000000888 ) ;
#6889 = CARTESIAN_POINT ( 'NONE',  ( 14.85000000009999788, -24.60407027184000128, -24.01428005041999825 ) ) ;
#6890 = DIRECTION ( 'NONE',  ( 1.000000000000000000, 0.000000000000000000, 0.000000000000000000 ) ) ;
#6891 = FACE_OUTER_BOUND ( 'NONE', #10836, .T. ) ;
#6892 = CARTESIAN_POINT ( 'NONE',  ( -1.831588579526983063, 3.958388136463033558, -7.231725184300001885 ) ) ;
#6893 = ADVANCED_BREP_SHAPE_REPRESENTATION ( '', ( #11447, #17722 ), #22285 ) ;
#6894 = CARTESIAN_POINT ( 'NONE',  ( 5.275462242469999730, -31.11186713239999690, 230.2432540810000319 ) ) ;
#6895 = VERTEX_POINT ( 'NONE', #14796 ) ;
#6896 = CARTESIAN_POINT ( 'NONE',  ( -2.249420116617089072, -4.577155045439369019, -44.10000000002499121 ) ) ;
#6897 = ADVANCED_FACE ( 'NONE', ( #28645 ), #19518, .F. ) ;
#6898 = CARTESIAN_POINT ( 'NONE',  ( -2.402234890526806499, 4.289919416549723863, -17.61511783619999960 ) ) ;
#6899 = CARTESIAN_POINT ( 'NONE',  ( 26.99674179536344099, 9.610833985112126499, 8.000000000000007105 ) ) ;
#6900 = CARTESIAN_POINT ( 'NONE',  ( -10.02421345359999982, -25.00000000000000000, -2.058579360600006236 ) ) ;
#6901 = B_SPLINE_CURVE_WITH_KNOTS ( 'NONE', 5,
 ( #22935, #3410, #8280, #20246, #29846, #25614 ),
 .UNSPECIFIED., .F., .F.,
 ( 6, 6 ),
 ( -2.300779717370000199, 0.000000000000000000 ),
 .UNSPECIFIED. ) ;
#6902 = CARTESIAN_POINT ( 'NONE',  ( 22.83564165258658818, -19.45716463537533159, -0.6999999999999784173 ) ) ;
#6903 = CARTESIAN_POINT ( 'NONE',  ( 0.2462945485190000117, -28.49939181899999951, 223.9202078600000050 ) ) ;
#6904 = CARTESIAN_POINT ( 'NONE',  ( 22.41293933140000050, 16.47772227400000489, 222.9999999789999947 ) ) ;
#6905 = FACE_OUTER_BOUND ( 'NONE', #20955, .T. ) ;
#6906 = CARTESIAN_POINT ( 'NONE',  ( 10.49791847189999849, 19.99999999999999645, -3.602081527999998034 ) ) ;
#6907 = AXIS2_PLACEMENT_3D ( 'NONE', #16184, #21074, #16341 ) ;
#6908 = CARTESIAN_POINT ( 'NONE',  ( 3.227294851203073023, -1.430228209132706318, 226.6412452697750268 ) ) ;
#6909 = CARTESIAN_POINT ( 'NONE',  ( 0.4713258872182368164, -27.79624559782057602, 3.899998581000013509 ) ) ;
#6910 = EDGE_CURVE ( 'NONE', #14792, #12633, #7794, .T. ) ;
#6911 = AXIS2_PLACEMENT_3D ( 'NONE', #23090, #1837, #30318 ) ;
#6912 = EDGE_CURVE ( 'NONE', #25637, #10339, #18062, .T. ) ;
#6913 = CARTESIAN_POINT ( 'NONE',  ( -9.707106781189999367, 19.99999999999999645, -43.10710678118599759 ) ) ;
#6914 = VERTEX_POINT ( 'NONE', #14177 ) ;
#6915 = AXIS2_PLACEMENT_3D ( 'NONE', #7197, #12381, #21989 ) ;
#6916 = CARTESIAN_POINT ( 'NONE',  ( -11.25000838610000109, 19.99999999999999645, -0.7501799203000064642 ) ) ;
#6917 = SURFACE_STYLE_USAGE ( .BOTH. , #25972 ) ;
#6918 = VECTOR ( 'NONE', #29412, 1000.000000000000000 ) ;
#6919 = DIRECTION ( 'NONE',  ( -0.9690327085533227969, -0.2219413702013694756, 0.1082480389981703706 ) ) ;
#6920 = ORIENTED_EDGE ( 'NONE', *, *, #13369, .F. ) ;
#6921 = CARTESIAN_POINT ( 'NONE',  ( -3.130203125555106158, 5.106303518385050033, -45.53531229042499717 ) ) ;
#6922 = VERTEX_POINT ( 'NONE', #9604 ) ;
#6923 = ORIENTED_EDGE ( 'NONE', *, *, #18957, .T. ) ;
#6924 = PRODUCT_RELATED_PRODUCT_CATEGORY ( 'part', '', ( #9142 ) ) ;
#6925 = DIRECTION ( 'NONE',  ( 1.000000000000000000, 0.000000000000000000, 0.000000000000000000 ) ) ;
#6926 = ORIENTED_EDGE ( 'NONE', *, *, #29953, .T. ) ;
#6927 = CARTESIAN_POINT ( 'NONE',  ( 11.69999999989999928, -24.11120071670000087, -0.6999999999999992895 ) ) ;
#6928 = ORIENTED_EDGE ( 'NONE', *, *, #29196, .T. ) ;
#6929 = CARTESIAN_POINT ( 'NONE',  ( -25.14597776469910428, -15.02549348198344603, 1.000000000000000888 ) ) ;
#6930 = CARTESIAN_POINT ( 'NONE',  ( 23.62421573330318836, 14.65442405561991634, 3.957526369000014199 ) ) ;
#6931 = DIRECTION ( 'NONE',  ( 1.000000000000000000, -1.224606353819999829E-16, 0.000000000000000000 ) ) ;
#6932 = CARTESIAN_POINT ( 'NONE',  ( 0.1986510695968027040, 4.503440677479858323, -35.69999999999999574 ) ) ;
#6933 = CIRCLE ( 'NONE', #2431, 27.92857142840000151 ) ;
#6934 = B_SPLINE_CURVE_WITH_KNOTS ( 'NONE', 3,
 ( #23820, #12460, #24271, #4778, #9802, #16874 ),
 .UNSPECIFIED., .F., .F.,
 ( 4, 2, 4 ),
 ( 0.000000000000000000, 0.5000000000000000000, 1.000000000000000000 ),
 .UNSPECIFIED. ) ;
#6935 = SHAPE_REPRESENTATION ( 'Release Lever', ( #17722 ), #2296 ) ;
#6936 = DIRECTION ( 'NONE',  ( 6.326189572192215265E-12, 0.3568421334038983650, -0.9341647027306021478 ) ) ;
#6937 = EDGE_CURVE ( 'NONE', #19859, #25327, #27302, .T. ) ;
#6938 = CYLINDRICAL_SURFACE ( 'NONE', #22986, 3.000000000000003997 ) ;
#6939 = CARTESIAN_POINT ( 'NONE',  ( -22.63992238019999803, -14.34133587289999845, 5.000000000000000000 ) ) ;
#6940 = CARTESIAN_POINT ( 'NONE',  ( 1.484924240490000047, -1.484924240490000047, 226.6412452697800006 ) ) ;
#6941 = ORIENTED_EDGE ( 'NONE', *, *, #16694, .T. ) ;
#6942 = TOROIDAL_SURFACE ( 'NONE', #26051, 24.50000000000000000, 3.200000000000000178 ) ;
#6943 = CARTESIAN_POINT ( 'NONE',  ( -6.505526340832360255, -0.4164809035307331930, -4.748838774899996729 ) ) ;
#6944 = CARTESIAN_POINT ( 'NONE',  ( 6.487627055914963137, 0.6495842397260740420, -29.03116556699999862 ) ) ;
#6945 = CYLINDRICAL_SURFACE ( 'NONE', #14293, 26.80000000000002203 ) ;
#6946 = AXIS2_PLACEMENT_3D ( 'NONE', #9759, #12116, #16842 ) ;
#6947 = CARTESIAN_POINT ( 'NONE',  ( -3.458129700886692248, 0.5397582531516398330, -88.52261276316077954 ) ) ;
#6948 = CARTESIAN_POINT ( 'NONE',  ( 0.9263908148288600986, 3.499834818475870968, 227.7157682482504413 ) ) ;
#6949 = CARTESIAN_POINT ( 'NONE',  ( -25.26019820782813596, 13.19871658270252723, 5.889015029569602433 ) ) ;
#6950 = CARTESIAN_POINT ( 'NONE',  ( -0.7873752056533345201, -4.273814420472608511, -3.525234013000005717 ) ) ;
#6951 = ADVANCED_FACE ( 'NONE', ( #24396 ), #14646, .F. ) ;
#6952 = PRODUCT_DEFINITION_SHAPE ( 'NONE', 'NONE',  #31137 ) ;
#6953 = CARTESIAN_POINT ( 'NONE',  ( 18.13191322229999969, 10.47263190749999495, -1.399999999599998990 ) ) ;
#6954 = APPLICATION_CONTEXT ( 'automotive_design' ) ;
#6955 = CARTESIAN_POINT ( 'NONE',  ( 1.311146135488785669, -27.76947565999227763, 5.759639119000015128 ) ) ;
#6956 = CARTESIAN_POINT ( 'NONE',  ( -18.93860194420127030, -19.09088854112969003, -1.399999999999998579 ) ) ;
#6957 = ORIENTED_EDGE ( 'NONE', *, *, #29494, .F. ) ;
#6958 = CARTESIAN_POINT ( 'NONE',  ( -24.81746041937532965, 14.01353061208509310, 6.079865099000020479 ) ) ;
#6959 = AXIS2_PLACEMENT_3D ( 'NONE', #14805, #29419, #22349 ) ;
#6960 = ORIENTED_EDGE ( 'NONE', *, *, #8269, .F. ) ;
#6961 = CARTESIAN_POINT ( 'NONE',  ( 4.638687372183706970, -17.80543024189401535, -28.79488058871456957 ) ) ;
#6962 = CARTESIAN_POINT ( 'NONE',  ( -6.074876045044606876, 0.8789665559579967757, -34.25783976329999092 ) ) ;
#6963 = ORIENTED_EDGE ( 'NONE', *, *, #6110, .T. ) ;
#6964 = EDGE_CURVE ( 'NONE', #24321, #11773, #5012, .T. ) ;
#6965 = CARTESIAN_POINT ( 'NONE',  ( 23.24663841809999809, -14.69162354060000020, 5.000000000000000000 ) ) ;
#6966 = CARTESIAN_POINT ( 'NONE',  ( 22.36196472700000015, 17.71394650440000262, 223.9999999570000000 ) ) ;
#6967 = ORIENTED_EDGE ( 'NONE', *, *, #24708, .F. ) ;
#6968 = CIRCLE ( 'NONE', #3954, 26.80000000000000071 ) ;
#6969 = PRODUCT_RELATED_PRODUCT_CATEGORY ( 'part', '', ( #24741 ) ) ;
#6970 = VERTEX_POINT ( 'NONE', #21575 ) ;
#6971 = ORIENTED_EDGE ( 'NONE', *, *, #437, .T. ) ;
#6972 =( NAMED_UNIT ( * ) PLANE_ANGLE_UNIT ( ) SI_UNIT ( $, .RADIAN. ) );
#6973 = B_SPLINE_CURVE_WITH_KNOTS ( 'NONE', 3,
 ( #962, #3452, #24565, #22201 ),
 .UNSPECIFIED., .F., .F.,
 ( 4, 4 ),
 ( 0.000000000000000000, 1.000000000000000000 ),
 .UNSPECIFIED. ) ;
#6974 = ORIENTED_EDGE ( 'NONE', *, *, #26867, .F. ) ;
#6976 = CARTESIAN_POINT ( 'NONE',  ( -17.49999999969999109, -23.99999999999999289, -28.79800326595887583 ) ) ;
#6975 = B_SPLINE_CURVE_WITH_KNOTS ( 'NONE', 5,
 ( #1699, #6719, #10985, #23427, #16323, #21054, #3740, #6565, #30803 ),
 .UNSPECIFIED., .F., .F.,
 ( 6, 3, 6 ),
 ( 0.000000000000000000, 1.472643963329999917, 1.642768356779999994 ),
 .UNSPECIFIED. ) ;
#6977 = CARTESIAN_POINT ( 'NONE',  ( -14.90000000006999947, -24.00000000000000000, -28.40000000020000215 ) ) ;
#6978 = CARTESIAN_POINT ( 'NONE',  ( 0.2632024292269652954, 4.191744801550177257, -68.60875473022500159 ) ) ;
#6979 = VERTEX_POINT ( 'NONE', #12272 ) ;
#6980 = DIRECTION ( 'NONE',  ( 1.000000000000000000, -1.634095982650525115E-15, 6.790302532597771964E-12 ) ) ;
#6981 = EDGE_CURVE ( 'NONE', #18020, #18294, #26135, .T. ) ;
#6982 = CARTESIAN_POINT ( 'NONE',  ( 14.99213822049999933, -23.71131899119999886, 222.0000000000000000 ) ) ;
#6983 = CARTESIAN_POINT ( 'NONE',  ( 3.556182480049746353, -3.295754068138798676, -0.6998097270557633864 ) ) ;
#6984 = ORIENTED_EDGE ( 'NONE', *, *, #19106, .T. ) ;
#6985 = CARTESIAN_POINT ( 'NONE',  ( -20.19477874851248700, 20.00033066885824695, 0.4884133666381245131 ) ) ;
#6986 = VECTOR ( 'NONE', #27795, 1000.000000000000000 ) ;
#6987 = ADVANCED_FACE ( 'NONE', ( #11814 ), #16199, .F. ) ;
#6988 = CARTESIAN_POINT ( 'NONE',  ( -4.363437395929424589, 0.1294788321584636748, -12.68304957890000217 ) ) ;
#6989 = CARTESIAN_POINT ( 'NONE',  ( 8.699999999528305494, -25.92947359976189503, -31.20249410819006286 ) ) ;
#6990 = CARTESIAN_POINT ( 'NONE',  ( -3.441895295100000141, -11.73074823080000151, 232.6627637660000119 ) ) ;
#6991 = ORIENTED_EDGE ( 'NONE', *, *, #11036, .T. ) ;
#6992 = CARTESIAN_POINT ( 'NONE',  ( 25.87491792499379883, 7.311113148304238862, -1.399999999999998579 ) ) ;
#6993 = CARTESIAN_POINT ( 'NONE',  ( -10.69999999989999928, -25.00000000000000000, -16.71944709739999979 ) ) ;
#6994 = CARTESIAN_POINT ( 'NONE',  ( -26.28649255380000227, 11.41136534319999996, 222.0000000000000000 ) ) ;
#6995 = EDGE_CURVE ( 'NONE', #30810, #17596, #10539, .T. ) ;
#6996 = CARTESIAN_POINT ( 'NONE',  ( -12.77820031340000106, 20.99999999999999645, -56.10000000020000499 ) ) ;
#6997 = CARTESIAN_POINT ( 'NONE',  ( -5.296314592117303377, -2.692763687817543161, -62.36424626872499033 ) ) ;
#6998 = AXIS2_PLACEMENT_3D ( 'NONE', #14893, #15045, #17393 ) ;
#6999 = DIRECTION ( 'NONE',  ( 0.2815395311429195746, 0.9595496299847261490, 0.000000000000000000 ) ) ;
#7000 = DIRECTION ( 'NONE',  ( 0.000000000000000000, 0.000000000000000000, 1.000000000000000000 ) ) ;
#7001 = EDGE_LOOP ( 'NONE', ( #8950, #13032, #29758, #637, #9992, #4843, #28422, #15870, #863, #20586 ) ) ;
#7002 = DIRECTION ( 'NONE',  ( 0.000000000000000000, 1.000000000000000000, 0.000000000000000000 ) ) ;
#7003 = CARTESIAN_POINT ( 'NONE',  ( 16.40303402077768169, -9.791839085275103827, -0.6999999999999784173 ) ) ;
#7004 = CARTESIAN_POINT ( 'NONE',  ( 1.237533978107217214, -4.800969678198779178, -68.10000000002500542 ) ) ;
#7005 = CARTESIAN_POINT ( 'NONE',  ( -4.876949263959866165, -0.8560970368912672601, -68.10000000002500542 ) ) ;
#7006 = CARTESIAN_POINT ( 'NONE',  ( -2.127246859535990353, 2.914123423714512384, -88.52261276242110455 ) ) ;
#7007 = CARTESIAN_POINT ( 'NONE',  ( -4.887447097588012213, -0.7107402505946681659, -44.10000000002498410 ) ) ;
#7008 = SURFACE_SIDE_STYLE ('',( #14406 ) ) ;
#7009 = EDGE_LOOP ( 'NONE', ( #21809, #19618 ) ) ;
#7010 = CARTESIAN_POINT ( 'NONE',  ( 11.50378924416101256, 21.69999999997430606, -55.48383121567042764 ) ) ;
#7011 = CARTESIAN_POINT ( 'NONE',  ( 1.592882851206511186, -27.75460863273100998, 4.791883387999989807 ) ) ;
#7012 = ORIENTED_EDGE ( 'NONE', *, *, #24795, .F. ) ;
#7013 = CARTESIAN_POINT ( 'NONE',  ( 24.78575720336396415, -12.59082710992283793, 4.503870356536896047 ) ) ;
#7014 = CIRCLE ( 'NONE', #26602, 0.2500000000000002220 ) ;
#7015 = CARTESIAN_POINT ( 'NONE',  ( 2.534862810676351330, -4.171999357468124003, -46.56669147672499065 ) ) ;
#7016 = EDGE_CURVE ( 'NONE', #5895, #9494, #6295, .T. ) ;
#7017 = ORIENTED_EDGE ( 'NONE', *, *, #7191, .T. ) ;
#7018 = DIRECTION ( 'NONE',  ( 0.000000000000000000, 0.000000000000000000, 1.000000000000000000 ) ) ;
#7019 = CARTESIAN_POINT ( 'NONE',  ( -19.80535357367646654, 19.50875577052770993, 2.600000086000031629 ) ) ;
#7020 = CARTESIAN_POINT ( 'NONE',  ( -0.5575288593901739365, -27.79459983365126163, 4.689815098000011062 ) ) ;
#7021 = EDGE_CURVE ( 'NONE', #2527, #6895, #9028, .T. ) ;
#7022 = CARTESIAN_POINT ( 'NONE',  ( -10.69999999994971240, -29.61921542333507773, -20.12109567583046399 ) ) ;
#7023 = EDGE_CURVE ( 'NONE', #28644, #1470, #25080, .T. ) ;
#7024 = DIRECTION ( 'NONE',  ( -0.9880370573969197157, 0.1542166437529879364, 0.000000000000000000 ) ) ;
#7025 = VERTEX_POINT ( 'NONE', #15102 ) ;
#7026 = DIRECTION ( 'NONE',  ( 1.000000000000000000, 0.000000000000000000, 0.000000000000000000 ) ) ;
#7027 = CARTESIAN_POINT ( 'NONE',  ( 24.68173674080000168, -14.25001227039999918, 226.1000014189999945 ) ) ;
#7028 = CARTESIAN_POINT ( 'NONE',  ( 18.03079990150000000, 20.00000068800000008, 230.7000122960000112 ) ) ;
#7029 = CARTESIAN_POINT ( 'NONE',  ( -19.80526803560000104, 19.50877411520000138, 222.0000000000000000 ) ) ;
#7030 = CARTESIAN_POINT ( 'NONE',  ( 8.700000000232158470, -29.34712076613124410, -26.49064271397861603 ) ) ;
#7031 = CARTESIAN_POINT ( 'NONE',  ( -0.07056952541309999272, -28.50017087330000010, 226.0986539140000104 ) ) ;
#7032 = LINE ( 'NONE', #25655, #26775 ) ;
#7033 = CARTESIAN_POINT ( 'NONE',  ( -24.82162973577332465, 12.51998933601907993, 4.689351480999998323 ) ) ;
#7034 = CARTESIAN_POINT ( 'NONE',  ( 24.07552309629999954, -13.90001137829999855, 226.1000014189999945 ) ) ;
#7035 = CARTESIAN_POINT ( 'NONE',  ( 5.363076718300177959, -2.525690298526013677, -51.81872167392499762 ) ) ;
#7036 = CARTESIAN_POINT ( 'NONE',  ( 12.09920926763414073, -0.2766206855562842737, 232.0000002394077967 ) ) ;
#7037 = CARTESIAN_POINT ( 'NONE',  ( -27.09307779339999911, -1.459363161060000088E-12, 229.9751247039999953 ) ) ;
#7038 = CARTESIAN_POINT ( 'NONE',  ( 24.47278418934494937, 14.60601539438439822, 6.095965388000001539 ) ) ;
#7039 = ORIENTED_EDGE ( 'NONE', *, *, #16041, .T. ) ;
#7040 = CARTESIAN_POINT ( 'NONE',  ( 20.30396079662882158, 20.00000000004802203, 1.800000000000023803 ) ) ;
#7041 = VERTEX_POINT ( 'NONE', #22183 ) ;
#7042 = CARTESIAN_POINT ( 'NONE',  ( -24.68204616399999907, -14.25020164319999871, 223.9000014189999774 ) ) ;
#7043 = CARTESIAN_POINT ( 'NONE',  ( 4.003591150705129387, -2.204345408526039218, -58.30843849682500490 ) ) ;
#7044 = ORIENTED_EDGE ( 'NONE', *, *, #7866, .F. ) ;
#7045 = EDGE_CURVE ( 'NONE', #13976, #6970, #1460, .T. ) ;
#7046 = ORIENTED_EDGE ( 'NONE', *, *, #15676, .F. ) ;
#7047 = VECTOR ( 'NONE', #27061, 1000.000000000000114 ) ;
#7048 = DIRECTION ( 'NONE',  ( 4.428977494234582379E-12, 0.8987940462991651502, -0.4383711467890810676 ) ) ;
#7049 = EDGE_LOOP ( 'NONE', ( #15438, #3661 ) ) ;
#7050 = CARTESIAN_POINT ( 'NONE',  ( 25.90432029460000152, 13.09158661030000026, 229.0000000000000000 ) ) ;
#7051 = CARTESIAN_POINT ( 'NONE',  ( -8.699999999628362346, -14.95623164695839513, -40.37561726986208299 ) ) ;
#7052 = CARTESIAN_POINT ( 'NONE',  ( -8.699999999662093586, -15.94902145834643115, -35.53273252493492862 ) ) ;
#7053 = CARTESIAN_POINT ( 'NONE',  ( -22.36167894509999954, 17.71395549689999882, 224.0000000000000000 ) ) ;
#7054 = CARTESIAN_POINT ( 'NONE',  ( -1.092383471258445704, -3.930924299782534437, -38.89973510835866222 ) ) ;
#7055 = CARTESIAN_POINT ( 'NONE',  ( -6.999999999888483870, -60.34578018689466461, -2.533826264308865817 ) ) ;
#7056 = CARTESIAN_POINT ( 'NONE',  ( 5.214500487626152037, -1.910846663805727541, -4.836105321700002513 ) ) ;
#7057 = CARTESIAN_POINT ( 'NONE',  ( -28.04325408110000240, 1.065814103639999922E-14, 230.2432540810000319 ) ) ;
#7058 = ORIENTED_EDGE ( 'NONE', *, *, #12156, .T. ) ;
#7059 = DIRECTION ( 'NONE',  ( 1.000000000000000000, 0.000000000000000000, 0.000000000000000000 ) ) ;
#7060 = CIRCLE ( 'NONE', #46, 2.926829268290000119 ) ;
#7061 = CARTESIAN_POINT ( 'NONE',  ( 3.244870203142138809, 3.966006825147196047, -21.19372222230000347 ) ) ;
#7062 = CARTESIAN_POINT ( 'NONE',  ( -11.50000000044500048, -23.79999999999999716, -28.40000000000541647 ) ) ;
#7063 = CARTESIAN_POINT ( 'NONE',  ( -9.999999999909999104, -25.00000000000000000, -2.399999999999999467 ) ) ;
#7064 = CARTESIAN_POINT ( 'NONE',  ( -1.027511273769999933E-13, -27.50000000000000000, 230.0000000000000000 ) ) ;
#7065 = CARTESIAN_POINT ( 'NONE',  ( 22.97596755210000197, 15.65128466780000061, 222.0000000000000000 ) ) ;
#7066 = CARTESIAN_POINT ( 'NONE',  ( -1.877135327876712667, -5.132840123261955156, -43.18640794712499797 ) ) ;
#7067 = VECTOR ( 'NONE', #4422, 1000.000000000000000 ) ;
#7068 = B_SPLINE_CURVE_WITH_KNOTS ( 'NONE', 3,
 ( #21141, #28213, #4463, #8696, #15791, #4149, #14063, #1797, #11388, #13744, #30736, #30436, #13590, #30898, #28059, #20986, #11076, #18615 ),
 .UNSPECIFIED., .F., .F.,
 ( 4, 2, 2, 2, 2, 2, 2, 2, 4 ),
 ( 0.000000000000000000, 0.1250000000000003053, 0.2500000000000006106, 0.3750000000000001665, 0.5000000000000002220, 0.6250000000000002220, 0.7500000000000001110, 0.8750000000000001110, 1.000000000000000000 ),
 .UNSPECIFIED. ) ;
#7069 = CYLINDRICAL_SURFACE ( 'NONE', #28788, 2.500000000000002220 ) ;
#7070 = DIRECTION ( 'NONE',  ( -6.325958275728752229E-12, -0.3568421334038983650, 0.9341647027306021478 ) ) ;
#7071 = CARTESIAN_POINT ( 'NONE',  ( -4.260936785125032600, -20.77695744284302037, -30.68337575642739168 ) ) ;
#7072 = EDGE_CURVE ( 'NONE', #31008, #30761, #14558, .T. ) ;
#7073 = EDGE_CURVE ( 'NONE', #15474, #20783, #12731, .T. ) ;
#7074 = CARTESIAN_POINT ( 'NONE',  ( -27.23548387100000312, 3.552713678799999608E-15, 38.33953982530000104 ) ) ;
#7075 = VERTEX_POINT ( 'NONE', #18183 ) ;
#7076 = DIRECTION ( 'NONE',  ( 4.429038154748118518E-12, 0.8987940462991653723, -0.4383711467890809010 ) ) ;
#7077 = CARTESIAN_POINT ( 'NONE',  ( 8.700000000244115128, -26.99999999999395328, -28.39999999994493862 ) ) ;
#7078 = CARTESIAN_POINT ( 'NONE',  ( -7.999999999650399651, -14.92320859811129097, -37.81428931786641812 ) ) ;
#7079 = ORIENTED_EDGE ( 'NONE', *, *, #30030, .F. ) ;
#7080 = CARTESIAN_POINT ( 'NONE',  ( -18.95046173579999760, -18.95046173579999760, 186.7828584120000244 ) ) ;
#7081 = CARTESIAN_POINT ( 'NONE',  ( -6.340437944841875506, 0.6332316896323284539, -47.62737393802499497 ) ) ;
#7082 = ORIENTED_EDGE ( 'NONE', *, *, #21478, .T. ) ;
#7083 = EDGE_CURVE ( 'NONE', #7041, #24435, #29567, .T. ) ;
#7084 = ORIENTED_EDGE ( 'NONE', *, *, #15610, .F. ) ;
#7085 = CARTESIAN_POINT ( 'NONE',  ( 0.000000000000000000, 0.000000000000000000, 0.000000000000000000 ) ) ;
#7086 = CIRCLE ( 'NONE', #26668, 3.200000000000001510 ) ;
#7087 = ORIENTED_EDGE ( 'NONE', *, *, #2738, .F. ) ;
#7088 = CARTESIAN_POINT ( 'NONE',  ( -17.43456092915394251, -9.925215865042019914, 0.000000000000000000 ) ) ;
#7089 = ORIENTED_EDGE ( 'NONE', *, *, #1516, .F. ) ;
#7090 = CARTESIAN_POINT ( 'NONE',  ( 23.51325844009999955, -14.83130343779999905, 225.2083717279999746 ) ) ;
#7091 = CARTESIAN_POINT ( 'NONE',  ( 2.100000000000000089, -1.998401444330000344E-15, 227.6412452697800006 ) ) ;
#7092 = CARTESIAN_POINT ( 'NONE',  ( 5.023648568059999597, 17.12171681569999748, 230.7531949689999919 ) ) ;
#7093 = CARTESIAN_POINT ( 'NONE',  ( 0.7856409681604972217, 4.723271593470196095, -35.69999999999999574 ) ) ;
#7094 = CARTESIAN_POINT ( 'NONE',  ( 18.49564307673682961, 20.00004823712628266, -0.6418581041093734951 ) ) ;
#7095 = DIRECTION ( 'NONE',  ( 1.000000000000000000, 0.000000000000000000, 0.000000000000000000 ) ) ;
#7096 = FACE_OUTER_BOUND ( 'NONE', #25011, .T. ) ;
#7097 = CARTESIAN_POINT ( 'NONE',  ( -19.56389390649999882, 19.56881929660000097, 229.4993219170000032 ) ) ;
#7098 = ADVANCED_FACE ( 'NONE', ( #5648 ), #19829, .T. ) ;
#7099 = B_SPLINE_CURVE_WITH_KNOTS ( 'NONE', 3,
 ( #6661, #8703, #20517, #18310, #11083, #18145 ),
 .UNSPECIFIED., .F., .F.,
 ( 4, 2, 4 ),
 ( 0.000000000000000000, 0.5000000000000000000, 1.000000000000000000 ),
 .UNSPECIFIED. ) ;
#7100 = ORIENTED_EDGE ( 'NONE', *, *, #23883, .F. ) ;
#7101 = CARTESIAN_POINT ( 'NONE',  ( -5.111484982110231279, -0.3272349956394805526, -5.086338774899995308 ) ) ;
#7102 = CARTESIAN_POINT ( 'NONE',  ( 3.430850994441077439, -5.010772104901466406, -26.53292313650000622 ) ) ;
#7103 = DIRECTION ( 'NONE',  ( -1.000000000000000000, 0.000000000000000000, 0.000000000000000000 ) ) ;
#7104 = EDGE_CURVE ( 'NONE', #7731, #11038, #13786, .T. ) ;
#7105 = CARTESIAN_POINT ( 'NONE',  ( 23.48238834476582326, -12.91648733588402820, 225.9606284813543482 ) ) ;
#7106 = DIRECTION ( 'NONE',  ( 0.000000000000000000, -1.000000000000000000, 0.000000000000000000 ) ) ;
#7107 = CARTESIAN_POINT ( 'NONE',  ( 12.94794535341399389, 25.03405588217355415, -59.76667836488295649 ) ) ;
#7108 = CARTESIAN_POINT ( 'NONE',  ( -1.295942751353772238, 4.166547562507297187, -4.774955258300003891 ) ) ;
#7109 = CIRCLE ( 'NONE', #7596, 2.000000000000000000 ) ;
#7110 = CARTESIAN_POINT ( 'NONE',  ( 1.100000000000000089, -27.47799119230000287, 5.000000000000000000 ) ) ;
#7111 = DIRECTION ( 'NONE',  ( 0.000000000000000000, 0.000000000000000000, -1.000000000000000000 ) ) ;
#7112 = CARTESIAN_POINT ( 'NONE',  ( -2.020725942269999909, -3.500000000000000000, 230.5235986622430175 ) ) ;
#7113 = EDGE_LOOP ( 'NONE', ( #27133, #2821, #5732, #20429 ) ) ;
#7114 = CARTESIAN_POINT ( 'NONE',  ( 8.700000000276082446, -16.84110654130126150, -33.19737377701691372 ) ) ;
#7115 = CARTESIAN_POINT ( 'NONE',  ( -6.202057249109299342, 1.908294659314309305, -22.32289663399999924 ) ) ;
#7116 = ORIENTED_EDGE ( 'NONE', *, *, #26922, .F. ) ;
#7117 = CARTESIAN_POINT ( 'NONE',  ( 23.32129337752340348, -14.57293380313067388, 5.556164354324400811 ) ) ;
#7118 = CARTESIAN_POINT ( 'NONE',  ( 23.82471740507292068, 15.64077205896351508, 4.791628269000009155 ) ) ;
#7119 = ORIENTED_EDGE ( 'NONE', *, *, #19079, .T. ) ;
#7120 = ORIENTED_EDGE ( 'NONE', *, *, #25464, .T. ) ;
#7121 = EDGE_CURVE ( 'NONE', #19036, #2003, #16049, .T. ) ;
#7122 = ORIENTED_EDGE ( 'NONE', *, *, #15437, .T. ) ;
#7123 = B_SPLINE_CURVE_WITH_KNOTS ( 'NONE', 1,
 ( #16105, #1799 ),
 .UNSPECIFIED., .F., .F.,
 ( 2, 2 ),
 ( 1.257340418068942224E-07, 0.7036780443879999680 ),
 .UNSPECIFIED. ) ;
#7124 = VERTEX_POINT ( 'NONE', #31090 ) ;
#7125 = DIRECTION ( 'NONE',  ( 0.7071067811865475727, 1.595945597898661921E-12, 0.7071067811865475727 ) ) ;
#7126 = DIRECTION ( 'NONE',  ( -0.9316362575375349842, 0.3633921898465292122, -0.000000000000000000 ) ) ;
#7127 = CARTESIAN_POINT ( 'NONE',  ( -7.999999999718669486, -5.981227587262960554, -27.94042817487965991 ) ) ;
#7128 = ORIENTED_EDGE ( 'NONE', *, *, #14968, .F. ) ;
#7129 = DIRECTION ( 'NONE',  ( -0.7071067811865466846, 1.595945597898659700E-12, 0.7071067811865484609 ) ) ;
#7130 = VECTOR ( 'NONE', #28397, 1000.000000000000114 ) ;
#7131 = LINE ( 'NONE', #14534, #6108 ) ;
#7132 = CARTESIAN_POINT ( 'NONE',  ( -11.50000000000000000, 21.72305290929948640, -60.97178489257708378 ) ) ;
#7133 = EDGE_CURVE ( 'NONE', #20466, #8872, #21102, .T. ) ;
#7134 = VECTOR ( 'NONE', #14910, 1000.000000000000000 ) ;
#7135 = CARTESIAN_POINT ( 'NONE',  ( 3.550686850769999806E-05, -28.50022181210000127, 226.1000014189999945 ) ) ;
#7136 = ORIENTED_EDGE ( 'NONE', *, *, #27076, .T. ) ;
#7137 = CARTESIAN_POINT ( 'NONE',  ( 10.49243769669999971, -24.66097101770000322, -1.192453590699998900 ) ) ;
#7138 = EDGE_CURVE ( 'NONE', #27710, #18256, #23708, .T. ) ;
#7139 = CARTESIAN_POINT ( 'NONE',  ( 3.292208284841127597, -3.106818514002832821, -17.09815260999999964 ) ) ;
#7140 = DIRECTION ( 'NONE',  ( 0.000000000000000000, 0.000000000000000000, 1.000000000000000000 ) ) ;
#7141 = CARTESIAN_POINT ( 'NONE',  ( 0.8184510536726904428, -27.48788286177519780, 5.736540937228021164 ) ) ;
#7142 = VERTEX_POINT ( 'NONE', #9208 ) ;
#7143 = CARTESIAN_POINT ( 'NONE',  ( -23.38367611648533639, -15.03487154286002436, 4.267303388019339394 ) ) ;
#7144 = CARTESIAN_POINT ( 'NONE',  ( 1.311146135404979818, -27.76947565989378219, 4.240358041999986227 ) ) ;
#7145 = CARTESIAN_POINT ( 'NONE',  ( -14.89999999969999855, -27.00000000000000000, -28.40000000020000215 ) ) ;
#7146 = EDGE_CURVE ( 'NONE', #19698, #5036, #29129, .T. ) ;
#7147 = DIRECTION ( 'NONE',  ( 2.415891560877031462E-12, -0.9341647027306021478, -0.3568421334038983650 ) ) ;
#7148 = CARTESIAN_POINT ( 'NONE',  ( -16.85343921422224156, -7.900182044607009679, 0.000000000000000000 ) ) ;
#7149 = DIRECTION ( 'NONE',  ( 0.8086898287149010267, 0.000000000000000000, 0.5882352938519278540 ) ) ;
#7150 = DIRECTION ( 'NONE',  ( 7.764622278472185525E-13, 0.9341647027306024809, 0.3568421334038978099 ) ) ;
#7151 = ORIENTED_EDGE ( 'NONE', *, *, #25427, .T. ) ;
#7152 = AXIS2_PLACEMENT_3D ( 'NONE', #20214, #8873, #25421 ) ;
#7153 = CARTESIAN_POINT ( 'NONE',  ( -10.69999999999999929, -24.00000000000000000, -28.40000000000000213 ) ) ;
#7154 = CARTESIAN_POINT ( 'NONE',  ( -7.999999999660042604, -18.28443193496838504, -36.42483736938474692 ) ) ;
#7155 = CARTESIAN_POINT ( 'NONE',  ( -27.79960709041389677, 4.276745829942281141, 0.5514269430000329208 ) ) ;
#7156 = EDGE_CURVE ( 'NONE', #24307, #10785, #14074, .T. ) ;
#7157 = B_SPLINE_CURVE_WITH_KNOTS ( 'NONE', 1,
 ( #11713, #28232 ),
 .UNSPECIFIED., .F., .F.,
 ( 2, 2 ),
 ( -2.555864960449999711E-06, 0.7000000000009999335 ),
 .UNSPECIFIED. ) ;
#7158 = CARTESIAN_POINT ( 'NONE',  ( 24.41841038956698640, 14.69667349781389376, 6.099998581000020792 ) ) ;
#7159 = ORIENTED_EDGE ( 'NONE', *, *, #4926, .F. ) ;
#7160 = CARTESIAN_POINT ( 'NONE',  ( 24.34663841809999951, -12.78636765230000094, 5.000000000000000000 ) ) ;
#7161 = ORIENTED_EDGE ( 'NONE', *, *, #5979, .T. ) ;
#7162 = CARTESIAN_POINT ( 'NONE',  ( 23.88383647311231428, 15.55037089993357746, 5.498277358143902838 ) ) ;
#7163 = VECTOR ( 'NONE', #4493, 1000.000000000000000 ) ;
#7164 = CARTESIAN_POINT ( 'NONE',  ( 23.76534794177020871, 14.42397062701149935, 6.095965061000018892 ) ) ;
#7165 = ORIENTED_EDGE ( 'NONE', *, *, #20020, .T. ) ;
#7166 = CARTESIAN_POINT ( 'NONE',  ( -4.217400109093717653, 2.917745507991296616, -26.40529765530000361 ) ) ;
#7167 = EDGE_CURVE ( 'NONE', #5533, #21014, #14219, .T. ) ;
#7168 = FACE_OUTER_BOUND ( 'NONE', #7616, .T. ) ;
#7169 = CARTESIAN_POINT ( 'NONE',  ( 4.531630834892032667, -0.6723478992683162847, -46.13818262062499542 ) ) ;
#7170 = DIRECTION ( 'NONE',  ( -0.000000000000000000, -0.000000000000000000, -1.000000000000000000 ) ) ;
#7171 = VECTOR ( 'NONE', #9309, 1000.000000000000000 ) ;
#7172 = CARTESIAN_POINT ( 'NONE',  ( 23.62697774660000150, -14.64965012220000062, 224.3193082299999901 ) ) ;
#7173 = UNCERTAINTY_MEASURE_WITH_UNIT (LENGTH_MEASURE( 1.000000000000000082E-05 ), #3868, 'distance_accuracy_value', 'NONE');
#7174 = DIRECTION ( 'NONE',  ( 0.000000000000000000, 0.000000000000000000, -1.000000000000000000 ) ) ;
#7175 = CARTESIAN_POINT ( 'NONE',  ( -10.00000000060000005, -25.00000000000000000, -4.837481085199997644 ) ) ;
#7176 = ORIENTED_EDGE ( 'NONE', *, *, #15461, .T. ) ;
#7177 = FACE_OUTER_BOUND ( 'NONE', #26512, .T. ) ;
#7178 = DIRECTION ( 'NONE',  ( 2.257150022439999944E-12, 0.000000000000000000, 1.000000000000000000 ) ) ;
#7179 = CARTESIAN_POINT ( 'NONE',  ( -0.8513360036590000846, -12.01011570999999911, 231.9999989789999972 ) ) ;
#7180 = B_SPLINE_CURVE_WITH_KNOTS ( 'NONE', 3,
 ( #5458, #19788, #12691, #17566, #20401, #15369, #5610, #3558, #15064, #12539 ),
 .UNSPECIFIED., .F., .F.,
 ( 4, 2, 2, 2, 4 ),
 ( 0.000000000000000000, 0.2500000000000000000, 0.5000000000000000000, 0.7500000000000000000, 1.000000000000000000 ),
 .UNSPECIFIED. ) ;
#7181 = CARTESIAN_POINT ( 'NONE',  ( -22.83911268609999823, 16.42879705520000044, 222.0000000000000000 ) ) ;
#7182 = DIRECTION ( 'NONE',  ( 0.000000000000000000, 1.000000000000000000, 0.000000000000000000 ) ) ;
#7183 = CARTESIAN_POINT ( 'NONE',  ( 11.51831195910000005, 3.792349640119999865, 230.6412452697800006 ) ) ;
#7184 =( REPRESENTATION_RELATIONSHIP ('NONE','NONE', #2712, #27424 ) REPRESENTATION_RELATIONSHIP_WITH_TRANSFORMATION ( #28607 )SHAPE_REPRESENTATION_RELATIONSHIP( ) );
#7185 = CARTESIAN_POINT ( 'NONE',  ( 4.638687372290002386, 3.765626869285956690, -39.31578811165251608 ) ) ;
#7186 = DIRECTION ( 'NONE',  ( 0.000000000000000000, 0.000000000000000000, 1.000000000000000000 ) ) ;
#7187 = CARTESIAN_POINT ( 'NONE',  ( 23.93355402185607872, -14.14369205957050468, 226.0731811994463669 ) ) ;
#7188 = CARTESIAN_POINT ( 'NONE',  ( -6.253676594953650358, -16.79482187635032986, -74.99114480175852293 ) ) ;
#7189 = CARTESIAN_POINT ( 'NONE',  ( -9.000000000229999131, 20.99999999999999645, -48.10000000000000142 ) ) ;
#7190 = CARTESIAN_POINT ( 'NONE',  ( 18.26905192736944983, 10.87373459873798609, -0.6999999999999784173 ) ) ;
#7191 = EDGE_CURVE ( 'NONE', #21717, #24422, #6698, .T. ) ;
#7192 = ORIENTED_EDGE ( 'NONE', *, *, #20888, .F. ) ;
#7193 = DIRECTION ( 'NONE',  ( 0.000000000000000000, 0.000000000000000000, -1.000000000000000000 ) ) ;
#7194 = EDGE_CURVE ( 'NONE', #25472, #27663, #29627, .T. ) ;
#7195 = ORIENTED_EDGE ( 'NONE', *, *, #12872, .F. ) ;
#7196 = EDGE_CURVE ( 'NONE', #29138, #30054, #11431, .T. ) ;
#7197 = CARTESIAN_POINT ( 'NONE',  ( -13.00000000000000000, 23.81663212713006672, -62.33813991915980779 ) ) ;
#7198 = ADVANCED_FACE ( 'NONE', ( #26065 ), #2990, .F. ) ;
#7199 = CARTESIAN_POINT ( 'NONE',  ( 5.235465350887244185, -2.882605534178610984, -58.30843849682499780 ) ) ;
#7200 = ORIENTED_EDGE ( 'NONE', *, *, #13556, .F. ) ;
#7201 = ITEM_DEFINED_TRANSFORMATION ( 'NONE', 'NONE', #21378,  #17722 ) ;
#7202 = ORIENTED_EDGE ( 'NONE', *, *, #20537, .T. ) ;
#7203 = CARTESIAN_POINT ( 'NONE',  ( -17.38583936189946755, -25.68983096307264091, -23.38292375445472260 ) ) ;
#7204 = VERTEX_POINT ( 'NONE', #23863 ) ;
#7205 = AXIS2_PLACEMENT_3D ( 'NONE', #3149, #810, #25176 ) ;
#7206 = AXIS2_PLACEMENT_3D ( 'NONE', #10700, #10400, #25178 ) ;
#7207 = CARTESIAN_POINT ( 'NONE',  ( -16.04158851053540857, -9.763538383445707680, -0.6999999999999784173 ) ) ;
#7208 = CARTESIAN_POINT ( 'NONE',  ( -27.79539923781684507, -0.5057481689249136991, 3.799999999999998046 ) ) ;
#7209 = VECTOR ( 'NONE', #18568, 1000.000000000000000 ) ;
#7210 = DIRECTION ( 'NONE',  ( 2.250897877190000270E-12, 0.000000000000000000, 1.000000000000000000 ) ) ;
#7211 = CARTESIAN_POINT ( 'NONE',  ( -8.999999999970000886, 20.99999999999999645, -45.10000000000000142 ) ) ;
#7212 = CYLINDRICAL_SURFACE ( 'NONE', #20460, 3.999999999999999112 ) ;
#7213 = CARTESIAN_POINT ( 'NONE',  ( -5.680091681631305178, 1.608645723366325164, -6.310827254900001293 ) ) ;
#7214 = VECTOR ( 'NONE', #19836, 1000.000000000000000 ) ;
#7215 = CARTESIAN_POINT ( 'NONE',  ( 25.92643298289999976, -14.85855223419999938, 229.7625741969999922 ) ) ;
#7216 = ORIENTED_EDGE ( 'NONE', *, *, #14083, .T. ) ;
#7217 = LINE ( 'NONE', #11629, #1427 ) ;
#7218 = CARTESIAN_POINT ( 'NONE',  ( 3.292208284841127597, -3.106818514002832821, -18.97315261000000319 ) ) ;
#7219 = CARTESIAN_POINT ( 'NONE',  ( -27.79999999999999716, -2.360778239559999931E-11, 229.0000000000000000 ) ) ;
#7220 = CARTESIAN_POINT ( 'NONE',  ( 24.44014313072642963, -13.24968496497942105, 6.079865069000017996 ) ) ;
#7221 = CARTESIAN_POINT ( 'NONE',  ( -11.08631337909999992, -4.914038143670000025, 230.6412452697800006 ) ) ;
#7222 = CYLINDRICAL_SURFACE ( 'NONE', #6628, 1.100000000000000089 ) ;
#7223 = CARTESIAN_POINT ( 'NONE',  ( -19.99465714571108066, 19.99999931014700749, 0.1508170869999880814 ) ) ;
#7224 = CARTESIAN_POINT ( 'NONE',  ( -10.69999999999999929, -126.7743301060000078, -33.87904238509999999 ) ) ;
#7225 = CARTESIAN_POINT ( 'NONE',  ( 1.087555935787781758, -26.77834284438278090, 224.7819484277976869 ) ) ;
#7226 = CARTESIAN_POINT ( 'NONE',  ( -4.783592046303898115, -19.82595474192468288, -31.14721076547942147 ) ) ;
#7227 = CIRCLE ( 'NONE', #3769, 27.69999999999999929 ) ;
#7228 = AXIS2_PLACEMENT_3D ( 'NONE', #30175, #30339, #27813 ) ;
#7229 = CIRCLE ( 'NONE', #27843, 26.80000000000000071 ) ;
#7230 = DIRECTION ( 'NONE',  ( 0.000000000000000000, 0.000000000000000000, -1.000000000000000000 ) ) ;
#7231 = ORIENTED_EDGE ( 'NONE', *, *, #21668, .F. ) ;
#7232 = AXIS2_PLACEMENT_3D ( 'NONE', #17061, #19118, #26661 ) ;
#7233 = CARTESIAN_POINT ( 'NONE',  ( -17.64799051141838859, -8.260028345153997975, 0.000000000000000000 ) ) ;
#7234 = EDGE_CURVE ( 'NONE', #16248, #8336, #14548, .T. ) ;
#7235 = LINE ( 'NONE', #7954, #1645 ) ;
#7236 = ORIENTED_EDGE ( 'NONE', *, *, #26168, .T. ) ;
#7237 = CARTESIAN_POINT ( 'NONE',  ( 24.14619884838972297, -13.16136950037729569, 4.119508997699939279 ) ) ;
#7238 = CARTESIAN_POINT ( 'NONE',  ( -4.848570193085766533, 0.4842359979205582143, -47.62737393802499497 ) ) ;
#7239 = ORIENTED_EDGE ( 'NONE', *, *, #402, .F. ) ;
#7240 = VERTEX_POINT ( 'NONE', #16758 ) ;
#7241 = SURFACE_STYLE_FILL_AREA ( #16988 ) ;
#7242 = B_SPLINE_SURFACE_WITH_KNOTS ( 'NONE', 5, 5, ( 
 ( #29524, #20096, #3397, #22454, #7963, #29684, #13150, #17707, #22758 ),
 ( #17563, #1207, #27170, #15061, #8268, #5456, #27321, #27469, #29986 ),
 ( #24963, #15207, #8111, #13001, #12852, #3089, #18019, #24810, #5607 ),
 ( #10959, #27015, #5763, #5913, #27625, #15668, #904, #20553, #22612 ),
 ( #24656, #6071, #25279, #10644, #17408, #20236, #15514, #3712, #29831 ),
 ( #25120, #13313, #22924, #3246, #750, #30149, #1364, #11429, #11272 ),
 ( #25600, #4505, #8741, #1525, #21336, #23403, #4186, #23234, #9206 ),
 ( #28104, #21031, #8579, #30477, #30632, #26062, #2144, #8901, #11732 ),
 ( #9058, #18808, #18180, #25911, #4033, #14103, #18351, #4346, #15989 ) ),
 .UNSPECIFIED., .F., .F., .F.,
 ( 6, 3, 6 ),
 ( 6, 3, 6 ),
 ( 0.000000000000000000, 53.20205529499999386, 91.13698440880000362 ),
 ( 8.011061266649999624, 8.831591450809998634, 9.652121634960000307 ),
 .UNSPECIFIED. ) ;
#7243 = ORIENTED_EDGE ( 'NONE', *, *, #22943, .T. ) ;
#7244 = DIRECTION ( 'NONE',  ( 0.000000000000000000, 0.000000000000000000, -1.000000000000000000 ) ) ;
#7245 = ORIENTED_EDGE ( 'NONE', *, *, #15837, .T. ) ;
#7246 = CARTESIAN_POINT ( 'NONE',  ( 17.82602571120844459, 11.89215903477950853, -0.6999999999999783062 ) ) ;
#7247 = CARTESIAN_POINT ( 'NONE',  ( -4.861312627775142836, -10.76947865206767219, -35.56434929207025419 ) ) ;
#7248 = CARTESIAN_POINT ( 'NONE',  ( -16.83342759582943060, -8.999999999996580513, -0.6999999999999784173 ) ) ;
#7249 = CARTESIAN_POINT ( 'NONE',  ( 0.3471370043377995929, 4.633915050096243604, -35.69999999999999574 ) ) ;
#7250 = DIRECTION ( 'NONE',  ( -1.000000000000000000, 0.000000000000000000, -2.257144471330000330E-12 ) ) ;
#7251 = CARTESIAN_POINT ( 'NONE',  ( -24.20792486932886689, 13.66932879934886813, 6.079865099000020479 ) ) ;
#7252 = DIRECTION ( 'NONE',  ( 0.000000000000000000, -0.3420201433259318913, 0.9396926207858126157 ) ) ;
#7253 = AXIS2_PLACEMENT_3D ( 'NONE', #18486, #21164, #30760 ) ;
#7254 = CARTESIAN_POINT ( 'NONE',  ( -3.389121647030000073, -11.55088358959999972, 224.6412452697800290 ) ) ;
#7255 = EDGE_CURVE ( 'NONE', #2554, #1635, #26215, .T. ) ;
#7256 = PRESENTATION_LAYER_ASSIGNMENT (  '', '', ( #5739 ) ) ;
#7257 = AXIS2_PLACEMENT_3D ( 'NONE', #16164, #4209, #30802 ) ;
#7258 = AXIS2_PLACEMENT_3D ( 'NONE', #23955, #11975, #34 ) ;
#7259 = CARTESIAN_POINT ( 'NONE',  ( -3.099128499470596765, -3.102542665468459138, -10.31399163100000216 ) ) ;
#7260 = CARTESIAN_POINT ( 'NONE',  ( 3.790912472548402246, -2.108217834232220866, -26.43037294500000556 ) ) ;
#7261 = AXIS2_PLACEMENT_3D ( 'NONE', #10354, #3259, #27181 ) ;
#7262 = CARTESIAN_POINT ( 'NONE',  ( -2.374791981039476862, -2.610414167372405281, 0.000000000000000000 ) ) ;
#7263 = CARTESIAN_POINT ( 'NONE',  ( 23.77947513710800109, -14.40125623032519719, 5.208432824000020389 ) ) ;
#7264 = CARTESIAN_POINT ( 'NONE',  ( 19.65705194378976728, 20.00000012267804905, -0.1821635029999879585 ) ) ;
#7265 = CARTESIAN_POINT ( 'NONE',  ( 5.949264573234793296, -30.44932768689938740, -79.96097848041759448 ) ) ;
#7266 = CARTESIAN_POINT ( 'NONE',  ( -3.331422745097512017, -2.438398348906446689, -18.87254627010000263 ) ) ;
#7267 = EDGE_CURVE ( 'NONE', #3758, #21856, #28106, .T. ) ;
#7268 = CARTESIAN_POINT ( 'NONE',  ( 16.90560620815911719, 9.921746937094770402, -1.400000000000001910 ) ) ;
#7269 = CARTESIAN_POINT ( 'NONE',  ( -24.31416968206321627, -13.47842985394946780, 4.493023692000025271 ) ) ;
#7270 = DIRECTION ( 'NONE',  ( 1.000000000000000000, 0.000000000000000000, 0.000000000000000000 ) ) ;
#7271 = ORIENTED_EDGE ( 'NONE', *, *, #22721, .T. ) ;
#7272 = CARTESIAN_POINT ( 'NONE',  ( 18.05835842950707359, 10.34011310949354367, -4.336808689942018722E-16 ) ) ;
#7273 = CARTESIAN_POINT ( 'NONE',  ( 10.69999999999999929, -24.00000000000000000, -28.40000000000000213 ) ) ;
#7274 = ORIENTED_EDGE ( 'NONE', *, *, #21760, .F. ) ;
#7275 = CARTESIAN_POINT ( 'NONE',  ( 7.000000000115440102, -60.75400889061052112, -3.446705952631804681 ) ) ;
#7276 = CARTESIAN_POINT ( 'NONE',  ( 8.000000000284819279, -13.66682223737133128, -36.55330428412179344 ) ) ;
#7277 = ORIENTED_EDGE ( 'NONE', *, *, #5957, .F. ) ;
#7278 = CIRCLE ( 'NONE', #12800, 27.50000000000000000 ) ;
#7279 = EDGE_LOOP ( 'NONE', ( #25249, #222, #29206, #18058 ) ) ;
#7280 = VERTEX_POINT ( 'NONE', #8903 ) ;
#7281 = VECTOR ( 'NONE', #19344, 1000.000000000000000 ) ;
#7282 = EDGE_LOOP ( 'NONE', ( #22506, #5529, #3010, #6057 ) ) ;
#7283 = LINE ( 'NONE', #21759, #13453 ) ;
#7284 = EDGE_CURVE ( 'NONE', #9026, #11038, #16554, .T. ) ;
#7285 = LINE ( 'NONE', #18928, #8932 ) ;
#7286 = CARTESIAN_POINT ( 'NONE',  ( -2.730738507911396606, 1.619674855095874610, -68.28881611251394190 ) ) ;
#7287 = EDGE_LOOP ( 'NONE', ( #28482, #19702, #16950, #137, #25671 ) ) ;
#7288 = DIRECTION ( 'NONE',  ( -2.764840495839172918E-12, -0.9128796883888953273, 0.4082287037029531107 ) ) ;
#7289 = DIRECTION ( 'NONE',  ( 0.8660254037843290176, 0.5000000000001899592, 0.000000000000000000 ) ) ;
#7290 = CARTESIAN_POINT ( 'NONE',  ( 19.56389002122311638, 19.56882009050699622, 0.5006759800000037952 ) ) ;
#7291 = AXIS2_PLACEMENT_3D ( 'NONE', #27755, #13755, #20999 ) ;
#7292 =( GEOMETRIC_REPRESENTATION_CONTEXT ( 3 ) GLOBAL_UNCERTAINTY_ASSIGNED_CONTEXT ( ( #19755 ) ) GLOBAL_UNIT_ASSIGNED_CONTEXT ( ( #17783, #29604, #17934 ) ) REPRESENTATION_CONTEXT ( 'NONE', 'WORKASPACE' ) );
#7293 = CARTESIAN_POINT ( 'NONE',  ( -9.000000000000000000, -55.00000000000000000, -43.39999999999999858 ) ) ;
#7294 = CARTESIAN_POINT ( 'NONE',  ( 2.911762171867607663, -4.051295066173226544, -0.6999994862911463889 ) ) ;
#7295 = VERTEX_POINT ( 'NONE', #17378 ) ;
#7296 = CARTESIAN_POINT ( 'NONE',  ( 0.000000000000000000, 0.000000000000000000, 115.0000000000000000 ) ) ;
#7297 = CARTESIAN_POINT ( 'NONE',  ( -2.183849900456024784, 3.899926742306370819, -16.17761783619999960 ) ) ;
#7298 = CARTESIAN_POINT ( 'NONE',  ( -7.999999999650683868, -16.30392683535412957, -38.02387007715461920 ) ) ;
#7299 = DIRECTION ( 'NONE',  ( 0.000000000000000000, 0.000000000000000000, -1.000000000000000000 ) ) ;
#7300 = ORIENTED_EDGE ( 'NONE', *, *, #5592, .T. ) ;
#7301 = CARTESIAN_POINT ( 'NONE',  ( -23.46764062199439493, -14.90374525705096254, 4.113458908961371563 ) ) ;
#7302 = CARTESIAN_POINT ( 'NONE',  ( 25.98552618960000160, 10.26029398309999863, 222.0000000000000000 ) ) ;
#7303 = VECTOR ( 'NONE', #12759, 1000.000000000000114 ) ;
#7304 = DIRECTION ( 'NONE',  ( 0.000000000000000000, -1.000000000000000000, 0.000000000000000000 ) ) ;
#7305 = ADVANCED_FACE ( 'NONE', ( #7625, #14883 ), #9842, .T. ) ;
#7306 = LINE ( 'NONE', #5089, #21018 ) ;
#7307 = B_SPLINE_CURVE_WITH_KNOTS ( 'NONE', 1,
 ( #12219, #443 ),
 .UNSPECIFIED., .F., .F.,
 ( 2, 2 ),
 ( 1.500000000000000000, 3.500000000000000000 ),
 .UNSPECIFIED. ) ;
#7308 = DIRECTION ( 'NONE',  ( -0.000000000000000000, -0.000000000000000000, -1.000000000000000000 ) ) ;
#7309 = CARTESIAN_POINT ( 'NONE',  ( -11.09640325699999863, -24.58282406889999905, -1.600739421300005683 ) ) ;
#7310 = CARTESIAN_POINT ( 'NONE',  ( -13.76031144620000113, -12.03544455119999945, 230.6999999999999886 ) ) ;
#7311 = ORIENTED_EDGE ( 'NONE', *, *, #8643, .T. ) ;
#7312 = LINE ( 'NONE', #4635, #29858 ) ;
#7313 = FACE_OUTER_BOUND ( 'NONE', #1444, .T. ) ;
#7314 = CARTESIAN_POINT ( 'NONE',  ( 2.211450541897235222, -4.299781033209638892, -68.10000000002500542 ) ) ;
#7315 = CARTESIAN_POINT ( 'NONE',  ( -4.859269776546366160, -1.038628159466365108, -68.10000000002500542 ) ) ;
#7316 = COLOUR_RGB ( '', 0.31764706, 0.68627451, 0.89019608) ;
#7317 = EDGE_CURVE ( 'NONE', #16606, #6097, #2178, .T. ) ;
#7318 = VERTEX_POINT ( 'NONE', #19438 ) ;
#7319 = EDGE_CURVE ( 'NONE', #26056, #26210, #10310, .T. ) ;
#7320 = CARTESIAN_POINT ( 'NONE',  ( 21.88912777999999903, 15.65358089960000321, 230.6999999999999886 ) ) ;
#7321 = ORIENTED_EDGE ( 'NONE', *, *, #12507, .F. ) ;
#7322 = CARTESIAN_POINT ( 'NONE',  ( 0.5401834767574382745, -27.79499634052776358, 3.899998581000013509 ) ) ;
#7323 = ORIENTED_EDGE ( 'NONE', *, *, #30535, .F. ) ;
#7324 = CARTESIAN_POINT ( 'NONE',  ( -4.856400125594941386, 3.359828160699422472, -26.46779765530000361 ) ) ;
#7325 = CARTESIAN_POINT ( 'NONE',  ( -1.484924240490000047, -1.484924240490000047, 226.6412452697800006 ) ) ;
#7326 = ADVANCED_FACE ( 'NONE', ( #24312 ), #5573, .T. ) ;
#7327 = CARTESIAN_POINT ( 'NONE',  ( -4.178199994060140199, -1.098053884355548737, -56.45102360502500005 ) ) ;
#7328 = CARTESIAN_POINT ( 'NONE',  ( 7.000000000000000000, -15.18061163548115466, -76.53197586718597734 ) ) ;
#7329 = CARTESIAN_POINT ( 'NONE',  ( -23.78314118791541532, -14.39461388281431375, 3.901343066999990228 ) ) ;
#7330 = CARTESIAN_POINT ( 'NONE',  ( 23.83740787290000185, -14.30495753649999990, 223.9972528570000065 ) ) ;
#7331 = CARTESIAN_POINT ( 'NONE',  ( -4.826218213038748317, -18.30365710847786787, -28.55187910938255769 ) ) ;
#7332 = B_SPLINE_CURVE_WITH_KNOTS ( 'NONE', 5,
 ( #2284, #29307, #11867, #2581, #9657, #21778 ),
 .UNSPECIFIED., .F., .F.,
 ( 6, 6 ),
 ( 71.86404503510000552, 94.75474465359999954 ),
 .UNSPECIFIED. ) ;
#7333 = CARTESIAN_POINT ( 'NONE',  ( -8.000000000002907896, -107.4273096626132116, 14.66297538107212262 ) ) ;
#7334 = EDGE_CURVE ( 'NONE', #1312, #22717, #7477, .T. ) ;
#7335 = DIRECTION ( 'NONE',  ( 1.000000000000000000, 7.807837518093016606E-13, 2.626330150305131362E-12 ) ) ;
#7336 = VERTEX_POINT ( 'NONE', #21962 ) ;
#7337 = CARTESIAN_POINT ( 'NONE',  ( 21.02336020643863179, 19.26966202639587067, 4.000000000000003553 ) ) ;
#7338 = CARTESIAN_POINT ( 'NONE',  ( 23.25782843551338885, -13.31625947593092896, 223.8999999999988404 ) ) ;
#7339 = CARTESIAN_POINT ( 'NONE',  ( -23.23277126416379801, -15.26692729116844482, 4.999998581000003384 ) ) ;
#7340 = DIRECTION ( 'NONE',  ( -0.000000000000000000, -0.000000000000000000, 1.000000000000000000 ) ) ;
#7341 = CARTESIAN_POINT ( 'NONE',  ( -12.47178235753292697, -31.04315797141627797, -31.83918434892504834 ) ) ;
#7342 = CARTESIAN_POINT ( 'NONE',  ( -4.861312627709997614, 3.765626869323773995, -39.31578811167095466 ) ) ;
#7343 = DIRECTION ( 'NONE',  ( -3.924189347185961537E-12, 0.4082287037029530552, 0.9128796883888952163 ) ) ;
#7344 = CARTESIAN_POINT ( 'NONE',  ( -0.9242233308569890449, -26.78436826007333238, 225.5979291942194891 ) ) ;
#7345 = CARTESIAN_POINT ( 'NONE',  ( -16.83342759575507586, 10.99999999997565503, -0.6999999999999784173 ) ) ;
#7346 = CARTESIAN_POINT ( 'NONE',  ( 9.999999999969999109, -24.87872937930000106, -30.52127062269999769 ) ) ;
#7347 = EDGE_CURVE ( 'NONE', #18002, #30101, #26200, .T. ) ;
#7348 = CARTESIAN_POINT ( 'NONE',  ( 12.12499559729999810, 21.69999999929999390, -55.73512174120000395 ) ) ;
#7349 = CARTESIAN_POINT ( 'NONE',  ( -16.06988964647317886, -8.208161364834239748, 0.000000000000000000 ) ) ;
#7350 = CARTESIAN_POINT ( 'NONE',  ( 18.24356172875952709, 10.73282780903411293, -0.6999999999999784173 ) ) ;
#7351 = VERTEX_POINT ( 'NONE', #24474 ) ;
#7352 = CARTESIAN_POINT ( 'NONE',  ( -8.999999999699999975, 21.69999999919999212, -70.09999999999999432 ) ) ;
#7353 = ORIENTED_EDGE ( 'NONE', *, *, #6772, .F. ) ;
#7354 = CARTESIAN_POINT ( 'NONE',  ( 24.60810180234884825, -14.37755052939759715, 223.9000014190000627 ) ) ;
#7355 = CARTESIAN_POINT ( 'NONE',  ( -5.623491485972666126, 3.092612689740418919, -60.29908057272499633 ) ) ;
#7356 = ORIENTED_EDGE ( 'NONE', *, *, #9844, .F. ) ;
#7357 = ITEM_DEFINED_TRANSFORMATION ( 'NONE', 'NONE', #21901,  #17722 ) ;
#7358 = ORIENTED_EDGE ( 'NONE', *, *, #15081, .T. ) ;
#7359 = CARTESIAN_POINT ( 'NONE',  ( -17.30852986269440308, -26.11984913498134020, -23.13465264714667313 ) ) ;
#7360 = ORIENTED_EDGE ( 'NONE', *, *, #25956, .T. ) ;
#7361 = CARTESIAN_POINT ( 'NONE',  ( 2.100000000000000089, -1.998401444330000344E-15, 226.6412452697800006 ) ) ;
#7362 = CARTESIAN_POINT ( 'NONE',  ( 12.27469135525410593, 20.99999999997359978, -55.79567638067133828 ) ) ;
#7363 =( LENGTH_UNIT ( ) NAMED_UNIT ( * ) SI_UNIT ( .MILLI., .METRE. ) );
#7364 = DIRECTION ( 'NONE',  ( 0.000000000000000000, 0.000000000000000000, 1.000000000000000000 ) ) ;
#7365 = EDGE_CURVE ( 'NONE', #19758, #8971, #29109, .T. ) ;
#7366 = DIRECTION ( 'NONE',  ( 1.000000000000000000, -1.843431230208684274E-12, 2.650498504958264790E-12 ) ) ;
#7367 = CARTESIAN_POINT ( 'NONE',  ( 6.086077541567210147, 0.7980478301550381071, -5.626979598400000171 ) ) ;
#7368 = DIRECTION ( 'NONE',  ( 1.000000000000000000, 0.000000000000000000, 0.000000000000000000 ) ) ;
#7369 = ORIENTED_EDGE ( 'NONE', *, *, #20595, .T. ) ;
#7370 = CARTESIAN_POINT ( 'NONE',  ( 13.67718073920000066, 20.99999999999999645, -57.16242423349999768 ) ) ;
#7371 = EDGE_CURVE ( 'NONE', #19781, #20878, #13424, .T. ) ;
#7372 = CARTESIAN_POINT ( 'NONE',  ( -3.331422745097512017, -2.438398348906446689, -18.87254627010000263 ) ) ;
#7373 = CARTESIAN_POINT ( 'NONE',  ( -27.79999999999999716, -2.354383354940000152E-11, 222.0000000000000000 ) ) ;
#7374 = PLANE ( 'NONE',  #22565 ) ;
#7375 = CARTESIAN_POINT ( 'NONE',  ( -11.51831195970000010, -3.792349639629999825, 230.6412452697800006 ) ) ;
#7376 = FACE_BOUND ( 'NONE', #27959, .T. ) ;
#7377 = CARTESIAN_POINT ( 'NONE',  ( 3.248659393266396300, -2.157825791482658850, -42.95875473022500302 ) ) ;
#7378 = CARTESIAN_POINT ( 'NONE',  ( -7.999999999985950794, -116.8591659214701792, 11.34031266722930908 ) ) ;
#7379 = CARTESIAN_POINT ( 'NONE',  ( -16.81341597763548990, -10.09981795544978311, -0.6999999989999727834 ) ) ;
#7380 = CYLINDRICAL_SURFACE ( 'NONE', #24865, 5.000000000000001776 ) ;
#7381 = CARTESIAN_POINT ( 'NONE',  ( -10.69999999989999928, -30.49251257979999963, -21.04205368470000082 ) ) ;
#7382 = B_SPLINE_CURVE_WITH_KNOTS ( 'NONE', 3,
 ( #5849, #24747, #7897, #17503, #17949, #692, #10279, #543, #24907, #27259, #5542, #22694 ),
 .UNSPECIFIED., .F., .F.,
 ( 4, 2, 2, 2, 2, 4 ),
 ( 0.000000000000000000, 0.2500000000000267009, 0.5000000000000534017, 0.6250000000000505151, 0.7500000000000476286, 1.000000000000000000 ),
 .UNSPECIFIED. ) ;
#7383 = ORIENTED_EDGE ( 'NONE', *, *, #6355, .F. ) ;
#7384 = CARTESIAN_POINT ( 'NONE',  ( -4.188726303739424672, 1.192588472141205891, -31.80158078969999735 ) ) ;
#7385 = CARTESIAN_POINT ( 'NONE',  ( 9.993285220779503319, -25.61999708228222872, 93.60555127639999284 ) ) ;
#7386 = VERTEX_POINT ( 'NONE', #28878 ) ;
#7387 = CARTESIAN_POINT ( 'NONE',  ( 9.999999999971130649, -25.48914305972228078, -31.02135916551032935 ) ) ;
#7388 = CARTESIAN_POINT ( 'NONE',  ( 2.534862810676351330, -4.171999357468123115, -46.96669147672501055 ) ) ;
#7389 = ORIENTED_EDGE ( 'NONE', *, *, #9901, .T. ) ;
#7390 = ORIENTED_EDGE ( 'NONE', *, *, #9680, .F. ) ;
#7391 = DIRECTION ( 'NONE',  ( 0.000000000000000000, 0.000000000000000000, 1.000000000000000000 ) ) ;
#7392 = ORIENTED_EDGE ( 'NONE', *, *, #21231, .F. ) ;
#7393 = CARTESIAN_POINT ( 'NONE',  ( -7.999999999730326827, -27.67628966639927057, -25.46613455157947570 ) ) ;
#7394 = ORIENTED_EDGE ( 'NONE', *, *, #30316, .F. ) ;
#7395 = AXIS2_PLACEMENT_3D ( 'NONE', #1173, #20364, #24779 ) ;
#7396 = DIRECTION ( 'NONE',  ( 0.000000000000000000, 0.000000000000000000, 1.000000000000000000 ) ) ;
#7397 = CARTESIAN_POINT ( 'NONE',  ( -6.148616650685278628, -8.802192167974602910, -36.52385902140760976 ) ) ;
#7398 = CARTESIAN_POINT ( 'NONE',  ( 10.00000000000000000, 3.868893114322062843, -67.47016761578689170 ) ) ;
#7399 = CARTESIAN_POINT ( 'NONE',  ( 0.3593491040380148438, 4.319799995452766161, -35.70000000000000284 ) ) ;
#7400 = FACE_OUTER_BOUND ( 'NONE', #8418, .T. ) ;
#7401 = DIRECTION ( 'NONE',  ( 0.3633921898465292122, 0.9316362575375348731, 0.000000000000000000 ) ) ;
#7402 = DIRECTION ( 'NONE',  ( -0.000000000000000000, 1.000000000000000000, -2.257145581549999994E-12 ) ) ;
#7403 = CARTESIAN_POINT ( 'NONE',  ( -21.27524652179786457, 16.93536700441368126, -0.6999999999999784173 ) ) ;
#7404 = ORIENTED_EDGE ( 'NONE', *, *, #27861, .F. ) ;
#7405 = EDGE_CURVE ( 'NONE', #15775, #24427, #29333, .T. ) ;
#7406 = CARTESIAN_POINT ( 'NONE',  ( 5.967946066639521874, -1.056419632483374116, -9.371482634700001313 ) ) ;
#7407 = CARTESIAN_POINT ( 'NONE',  ( -4.346598770676711965, -0.007247149673127636568, -27.66856466010000659 ) ) ;
#7408 = CARTESIAN_POINT ( 'NONE',  ( 3.455601306038246001, 0.7156333712654180390, 0.000000000000000000 ) ) ;
#7409 = EDGE_CURVE ( 'NONE', #13409, #4540, #15031, .T. ) ;
#7410 = CARTESIAN_POINT ( 'NONE',  ( -16.81341597784800967, -10.09981795476353739, 0.000000000000000000 ) ) ;
#7411 = CARTESIAN_POINT ( 'NONE',  ( 19.06888577842656574, 19.69230313816537148, 0.2004941630000256492 ) ) ;
#7412 = FILL_AREA_STYLE ('',( #9933 ) ) ;
#7413 = CARTESIAN_POINT ( 'NONE',  ( 8.090238276950916685, -26.28358643434115649, 22.68593013736110109 ) ) ;
#7414 = CARTESIAN_POINT ( 'NONE',  ( 4.347198243976404974, 0.5700341643805826308, -5.626979598400000171 ) ) ;
#7415 = MECHANICAL_DESIGN_GEOMETRIC_PRESENTATION_REPRESENTATION (  '', ( #5899 ), #18465 ) ;
#7416 = VECTOR ( 'NONE', #14110, 1000.000000000000114 ) ;
#7417 = DIRECTION ( 'NONE',  ( 1.000000000000000000, 0.000000000000000000, 0.000000000000000000 ) ) ;
#7418 = CARTESIAN_POINT ( 'NONE',  ( -24.00926694310947695, -14.01467022312833421, 3.957524336000023624 ) ) ;
#7419 = DIRECTION ( 'NONE',  ( -0.9316362575375349842, 0.3633921898465292122, -0.000000000000000000 ) ) ;
#7420 = VERTEX_POINT ( 'NONE', #12654 ) ;
#7421 = CARTESIAN_POINT ( 'NONE',  ( 18.26375984360044313, -8.835417945884492141, -0.6999999999999783062 ) ) ;
#7422 = CARTESIAN_POINT ( 'NONE',  ( 4.638687372203635917, -15.07597047391499778, -33.46393288816293676 ) ) ;
#7423 = ORIENTED_EDGE ( 'NONE', *, *, #5009, .T. ) ;
#7424 = CARTESIAN_POINT ( 'NONE',  ( 24.68173674080000168, -14.25001227039999918, 226.1000014189999945 ) ) ;
#7425 = CARTESIAN_POINT ( 'NONE',  ( -16.81341597756113515, 9.900182044522454206, -0.6999999999999784173 ) ) ;
#7426 = ORIENTED_EDGE ( 'NONE', *, *, #29497, .F. ) ;
#7427 = ORIENTED_EDGE ( 'NONE', *, *, #18799, .F. ) ;
#7428 = B_SPLINE_SURFACE_WITH_KNOTS ( 'NONE', 5, 1, ( 
 ( #16630, #26239 ),
 ( #20084, #14902 ),
 ( #22748, #12846 ),
 ( #19778, #895 ),
 ( #3388, #15056 ),
 ( #27007, #3238 ),
 ( #29675, #25112 ),
 ( #10635, #3545 ),
 ( #594, #8105 ),
 ( #27164, #1043 ),
 ( #29360, #5447 ),
 ( #10177, #22448 ) ),
 .UNSPECIFIED., .F., .F., .F.,
 ( 6, 3, 3, 6 ),
 ( 2, 2 ),
 ( 0.000000000000000000, 0.5717440563929999664, 1.143488112780000066, 1.429360140980000082 ),
 ( -0.7000000000009999335, 0.002002273571169999912 ),
 .UNSPECIFIED. ) ;
#7429 = EDGE_LOOP ( 'NONE', ( #1438, #5803 ) ) ;
#7430 = VECTOR ( 'NONE', #13987, 1000.000000000000000 ) ;
#7431 = EDGE_LOOP ( 'NONE', ( #20709, #19090, #6812, #15584 ) ) ;
#7432 = DIRECTION ( 'NONE',  ( -0.7071067811865475727, 0.7071067811865475727, 0.000000000000000000 ) ) ;
#7433 = CIRCLE ( 'NONE', #25015, 1.099999999570000497 ) ;
#7434 = CARTESIAN_POINT ( 'NONE',  ( 27.55801272791059731, 0.5014288284349769365, -0.5592437529999827461 ) ) ;
#7435 = CARTESIAN_POINT ( 'NONE',  ( -7.999999999683784502, -16.99089124002251694, -33.25453181222756882 ) ) ;
#7436 = EDGE_CURVE ( 'NONE', #3834, #30810, #30630, .T. ) ;
#7437 = ORIENTED_EDGE ( 'NONE', *, *, #2678, .F. ) ;
#7438 =( NAMED_UNIT ( * ) PLANE_ANGLE_UNIT ( ) SI_UNIT ( $, .RADIAN. ) );
#7439 = AXIS2_PLACEMENT_3D ( 'NONE', #14714, #19121, #28714 ) ;
#7440 = CARTESIAN_POINT ( 'NONE',  ( -13.46591448088098808, 21.69999999929855505, -56.74462827942989662 ) ) ;
#7441 = AXIS2_PLACEMENT_3D ( 'NONE', #26803, #10130, #5247 ) ;
#7442 = DIRECTION ( 'NONE',  ( 0.000000000000000000, 0.2713155151490714290, 0.9624904629342537765 ) ) ;
#7443 = CARTESIAN_POINT ( 'NONE',  ( 10.69999999999999929, -29.06671945340000107, -26.22544931050000017 ) ) ;
#7444 = EDGE_LOOP ( 'NONE', ( #20422, #16741, #20938, #23854 ) ) ;
#7445 = FACE_BOUND ( 'NONE', #16309, .T. ) ;
#7446 = B_SPLINE_CURVE_WITH_KNOTS ( 'NONE', 3,
 ( #8869, #15961, #25569, #4475, #18474, #1498, #8552, #11400, #4162, #28072 ),
 .UNSPECIFIED., .F., .F.,
 ( 4, 2, 2, 2, 4 ),
 ( 0.000000000000000000, 0.2499999999999998890, 0.4999999999999997780, 0.7499999999999998890, 1.000000000000000000 ),
 .UNSPECIFIED. ) ;
#7447 = CARTESIAN_POINT ( 'NONE',  ( 1.102985302404366097, 4.375751030832064181, -16.11330441500000177 ) ) ;
#7448 = CARTESIAN_POINT ( 'NONE',  ( 11.69999999989999928, 19.99999999999999645, -1.399999999999998579 ) ) ;
#7449 = CARTESIAN_POINT ( 'NONE',  ( 0.8471243414734038746, -27.48706736360548319, 5.703083847462546707 ) ) ;
#7450 = CARTESIAN_POINT ( 'NONE',  ( -12.60598845464734907, -27.44337724096553899, -33.91751872268586965 ) ) ;
#7451 = CARTESIAN_POINT ( 'NONE',  ( 0.000000000000000000, -3.434453875705480108, -72.25672407562892374 ) ) ;
#7452 = CARTESIAN_POINT ( 'NONE',  ( -24.73806702658698953, 12.68469578970483269, 4.322438790421920807 ) ) ;
#7453 = DIRECTION ( 'NONE',  ( 1.000000000000000000, 0.000000000000000000, 0.000000000000000000 ) ) ;
#7454 = CARTESIAN_POINT ( 'NONE',  ( 0.000000000000000000, -119.7166638525666826, -63.39999999999999858 ) ) ;
#7455 = CARTESIAN_POINT ( 'NONE',  ( -11.37440858360000107, -24.37257237719999736, -1.450121501800003099 ) ) ;
#7456 = DIRECTION ( 'NONE',  ( 0.000000000000000000, -0.7113488923935513686, 0.7028390664230806939 ) ) ;
#7457 = ORIENTED_EDGE ( 'NONE', *, *, #9897, .F. ) ;
#7458 = CARTESIAN_POINT ( 'NONE',  ( 27.79999999999999716, 2.355804440410000085E-11, 229.0000000000000000 ) ) ;
#7459 = B_SPLINE_CURVE_WITH_KNOTS ( 'NONE', 3,
 ( #563, #29022, #7468, #17064, #29170, #16906 ),
 .UNSPECIFIED., .F., .F.,
 ( 4, 2, 4 ),
 ( 0.000000000000000000, 0.5000000000000000000, 1.000000000000000000 ),
 .UNSPECIFIED. ) ;
#7460 = CARTESIAN_POINT ( 'NONE',  ( -27.08859402333790456, -0.4928875713652468016, 0.02487529600000981667 ) ) ;
#7461 = AXIS2_PLACEMENT_3D ( 'NONE', #18551, #27992, #27673 ) ;
#7462 = CARTESIAN_POINT ( 'NONE',  ( 23.80092420482279891, 14.36517094565843777, 6.099998581000020792 ) ) ;
#7463 = ORIENTED_EDGE ( 'NONE', *, *, #17830, .F. ) ;
#7464 = EDGE_CURVE ( 'NONE', #26031, #29777, #21083, .T. ) ;
#7465 = DIRECTION ( 'NONE',  ( 0.000000000000000000, -1.000000000000000000, 0.000000000000000000 ) ) ;
#7466 = SURFACE_STYLE_USAGE ( .BOTH. , #404 ) ;
#7467 = VERTEX_POINT ( 'NONE', #102 ) ;
#7468 = CARTESIAN_POINT ( 'NONE',  ( -11.19478429451004153, 19.99999999999999645, -1.527457921041847966 ) ) ;
#7469 = CARTESIAN_POINT ( 'NONE',  ( -1.746607907818665817, 4.818926816502865584, -69.95099036452499774 ) ) ;
#7470 = ORIENTED_EDGE ( 'NONE', *, *, #28437, .F. ) ;
#7471 = CARTESIAN_POINT ( 'NONE',  ( 0.09521150875770739708, -4.665041947735808492, -24.41888333260000365 ) ) ;
#7472 = EDGE_CURVE ( 'NONE', #10219, #19754, #19286, .T. ) ;
#7473 = CARTESIAN_POINT ( 'NONE',  ( -1.834980887776583636, -1.057731052603296362, 226.6412452697800006 ) ) ;
#7474 = AXIS2_PLACEMENT_3D ( 'NONE', #25606, #1836, #2149 ) ;
#7475 = B_SPLINE_CURVE_WITH_KNOTS ( 'NONE', 3,
 ( #2428, #12019, #77, #9655, #19258, #16270 ),
 .UNSPECIFIED., .F., .F.,
 ( 4, 2, 4 ),
 ( 0.000000000000000000, 0.5000000000000000000, 1.000000000000000000 ),
 .UNSPECIFIED. ) ;
#7476 = CARTESIAN_POINT ( 'NONE',  ( -3.468517234904579194, -2.575357395510371461, -56.27895058492499913 ) ) ;
#7477 = LINE ( 'NONE', #10153, #29605 ) ;
#7478 = CARTESIAN_POINT ( 'NONE',  ( -24.29089620838935204, -14.90695587844356673, 3.920145809000019632 ) ) ;
#7479 = CARTESIAN_POINT ( 'NONE',  ( -4.263497950344331322, -19.43679463443259792, -27.99921101064753159 ) ) ;
#7480 = PRODUCT_DEFINITION_CONTEXT ( 'detailed design', #15825, 'design' ) ;
#7481 = CARTESIAN_POINT ( 'NONE',  ( -8.350000000008115819, -22.83323352208430634, -39.84673050100227698 ) ) ;
#7482 = CARTESIAN_POINT ( 'NONE',  ( -17.27724273262455412, -22.00035689406917783, -26.42754666945129927 ) ) ;
#7483 = ORIENTED_EDGE ( 'NONE', *, *, #24063, .T. ) ;
#7484 = CARTESIAN_POINT ( 'NONE',  ( -15.75699695929680821, 10.73161574548146824, -1.384526174263989162E-13 ) ) ;
#7485 = EDGE_CURVE ( 'NONE', #15025, #16515, #21600, .T. ) ;
#7486 = CARTESIAN_POINT ( 'NONE',  ( 8.700000000289733748, -15.05693637256081097, -37.86809127166881694 ) ) ;
#7487 = CARTESIAN_POINT ( 'NONE',  ( -6.652733932600000344, -10.33873597240000031, 232.6627643349999914 ) ) ;
#7488 = CARTESIAN_POINT ( 'NONE',  ( -27.79999999999999716, -2.356928386389999887E-11, 224.8000000000000114 ) ) ;
#7489 = CARTESIAN_POINT ( 'NONE',  ( 23.56533302370000271, -14.74861233630000079, 224.4930104139999969 ) ) ;
#7490 = CARTESIAN_POINT ( 'NONE',  ( 10.69999999998770157, -129.0530586102001962, -36.95173408317435815 ) ) ;
#7491 = LINE ( 'NONE', #4667, #2651 ) ;
#7492 = CARTESIAN_POINT ( 'NONE',  ( -25.77914833258148164, -15.40383343755785361, 0.7595836940000044724 ) ) ;
#7493 = CARTESIAN_POINT ( 'NONE',  ( -8.523495769106718356, -15.81573655472489470, -74.63478688787961346 ) ) ;
#7494 = CARTESIAN_POINT ( 'NONE',  ( -20.77600556914587315, -21.68409854326995045, 8.000000000000007105 ) ) ;
#7495 = DIRECTION ( 'NONE',  ( -1.000000000000000000, -0.000000000000000000, 0.000000000000000000 ) ) ;
#7496 = TOROIDAL_SURFACE ( 'NONE', #6482, 24.50000000000000000, 4.000000000000000000 ) ;
#7497 = CARTESIAN_POINT ( 'NONE',  ( 8.751033282710258376, 8.359832557568292799, 232.0000002394078251 ) ) ;
#7498 = CARTESIAN_POINT ( 'NONE',  ( 10.69999999930000101, -120.5233595624000174, -31.26042064949999855 ) ) ;
#7499 = CARTESIAN_POINT ( 'NONE',  ( -16.83342759575507586, 10.99999999997565503, -0.6999999999999784173 ) ) ;
#7500 = ORIENTED_EDGE ( 'NONE', *, *, #5167, .T. ) ;
#7501 = CARTESIAN_POINT ( 'NONE',  ( 7.638687372290000610, 2.450513428906772706, -42.01217025054418741 ) ) ;
#7502 = VECTOR ( 'NONE', #3518, 1000.000000000000000 ) ;
#7503 = ORIENTED_EDGE ( 'NONE', *, *, #12189, .T. ) ;
#7504 = CARTESIAN_POINT ( 'NONE',  ( 24.39644993330914247, -14.73373303253482369, 224.0345656044051168 ) ) ;
#7505 = AXIS2_PLACEMENT_3D ( 'NONE', #24274, #7289, #21929 ) ;
#7506 = CARTESIAN_POINT ( 'NONE',  ( 5.235465350887244185, -2.882605534178610984, -58.78843849682499467 ) ) ;
#7507 = ORIENTED_EDGE ( 'NONE', *, *, #13732, .F. ) ;
#7508 = ADVANCED_FACE ( 'NONE', ( #20205 ), #18146, .F. ) ;
#7509 = VERTEX_POINT ( 'NONE', #17833 ) ;
#7510 = DIRECTION ( 'NONE',  ( 1.000000000000000000, -9.224647189900196894E-13, 4.710284450064082408E-12 ) ) ;
#7511 = EDGE_LOOP ( 'NONE', ( #28574, #28810, #13177, #4592 ) ) ;
#7512 = ORIENTED_EDGE ( 'NONE', *, *, #29999, .T. ) ;
#7513 = DIRECTION ( 'NONE',  ( 0.000000000000000000, 0.000000000000000000, -1.000000000000000000 ) ) ;
#7514 = CARTESIAN_POINT ( 'NONE',  ( -23.92481352202682388, 14.15879617723574313, 4.239732039000021047 ) ) ;
#7515 = DIRECTION ( 'NONE',  ( -2.416122857340496113E-12, 0.9341647027306024809, 0.3568421334038978099 ) ) ;
#7516 = DIRECTION ( 'NONE',  ( 0.000000000000000000, -1.000000000000000000, 0.000000000000000000 ) ) ;
#7517 = CARTESIAN_POINT ( 'NONE',  ( 0.5074138422395748638, -6.503547975687064664, -9.393384211799999051 ) ) ;
#7518 = DIRECTION ( 'NONE',  ( 0.000000000000000000, 0.000000000000000000, 1.000000000000000000 ) ) ;
#7519 = ORIENTED_EDGE ( 'NONE', *, *, #1726, .F. ) ;
#7520 = DIRECTION ( 'NONE',  ( 0.000000000000000000, 0.000000000000000000, 1.000000000000000000 ) ) ;
#7521 = EDGE_CURVE ( 'NONE', #28717, #11411, #23048, .T. ) ;
#7522 = CARTESIAN_POINT ( 'NONE',  ( -24.45473033751197178, -14.63622298155413226, 3.901342939999996595 ) ) ;
#7523 = CARTESIAN_POINT ( 'NONE',  ( -1.058439502263211374, 6.005994971325610443, -20.43583244400000609 ) ) ;
#7524 = CARTESIAN_POINT ( 'NONE',  ( 1.636264169893193676, 3.500000000000000000, 230.6345832158283145 ) ) ;
#7525 = VECTOR ( 'NONE', #25518, 1000.000000000000000 ) ;
#7526 = DIRECTION ( 'NONE',  ( -1.000000000000000000, 5.665498452320000818E-16, 0.000000000000000000 ) ) ;
#7527 = B_SPLINE_SURFACE_WITH_KNOTS ( 'NONE', 5, 1, ( 
 ( #24881, #27387 ),
 ( #5981, #8173 ),
 ( #22983, #3310 ),
 ( #25182, #22667 ),
 ( #1430, #11024 ),
 ( #30056, #29904 ),
 ( #15575, #30211 ),
 ( #3616, #22524 ),
 ( #8644, #13210 ),
 ( #18241, #27852 ),
 ( #22823, #20302 ),
 ( #20154, #8327 ),
 ( #1275, #10872 ),
 ( #17623, #7462 ),
 ( #7158, #12178 ) ),
 .UNSPECIFIED., .F., .F., .F.,
 ( 6, 3, 3, 3, 6 ),
 ( 2, 2 ),
 ( 0.000000000000000000, 0.5238999881950000548, 1.047799976390000110, 1.571699964580000053, 1.746333293980000034 ),
 ( -0.7000000000009999335, 2.555885125540000124E-06 ),
 .UNSPECIFIED. ) ;
#7528 = EDGE_CURVE ( 'NONE', #17102, #8971, #22579, .T. ) ;
#7529 = CARTESIAN_POINT ( 'NONE',  ( 8.903108651239925564, -22.82508830966962421, 90.00000000000000000 ) ) ;
#7530 = CARTESIAN_POINT ( 'NONE',  ( -15.83793381061078875, -8.512024964203421362, 0.000000000000000000 ) ) ;
#7531 = CARTESIAN_POINT ( 'NONE',  ( 0.7190444496327288437, -5.886645524263159679, -43.30057807742499421 ) ) ;
#7532 = ADVANCED_FACE ( 'NONE', ( #8705 ), #20574, .F. ) ;
#7533 = CARTESIAN_POINT ( 'NONE',  ( -10.69999999999999929, -121.6050280552999965, -31.36907097850000170 ) ) ;
#7534 = CARTESIAN_POINT ( 'NONE',  ( 0.000000000000000000, 0.000000000000000000, 227.6412452703700069 ) ) ;
#7535 = CARTESIAN_POINT ( 'NONE',  ( -24.07583586439999834, -13.90018868249999962, 223.9000014189999774 ) ) ;
#7536 = CARTESIAN_POINT ( 'NONE',  ( -24.81427761910000029, 13.76515143070000136, 229.2930779689999952 ) ) ;
#7537 = DIRECTION ( 'NONE',  ( 0.000000000000000000, 0.000000000000000000, 1.000000000000000000 ) ) ;
#7538 = EDGE_LOOP ( 'NONE', ( #26363, #5179, #12042, #19040 ) ) ;
#7539 = CARTESIAN_POINT ( 'NONE',  ( -5.414567903583902719, -1.055967702048432599, -32.09652066320001751 ) ) ;
#7540 = EDGE_CURVE ( 'NONE', #15618, #9281, #9697, .T. ) ;
#7541 = EDGE_LOOP ( 'NONE', ( #20407, #27603, #30587, #24429, #10139, #7647 ) ) ;
#7542 = CARTESIAN_POINT ( 'NONE',  ( 24.54884435356041905, -13.04717673660012522, 3.997190761000024573 ) ) ;
#7543 = CARTESIAN_POINT ( 'NONE',  ( -5.843148694310191793, 0.5835664591014033675, -48.42737393802499923 ) ) ;
#7544 = VERTEX_POINT ( 'NONE', #27439 ) ;
#7545 = ORIENTED_EDGE ( 'NONE', *, *, #4842, .T. ) ;
#7546 = AXIS2_PLACEMENT_3D ( 'NONE', #23981, #2273, #31057 ) ;
#7547 = ADVANCED_FACE ( 'NONE', ( #25410 ), #10284, .F. ) ;
#7548 = ORIENTED_EDGE ( 'NONE', *, *, #532, .T. ) ;
#7549 = CARTESIAN_POINT ( 'NONE',  ( -0.8738876050350000702, -27.78662806160000187, 224.3198333100000070 ) ) ;
#7550 = EDGE_LOOP ( 'NONE', ( #8499, #27577, #18166, #10679 ) ) ;
#7551 = CARTESIAN_POINT ( 'NONE',  ( 24.09856112909999837, -15.21545593799999985, 225.0000014190000002 ) ) ;
#7552 = EDGE_CURVE ( 'NONE', #20501, #23803, #29588, .T. ) ;
#7553 = FACE_OUTER_BOUND ( 'NONE', #18550, .T. ) ;
#7554 = CARTESIAN_POINT ( 'NONE',  ( 0.3780721272196958527, 4.308878343199122440, -35.69999999999999574 ) ) ;
#7555 = CARTESIAN_POINT ( 'NONE',  ( -12.67644879029220739, -27.23199623400657998, -22.76044039645793049 ) ) ;
#7556 = CARTESIAN_POINT ( 'NONE',  ( -3.751900487315417809, -0.8603159972124789778, -0.6999999999999994005 ) ) ;
#7557 = CARTESIAN_POINT ( 'NONE',  ( 0.000000000000000000, 0.000000000000000000, 227.6412452700500069 ) ) ;
#7558 = CARTESIAN_POINT ( 'NONE',  ( -10.69999999995908091, -34.38191890726957212, -24.27107665818032700 ) ) ;
#7559 = ORIENTED_EDGE ( 'NONE', *, *, #1230, .F. ) ;
#7560 = CARTESIAN_POINT ( 'NONE',  ( 0.2164205762250857590, 5.520452575866341860, -8.937690181099998910 ) ) ;
#7561 = CARTESIAN_POINT ( 'NONE',  ( 2.193772516446764076, 5.694542648089183423, -25.49462237480000582 ) ) ;
#7562 = CARTESIAN_POINT ( 'NONE',  ( 3.361572482953519625, 1.073845131765873484, 0.000000000000000000 ) ) ;
#7563 = CYLINDRICAL_SURFACE ( 'NONE', #2631, 1.099999999999998979 ) ;
#7564 = CARTESIAN_POINT ( 'NONE',  ( 23.81866173088643635, 14.33570044285385947, 6.099998581000020792 ) ) ;
#7565 = CARTESIAN_POINT ( 'NONE',  ( 5.654928157491471374, -26.91331636611315403, 20.79580928853452093 ) ) ;
#7566 = CARTESIAN_POINT ( 'NONE',  ( -4.180754675048095947, 1.217138862148074763, -16.30443125759999745 ) ) ;
#7567 = B_SPLINE_CURVE_WITH_KNOTS ( 'NONE', 3,
 ( #16350, #23287, #26115, #16195, #25960, #30369, #25809, #30527, #24177, #13843 ),
 .UNSPECIFIED., .F., .F.,
 ( 4, 2, 2, 2, 4 ),
 ( 0.000000000000000000, 0.2500000000000000000, 0.5000000000000000000, 0.7500000000000000000, 1.000000000000000000 ),
 .UNSPECIFIED. ) ;
#7568 = DIRECTION ( 'NONE',  ( 0.9880370573969197157, -0.1542166437529878531, -1.665334536939228724E-13 ) ) ;
#7569 = CARTESIAN_POINT ( 'NONE',  ( -24.43659368756648576, -14.66646236829179450, 3.899998581000013509 ) ) ;
#7570 = DIRECTION ( 'NONE',  ( 0.3633921898465292122, 0.9316362575375348731, -5.204170427930420494E-15 ) ) ;
#7571 = ORIENTED_EDGE ( 'NONE', *, *, #18210, .F. ) ;
#7572 = DIRECTION ( 'NONE',  ( 0.8923935798119907448, 1.018860921557044162E-12, 0.4512579070889951582 ) ) ;
#7573 = CARTESIAN_POINT ( 'NONE',  ( 10.32522729140000095, -2.500000000000002220, -1.399999999999998579 ) ) ;
#7574 = AXIS2_PLACEMENT_3D ( 'NONE', #10170, #10484, #8254 ) ;
#7575 = VERTEX_POINT ( 'NONE', #15334 ) ;
#7576 = DIRECTION ( 'NONE',  ( 0.000000000000000000, 0.000000000000000000, 1.000000000000000000 ) ) ;
#7577 = CARTESIAN_POINT ( 'NONE',  ( 3.861721477338985409, 1.529807325115373207, -38.22530605780803370 ) ) ;
#7578 = ADVANCED_FACE ( 'NONE', ( #8080 ), #23607, .T. ) ;
#7579 = ORIENTED_EDGE ( 'NONE', *, *, #24242, .F. ) ;
#7580 = DIRECTION ( 'NONE',  ( 1.000000000000000000, -1.224606353819999582E-16, 0.000000000000000000 ) ) ;
#7581 = EDGE_LOOP ( 'NONE', ( #5169, #26566, #29104, #30158, #25041, #10558, #14365, #10874 ) ) ;
#7582 = ORIENTED_EDGE ( 'NONE', *, *, #2074, .F. ) ;
#7583 = EDGE_CURVE ( 'NONE', #1757, #1312, #1330, .T. ) ;
#7584 = ORIENTED_EDGE ( 'NONE', *, *, #13774, .F. ) ;
#7585 = CARTESIAN_POINT ( 'NONE',  ( -17.49999999970000175, -28.83948587665830843, -30.80191174503961449 ) ) ;
#7586 = EDGE_CURVE ( 'NONE', #29101, #11584, #2481, .T. ) ;
#7587 = ADVANCED_FACE ( 'NONE', ( #11084 ), #23511, .F. ) ;
#7588 = CARTESIAN_POINT ( 'NONE',  ( 28.49528339128749366, 0.5184828350247753237, 8.000000000000007105 ) ) ;
#7589 = CARTESIAN_POINT ( 'NONE',  ( -7.999999999683340413, -17.27538706577754724, -33.40447746430434961 ) ) ;
#7590 = VERTEX_POINT ( 'NONE', #21459 ) ;
#7591 = LINE ( 'NONE', #21613, #19459 ) ;
#7592 = DIRECTION ( 'NONE',  ( 0.000000000000000000, 0.3420201433259318358, -0.9396926207858125046 ) ) ;
#7593 = CARTESIAN_POINT ( 'NONE',  ( 8.000000000276081380, -16.84112630282697154, -33.19732204816383359 ) ) ;
#7594 = CARTESIAN_POINT ( 'NONE',  ( 7.638687372242999984, -7.087249463098728164, -37.36029246609886911 ) ) ;
#7595 = ORIENTED_EDGE ( 'NONE', *, *, #22132, .F. ) ;
#7596 = AXIS2_PLACEMENT_3D ( 'NONE', #29083, #22014, #5015 ) ;
#7597 = CARTESIAN_POINT ( 'NONE',  ( -12.74757277634464003, 25.48862485138152678, -59.60122879067003510 ) ) ;
#7598 = CARTESIAN_POINT ( 'NONE',  ( -2.402234890526806499, 4.289919416549723863, -15.74011783620000671 ) ) ;
#7599 = FACE_BOUND ( 'NONE', #23703, .T. ) ;
#7600 = CARTESIAN_POINT ( 'NONE',  ( 27.23548387100000312, -1.776356839399999804E-15, 88.33953982530000815 ) ) ;
#7601 = CARTESIAN_POINT ( 'NONE',  ( -17.83931601609999973, 20.00000000000000000, 230.0000000010000178 ) ) ;
#7602 = CARTESIAN_POINT ( 'NONE',  ( 0.6090474298383116158, -27.79358669172298946, 3.904048352000033528 ) ) ;
#7603 = CARTESIAN_POINT ( 'NONE',  ( 27.06563795990000187, -3.314475221579999886E-15, 91.94026860140000679 ) ) ;
#7604 = CARTESIAN_POINT ( 'NONE',  ( 8.000000000651317222, -14.08431897228786411, -33.76897726028251157 ) ) ;
#7605 = CARTESIAN_POINT ( 'NONE',  ( -3.496762477156740268, 0.4822370985009253319, -0.6999999999999784173 ) ) ;
#7606 = CARTESIAN_POINT ( 'NONE',  ( 26.27730496000000215, 9.202811183099997905, 229.9172022029999880 ) ) ;
#7607 = CARTESIAN_POINT ( 'NONE',  ( -14.81011783459999975, -10.71728792430000077, 230.6999999999999886 ) ) ;
#7608 = ORIENTED_EDGE ( 'NONE', *, *, #14635, .F. ) ;
#7609 = CARTESIAN_POINT ( 'NONE',  ( -1.065285671501096765, -5.119323817795550902, -52.17706695232500635 ) ) ;
#7610 = CARTESIAN_POINT ( 'NONE',  ( -12.41634270788144789, -25.70200949929017753, -23.37589838086136496 ) ) ;
#7611 = CARTESIAN_POINT ( 'NONE',  ( -22.06913545133442511, 17.56725181239296774, 0.9999999989999952543 ) ) ;
#7612 = CARTESIAN_POINT ( 'NONE',  ( -4.829479218091812243, -1.221145322595682092, -68.10000000002503384 ) ) ;
#7613 = ORIENTED_EDGE ( 'NONE', *, *, #2961, .F. ) ;
#7614 = CARTESIAN_POINT ( 'NONE',  ( -0.5493605121539751890, 3.610303475240396409, -92.12187520236776095 ) ) ;
#7615 = B_SPLINE_SURFACE_WITH_KNOTS ( 'NONE', 5, 1, ( 
 ( #26610, #17464 ),
 ( #19845, #12290 ),
 ( #2842, #7263 ),
 ( #12435, #5196 ),
 ( #4901, #28967 ),
 ( #9931, #10241 ),
 ( #29119, #5050 ),
 ( #27070, #22054 ),
 ( #37, #10089 ),
 ( #15113, #26921 ),
 ( #19683, #29268 ),
 ( #5358, #14962 ),
 ( #24710, #16854 ),
 ( #654, #29426 ),
 ( #7860, #3146 ) ),
 .UNSPECIFIED., .F., .F., .F.,
 ( 6, 3, 3, 3, 6 ),
 ( 2, 2 ),
 ( 0.000000000000000000, 0.5239055192570000186, 1.047811038520000126, 1.571716557770000078, 1.746351730860000062 ),
 ( -0.7000000000009999335, 2.557314091049999969E-06 ),
 .UNSPECIFIED. ) ;
#7616 = EDGE_LOOP ( 'NONE', ( #10909, #17674, #6640, #1500 ) ) ;
#7617 = CARTESIAN_POINT ( 'NONE',  ( -1.421085471519999843E-14, -3.552713678799999608E-15, 186.3944487249999895 ) ) ;
#7618 = AXIS2_PLACEMENT_3D ( 'NONE', #5531, #22075, #982 ) ;
#7619 = LINE ( 'NONE', #17828, #9955 ) ;
#7620 = EDGE_LOOP ( 'NONE', ( #9636, #14828, #15973, #20165 ) ) ;
#7621 = CARTESIAN_POINT ( 'NONE',  ( -5.367600138796280618, 3.713494282865395402, -26.06779765530001214 ) ) ;
#7622 = DIRECTION ( 'NONE',  ( -1.000000000000000000, 1.853796481301025284E-24, -2.257144471330669991E-12 ) ) ;
#7623 = B_SPLINE_CURVE_WITH_KNOTS ( 'NONE', 5,
 ( #22976, #16045, #13526, #28158, #30203, #30833, #25810, #30528, #1580, #18231, #23138, #16351, #25657, #23609, #26116 ),
 .UNSPECIFIED., .F., .F.,
 ( 6, 3, 3, 3, 6 ),
 ( 0.000000000000000000, 0.1999999999996538436, 0.4000000000006923018, 0.6999999999986153965, 1.000000000000000000 ),
 .UNSPECIFIED. ) ;
#7624 = CARTESIAN_POINT ( 'NONE',  ( -4.300317018729668206, 2.364939115720630980, -59.81908057272499946 ) ) ;
#7625 = FACE_BOUND ( 'NONE', #22568, .T. ) ;
#7626 = CARTESIAN_POINT ( 'NONE',  ( -27.50000000000000000, 3.552713678799999608E-15, 193.6055512750000105 ) ) ;
#7627 = CARTESIAN_POINT ( 'NONE',  ( 10.80000000000790550, -15.94902145823636985, -35.53273252494371093 ) ) ;
#7628 = CARTESIAN_POINT ( 'NONE',  ( 3.511914029064534315, 0.9171864698412210970, 230.7613442533399279 ) ) ;
#7629 = CARTESIAN_POINT ( 'NONE',  ( -17.04621913067799710, -22.00000000000000000, -31.28675134614999820 ) ) ;
#7630 = VERTEX_POINT ( 'NONE', #6358 ) ;
#7631 = CARTESIAN_POINT ( 'NONE',  ( 14.65905325912865997, -31.99961021129703909, -26.55383800025211372 ) ) ;
#7632 = ADVANCED_FACE ( 'NONE', ( #20993 ), #25562, .F. ) ;
#7633 = DIRECTION ( 'NONE',  ( 1.000000000000000000, 0.000000000000000000, 0.000000000000000000 ) ) ;
#7634 = CARTESIAN_POINT ( 'NONE',  ( -11.95978252129999930, -1.610295041749999934, 231.9999989789999972 ) ) ;
#7635 = CARTESIAN_POINT ( 'NONE',  ( 28.49528339128749366, 0.5184828350247753237, 8.000000000000007105 ) ) ;
#7636 = TOROIDAL_SURFACE ( 'NONE', #19717, 24.50000000000000000, 3.200000000000000178 ) ;
#7637 = CARTESIAN_POINT ( 'NONE',  ( -24.09747192797636828, -13.86256885946331430, 4.035710821950520888 ) ) ;
#7638 = CARTESIAN_POINT ( 'NONE',  ( -5.897866114205988275, -30.56559748946277466, -80.00329722769471630 ) ) ;
#7639 = CARTESIAN_POINT ( 'NONE',  ( 3.205646567073016318, -2.709343606966754248, -0.6999999999999992895 ) ) ;
#7640 = CARTESIAN_POINT ( 'NONE',  ( -20.44304571761251665, -21.33658544107177590, -0.2432540810000105580 ) ) ;
#7641 = CARTESIAN_POINT ( 'NONE',  ( 2.774054804950544682E-10, -5.572998883585641217, -27.02754848644491403 ) ) ;
#7642 = LINE ( 'NONE', #10331, #4742 ) ;
#7643 = DIRECTION ( 'NONE',  ( -1.000000000000000000, 5.665498452320000818E-16, 0.000000000000000000 ) ) ;
#7644 = EDGE_CURVE ( 'NONE', #9163, #11537, #6683, .T. ) ;
#7645 = CARTESIAN_POINT ( 'NONE',  ( -23.81569860410000317, -13.75000000000000000, 6.099999999630000502 ) ) ;
#7646 = FACE_OUTER_BOUND ( 'NONE', #17212, .T. ) ;
#7647 = ORIENTED_EDGE ( 'NONE', *, *, #24998, .F. ) ;
#7648 = FACE_OUTER_BOUND ( 'NONE', #18452, .T. ) ;
#7649 = DIRECTION ( 'NONE',  ( 1.000000000000000000, 0.000000000000000000, 0.000000000000000000 ) ) ;
#7650 = CARTESIAN_POINT ( 'NONE',  ( 4.311559700750661861, -2.373910439939187267, -59.05843849682499780 ) ) ;
#7651 = ORIENTED_EDGE ( 'NONE', *, *, #1919, .F. ) ;
#7652 = CONTEXT_DEPENDENT_SHAPE_REPRESENTATION ( #16824, #11981 ) ;
#7653 = VERTEX_POINT ( 'NONE', #23522 ) ;
#7654 = CARTESIAN_POINT ( 'NONE',  ( -17.04621913067799710, -27.00000000059169736, -22.62649730796000114 ) ) ;
#7655 = ORIENTED_EDGE ( 'NONE', *, *, #6549, .F. ) ;
#7656 = ADVANCED_FACE ( 'NONE', ( #1956 ), #11550, .F. ) ;
#7657 = ORIENTED_EDGE ( 'NONE', *, *, #6169, .F. ) ;
#7658 = CARTESIAN_POINT ( 'NONE',  ( 23.20948082139999968, -13.40000000000000036, 223.8999999999999773 ) ) ;
#7659 = CARTESIAN_POINT ( 'NONE',  ( -22.90527192528401201, 16.36193184990112570, 1.000000000000000888 ) ) ;
#7660 = DIRECTION ( 'NONE',  ( -0.7071067811865475727, -0.7071067811865475727, 0.000000000000000000 ) ) ;
#7661 = CARTESIAN_POINT ( 'NONE',  ( 25.16696686177538567, -13.37570800333111087, 6.002806400000004317 ) ) ;
#7662 = CARTESIAN_POINT ( 'NONE',  ( 3.981471518793421538, 3.199610153647690414, -7.417086408000004738 ) ) ;
#7663 = CARTESIAN_POINT ( 'NONE',  ( -4.667733413567799694, -30.93201666733562405, 8.000000000000007105 ) ) ;
#7664 = EDGE_LOOP ( 'NONE', ( #26321, #30322, #26418, #23205 ) ) ;
#7665 = CARTESIAN_POINT ( 'NONE',  ( 0.7487076883252210546, -3.952114498550206800, -44.10000000002500542 ) ) ;
#7666 = CARTESIAN_POINT ( 'NONE',  ( -24.83401023410189623, -13.98326748962921329, 4.239871886000001311 ) ) ;
#7667 = CARTESIAN_POINT ( 'NONE',  ( -2.227024806490486508, -3.476280271252723431, -18.70544088819999118 ) ) ;
#7668 = CARTESIAN_POINT ( 'NONE',  ( -12.30731012795045842, -24.88828231266208846, -32.95456904492809258 ) ) ;
#7669 = CARTESIAN_POINT ( 'NONE',  ( -2.947640775130000104E-14, -27.50000000000000000, 226.0999999999999943 ) ) ;
#7670 = VECTOR ( 'NONE', #5549, 1000.000000000000000 ) ;
#7671 = FACE_OUTER_BOUND ( 'NONE', #28980, .T. ) ;
#7672 = CARTESIAN_POINT ( 'NONE',  ( -9.897162125297919388, -25.37356426550854138, 191.6604601750000256 ) ) ;
#7673 = CARTESIAN_POINT ( 'NONE',  ( -4.757978549728680839, 2.797812790916673897, -44.04354844312500461 ) ) ;
#7674 = EDGE_CURVE ( 'NONE', #18191, #5647, #8168, .T. ) ;
#7675 = DIRECTION ( 'NONE',  ( 0.000000000000000000, 0.000000000000000000, 1.000000000000000000 ) ) ;
#7676 = CARTESIAN_POINT ( 'NONE',  ( -7.861312627776432471, -9.716283825151744935, -32.74022090984056632 ) ) ;
#7677 = CARTESIAN_POINT ( 'NONE',  ( 8.699999999966381736, -117.4706889487312083, 13.80759369670018444 ) ) ;
#7678 = CARTESIAN_POINT ( 'NONE',  ( -26.78802611780000120, 9.366666170069999353, 229.2930777859999978 ) ) ;
#7679 = CARTESIAN_POINT ( 'NONE',  ( 6.438687372205746051, -7.245008774379918748, -33.94554228741176161 ) ) ;
#7680 = VERTEX_POINT ( 'NONE', #7593 ) ;
#7681 = CARTESIAN_POINT ( 'NONE',  ( 1.456545767631115096, -4.104408573385633474, -30.75632401680000072 ) ) ;
#7682 = ORIENTED_EDGE ( 'NONE', *, *, #13467, .T. ) ;
#7683 = ADVANCED_FACE ( 'NONE', ( #2420 ), #10275, .T. ) ;
#7684 = CARTESIAN_POINT ( 'NONE',  ( 25.41286869299526074, -12.90211872965451079, 4.492873455000018446 ) ) ;
#7685 = CARTESIAN_POINT ( 'NONE',  ( -1.909971040720825908, -5.612411004515823088, -47.47520033292499875 ) ) ;
#7686 = ORIENTED_EDGE ( 'NONE', *, *, #6579, .T. ) ;
#7687 = AXIS2_PLACEMENT_3D ( 'NONE', #9145, #23643, #9461 ) ;
#7688 = ORIENTED_EDGE ( 'NONE', *, *, #12089, .T. ) ;
#7689 = EDGE_CURVE ( 'NONE', #12087, #7467, #218, .T. ) ;
#7690 =( LENGTH_UNIT ( ) NAMED_UNIT ( * ) SI_UNIT ( .MILLI., .METRE. ) );
#7691 = AXIS2_PLACEMENT_3D ( 'NONE', #12605, #27236, #29284 ) ;
#7692 = ORIENTED_EDGE ( 'NONE', *, *, #9169, .T. ) ;
#7693 = CARTESIAN_POINT ( 'NONE',  ( -7.999999999727729794, -25.80029109889006023, -25.65030496461561071 ) ) ;
#7694 = ORIENTED_EDGE ( 'NONE', *, *, #9036, .F. ) ;
#7695 = VECTOR ( 'NONE', #11794, 1000.000000000000000 ) ;
#7696 = CARTESIAN_POINT ( 'NONE',  ( -11.57608395609999974, -24.17108566160000294, -0.7028182529999968953 ) ) ;
#7697 = CARTESIAN_POINT ( 'NONE',  ( 2.728640529172922768, 2.273855967875096695, 227.6754430268697718 ) ) ;
#7698 = CARTESIAN_POINT ( 'NONE',  ( 22.62517538422034136, 16.36045799713766158, 1.000000000000000888 ) ) ;
#7699 = FACE_OUTER_BOUND ( 'NONE', #8652, .T. ) ;
#7700 = EDGE_CURVE ( 'NONE', #9494, #11197, #29191, .T. ) ;
#7701 = CARTESIAN_POINT ( 'NONE',  ( -12.75378086759999796, -27.00000000059169736, -22.62649730796000114 ) ) ;
#7702 = CARTESIAN_POINT ( 'NONE',  ( -2.240416623506871208, -3.018983424413556715, -0.6999999999999992895 ) ) ;
#7703 = FACE_OUTER_BOUND ( 'NONE', #25157, .T. ) ;
#7704 = CARTESIAN_POINT ( 'NONE',  ( -10.69999999999999929, -43.95328087560000085, -27.24755286599999948 ) ) ;
#7705 = CARTESIAN_POINT ( 'NONE',  ( -4.602605444716575178, -1.443872896163948205, -10.96073088899999526 ) ) ;
#7706 = CARTESIAN_POINT ( 'NONE',  ( -3.231711866632715147, -5.662799918003592836, -30.67642233980000199 ) ) ;
#7707 = DIRECTION ( 'NONE',  ( -0.7071067811834158556, 0.6355433650310500227, -0.3099752105724556395 ) ) ;
#7708 = EDGE_CURVE ( 'NONE', #9708, #12147, #6493, .T. ) ;
#7709 = CARTESIAN_POINT ( 'NONE',  ( -14.94562240850000023, -8.628859120750000500, 225.0000000000000000 ) ) ;
#7710 = FACE_OUTER_BOUND ( 'NONE', #18304, .T. ) ;
#7711 = CARTESIAN_POINT ( 'NONE',  ( -28.50000000000000000, 1.776356839399999922E-14, 222.0000000000000000 ) ) ;
#7712 = CIRCLE ( 'NONE', #10724, 2.100000000000000089 ) ;
#7713 = CARTESIAN_POINT ( 'NONE',  ( 2.442787111560830837, -20.41832893614638067, -27.52048474490649355 ) ) ;
#7714 = CARTESIAN_POINT ( 'NONE',  ( -1.598721155459999804E-14, 0.000000000000000000, -0.6999999999999992895 ) ) ;
#7715 = VECTOR ( 'NONE', #3305, 1000.000000000000000 ) ;
#7716 = AXIS2_PLACEMENT_3D ( 'NONE', #6186, #23355, #1795 ) ;
#7717 = CARTESIAN_POINT ( 'NONE',  ( 1.379247882482921517, -27.76613141686462782, 5.680166690000016061 ) ) ;
#7718 = CARTESIAN_POINT ( 'NONE',  ( -24.66346748855670867, -14.28208995890320665, 3.997248602000014195 ) ) ;
#7719 = CARTESIAN_POINT ( 'NONE',  ( 0.8978302376563351839, -3.499838689521491464, 230.7708768453263701 ) ) ;
#7720 = ORIENTED_EDGE ( 'NONE', *, *, #25675, .F. ) ;
#7721 = EDGE_CURVE ( 'NONE', #25371, #19777, #7014, .T. ) ;
#7722 = CARTESIAN_POINT ( 'NONE',  ( 8.000000000241653808, -24.19750966826863348, -27.32947504231146851 ) ) ;
#7723 = CARTESIAN_POINT ( 'NONE',  ( -2.870505120338942007, -20.37236795256072597, -27.54290141440374384 ) ) ;
#7724 = ORIENTED_EDGE ( 'NONE', *, *, #9895, .T. ) ;
#7725 = FACE_OUTER_BOUND ( 'NONE', #1309, .T. ) ;
#7726 = CARTESIAN_POINT ( 'NONE',  ( -8.699999999693083907, -27.47644226430233871, -31.38783462183295114 ) ) ;
#7727 = VERTEX_POINT ( 'NONE', #12157 ) ;
#7728 = CARTESIAN_POINT ( 'NONE',  ( -4.529613163810471299, 1.007793355091292531, -44.10000000002500542 ) ) ;
#7729 = ORIENTED_EDGE ( 'NONE', *, *, #20770, .T. ) ;
#7730 = VERTEX_POINT ( 'NONE', #14847 ) ;
#7731 = VERTEX_POINT ( 'NONE', #10119 ) ;
#7732 = DIRECTION ( 'NONE',  ( 0.000000000000000000, -1.000000000000000000, 0.000000000000000000 ) ) ;
#7733 = VECTOR ( 'NONE', #22597, 1000.000000000000000 ) ;
#7734 = DIRECTION ( 'NONE',  ( 0.000000000000000000, 0.000000000000000000, 1.000000000000000000 ) ) ;
#7736 = CYLINDRICAL_SURFACE ( 'NONE', #18325, 4.276011752367103291 ) ;
#7735 = AXIS2_PLACEMENT_3D ( 'NONE', #29194, #22599, #22129 ) ;
#7737 = VECTOR ( 'NONE', #21598, 1000.000000000000000 ) ;
#7738 = ORIENTED_EDGE ( 'NONE', *, *, #13231, .F. ) ;
#7739 =( NAMED_UNIT ( * ) SI_UNIT ( $, .STERADIAN. ) SOLID_ANGLE_UNIT ( ) );
#7740 = CONICAL_SURFACE ( 'NONE', #30872, 1.303225372841144925, 0.9162978572969998625 ) ;
#7741 = CARTESIAN_POINT ( 'NONE',  ( 28.49528339128749366, 0.5184828350247835393, 8.000000000000007105 ) ) ;
#7742 = DIRECTION ( 'NONE',  ( 1.000000000000000000, 0.000000000000000000, 0.000000000000000000 ) ) ;
#7743 = CYLINDRICAL_SURFACE ( 'NONE', #24037, 2.000000000000003553 ) ;
#7744 = CARTESIAN_POINT ( 'NONE',  ( 2.131628207279999844E-14, 1.421085471519999843E-14, 230.7531949689999919 ) ) ;
#7745 = CARTESIAN_POINT ( 'NONE',  ( -3.057389860650357338, 5.459897439232808125, -16.67761783620000315 ) ) ;
#7746 = CARTESIAN_POINT ( 'NONE',  ( -17.93324555128263142, -9.020011618190519442, -0.6999999999999784173 ) ) ;
#7747 = EDGE_CURVE ( 'NONE', #24060, #9909, #30025, .T. ) ;
#7748 = CARTESIAN_POINT ( 'NONE',  ( -26.80000000069999899, 3.281945028329999726E-15, 143.2171415869999862 ) ) ;
#7749 = PRESENTATION_LAYER_ASSIGNMENT (  '', '', ( #10281 ) ) ;
#7750 = CARTESIAN_POINT ( 'NONE',  ( -24.41841039498785193, -14.69667350221323865, 6.099998581000020792 ) ) ;
#7751 = CARTESIAN_POINT ( 'NONE',  ( 26.63983911210000244, 10.51862255760000053, 222.0000000000000000 ) ) ;
#7752 = CARTESIAN_POINT ( 'NONE',  ( -24.46167596951645251, 13.21010012949721535, 3.927763967234794595 ) ) ;
#7753 = EDGE_CURVE ( 'NONE', #26866, #4633, #26309, .T. ) ;
#7754 = ADVANCED_FACE ( 'NONE', ( #15752 ), #12529, .T. ) ;
#7755 = CARTESIAN_POINT ( 'NONE',  ( -10.69999999999999929, -27.00000000000000000, -31.39999999999999858 ) ) ;
#7756 = CARTESIAN_POINT ( 'NONE',  ( 24.33692359859999854, 13.51547608080000096, 229.9171999149999692 ) ) ;
#7757 = DIRECTION ( 'NONE',  ( -1.224606353819999829E-16, -1.000000000000000000, 0.000000000000000000 ) ) ;
#7758 = AXIS2_PLACEMENT_3D ( 'NONE', #6485, #25698, #14364 ) ;
#7759 = ORIENTED_EDGE ( 'NONE', *, *, #12733, .F. ) ;
#7760 = CARTESIAN_POINT ( 'NONE',  ( 3.346097069831758919, -4.318458891484066697, -51.70430438132500228 ) ) ;
#7761 = CARTESIAN_POINT ( 'NONE',  ( -12.49429647964976375, -26.13498548490847284, -23.12598273097680845 ) ) ;
#7762 = AXIS2_PLACEMENT_3D ( 'NONE', #7499, #12068, #26544 ) ;
#7763 = VECTOR ( 'NONE', #23685, 1000.000000000000000 ) ;
#7764 = CONICAL_SURFACE ( 'NONE', #10780, 0.9999999999991012745, 0.7853981633970000820 ) ;
#7765 = CARTESIAN_POINT ( 'NONE',  ( -24.05392374927932053, 13.13253365033636477, 0.000000000000000000 ) ) ;
#7766 = CARTESIAN_POINT ( 'NONE',  ( -4.280718260511862994, 1.038266773289004075, -68.10000000002500542 ) ) ;
#7767 = VERTEX_POINT ( 'NONE', #8046 ) ;
#7768 = CARTESIAN_POINT ( 'NONE',  ( -3.458129700890608671, 0.5397582531265487926, -88.52261276240527366 ) ) ;
#7769 = ORIENTED_EDGE ( 'NONE', *, *, #24497, .T. ) ;
#7770 = FACE_OUTER_BOUND ( 'NONE', #2829, .T. ) ;
#7771 = AXIS2_PLACEMENT_3D ( 'NONE', #11283, #20886, #9064 ) ;
#7772 = CARTESIAN_POINT ( 'NONE',  ( 23.29312071241426096, 15.17488100587054767, 5.506989593000027661 ) ) ;
#7773 = ORIENTED_EDGE ( 'NONE', *, *, #16488, .F. ) ;
#7774 = CARTESIAN_POINT ( 'NONE',  ( -0.6320852424383932577, 6.069672320066970883, -26.48903409330001679 ) ) ;
#7775 = DIRECTION ( 'NONE',  ( 1.553705081258626668E-12, 0.7253743710120288402, -0.6883545756940265825 ) ) ;
#7776 = CARTESIAN_POINT ( 'NONE',  ( 4.406935161057896622, -1.569536819518615900, -67.23341453912500754 ) ) ;
#7777 = CARTESIAN_POINT ( 'NONE',  ( 26.80000000069999899, -3.281945028320000125E-15, 115.0000000010000036 ) ) ;
#7778 = AXIS2_PLACEMENT_3D ( 'NONE', #1196, #29672, #8102 ) ;
#7779 = CARTESIAN_POINT ( 'NONE',  ( -2.947640775130000104E-14, -27.50000000000000000, 223.8999999999999773 ) ) ;
#7780 = DIRECTION ( 'NONE',  ( 0.2815395311429191305, 0.9595496299847263710, 0.000000000000000000 ) ) ;
#7781 = ORIENTED_EDGE ( 'NONE', *, *, #20540, .F. ) ;
#7782 = UNCERTAINTY_MEASURE_WITH_UNIT (LENGTH_MEASURE( 1.000000000000000082E-05 ), #1485, 'distance_accuracy_value', 'NONE');
#7783 = CARTESIAN_POINT ( 'NONE',  ( -7.534632680830988249, -6.582071621271182060, -34.26887834115397169 ) ) ;
#7784 = CARTESIAN_POINT ( 'NONE',  ( -5.114250173089999407, -17.43050732989999929, 231.6999999999999886 ) ) ;
#7785 = ORIENTED_EDGE ( 'NONE', *, *, #4851, .F. ) ;
#7786 = CARTESIAN_POINT ( 'NONE',  ( 14.84835410051233850, -32.00028618471380071, -27.94962782489255915 ) ) ;
#7787 = CARTESIAN_POINT ( 'NONE',  ( -24.36130770023045145, -13.39283555876519749, 5.208359076000035337 ) ) ;
#7788 = CARTESIAN_POINT ( 'NONE',  ( -11.39200449410000004, 4.622831274389999301, 232.6627643349999914 ) ) ;
#7790 = EDGE_CURVE ( 'NONE', #14877, #25546, #24604, .T. ) ;
#7789 = CARTESIAN_POINT ( 'NONE',  ( -0.4860360036921328453, -0.1431275748294068006, -98.16700801147820243 ) ) ;
#7791 = CARTESIAN_POINT ( 'NONE',  ( -4.374602998565779721, 11.28407061768234954, 232.0000000000051443 ) ) ;
#7792 = CARTESIAN_POINT ( 'NONE',  ( 10.69999999998402274, -128.0799935798686136, -35.32105789699520670 ) ) ;
#7794 = B_SPLINE_CURVE_WITH_KNOTS ( 'NONE', 3,
 ( #24233, #7246, #16840, #26445, #28489, #335 ),
 .UNSPECIFIED., .F., .F.,
 ( 4, 2, 4 ),
 ( 0.000000000000000000, 0.5000000000000000000, 1.000000000000000000 ),
 .UNSPECIFIED. ) ;
#7793 = CARTESIAN_POINT ( 'NONE',  ( 2.392384901021629151, -3.229711410377742453, -0.6999999999999992895 ) ) ;
#7795 = CARTESIAN_POINT ( 'NONE',  ( -26.79556473285982321, -0.4875557887251147915, -0.6999999999999784173 ) ) ;
#7797 = ADVANCED_FACE ( 'NONE', ( #22686 ), #29457, .F. ) ;
#7796 = CARTESIAN_POINT ( 'NONE',  ( 0.2897533057796581324, -27.49881094941897786, 3.928609959452268097 ) ) ;
#7798 = CIRCLE ( 'NONE', #9303, 3.200000000000002398 ) ;
#7799 = CARTESIAN_POINT ( 'NONE',  ( -15.86808677770000209, -9.527368092500001495, -0.7999999992999995424 ) ) ;
#7800 = CARTESIAN_POINT ( 'NONE',  ( -10.69999999895494192, -27.00000000000000000, -28.40000000000000213 ) ) ;
#7801 = CARTESIAN_POINT ( 'NONE',  ( -7.121574564636396154, -25.83919502053029404, 21.93648921904840776 ) ) ;
#7802 = CARTESIAN_POINT ( 'NONE',  ( -0.5575288593801756010, -27.79459983365108044, 5.310182064000024127 ) ) ;
#7803 = ORIENTED_EDGE ( 'NONE', *, *, #17109, .F. ) ;
#7804 = CARTESIAN_POINT ( 'NONE',  ( 24.50000001620000134, -3.000285568839999855E-15, 139.9999999960000139 ) ) ;
#7805 = CARTESIAN_POINT ( 'NONE',  ( 24.10986967230000033, -13.84040926149999962, 226.0986570600000221 ) ) ;
#7806 = CARTESIAN_POINT ( 'NONE',  ( -5.296314592117303377, -2.692763687817543161, -62.36424626872499033 ) ) ;
#7807 = EDGE_LOOP ( 'NONE', ( #14174, #9599, #8681, #24455 ) ) ;
#7808 = ITEM_DEFINED_TRANSFORMATION ( 'NONE', 'NONE', #20357,  #17722 ) ;
#7809 = VERTEX_POINT ( 'NONE', #988 ) ;
#7810 = CARTESIAN_POINT ( 'NONE',  ( -11.08346179031913437, -28.41490585489481191, 93.60555127549999099 ) ) ;
#7811 = ORIENTED_EDGE ( 'NONE', *, *, #7552, .T. ) ;
#7812 = AXIS2_PLACEMENT_3D ( 'NONE', #23620, #30142, #20870 ) ;
#7813 = VERTEX_POINT ( 'NONE', #15140 ) ;
#7814 = PLANE ( 'NONE',  #4003 ) ;
#7815 = EDGE_CURVE ( 'NONE', #9796, #21330, #6002, .T. ) ;
#7816 = LINE ( 'NONE', #16798, #442 ) ;
#7817 = CARTESIAN_POINT ( 'NONE',  ( -21.30888436558564081, -16.34772642260385211, 143.2171415880000040 ) ) ;
#7818 = CARTESIAN_POINT ( 'NONE',  ( 11.98808650430000000, -2.924528239270000274, 232.6627648150000027 ) ) ;
#7819 = FACE_OUTER_BOUND ( 'NONE', #14104, .T. ) ;
#7820 = CARTESIAN_POINT ( 'NONE',  ( -5.857861475075242019, -1.837656413297739766, -10.02323088899999881 ) ) ;
#7821 = CARTESIAN_POINT ( 'NONE',  ( 26.80000000000000071, -6.039613253960000872E-14, 230.6999999999999886 ) ) ;
#7822 = ORIENTED_EDGE ( 'NONE', *, *, #782, .F. ) ;
#7823 = CARTESIAN_POINT ( 'NONE',  ( 2.130274636608692873, -3.629988127160616695, -44.10000000002499121 ) ) ;
#7824 = CARTESIAN_POINT ( 'NONE',  ( 24.92639507930385889, 13.81781707913292934, 4.493023686000019445 ) ) ;
#7825 = CARTESIAN_POINT ( 'NONE',  ( 5.972505199797514486, -1.290950946386169917, -24.39036215650000727 ) ) ;
#7826 = CARTESIAN_POINT ( 'NONE',  ( 27.73177268570753640, 2.208741748110918390, 8.000000000000007105 ) ) ;
#7827 = CARTESIAN_POINT ( 'NONE',  ( -6.000000000000000000, -15.86465192213301556, -74.65259062561435144 ) ) ;
#7828 = CARTESIAN_POINT ( 'NONE',  ( -24.07583586439999834, -13.90018868249999962, 226.1000014189999945 ) ) ;
#7829 = CARTESIAN_POINT ( 'NONE',  ( -5.162912894389027230, 3.035924517800103750, -44.84354844312500177 ) ) ;
#7830 = CARTESIAN_POINT ( 'NONE',  ( -10.69999999999999929, -120.7100010810000015, -31.27129587090000129 ) ) ;
#7831 = CARTESIAN_POINT ( 'NONE',  ( 7.000000000281329626, -5.981227587276792157, -27.94042817480899288 ) ) ;
#7832 = CARTESIAN_POINT ( 'NONE',  ( -19.41565715145875615, 19.99999633038200741, 230.3176857765022874 ) ) ;
#7833 = CARTESIAN_POINT ( 'NONE',  ( -24.79654435811118063, -10.16723671460306910, 43.21714158839818509 ) ) ;
#7834 = CARTESIAN_POINT ( 'NONE',  ( -1.887507898140760254, 0.9307262473892381482, 226.6412452697800290 ) ) ;
#7835 = ORIENTED_EDGE ( 'NONE', *, *, #14700, .F. ) ;
#7836 = CARTESIAN_POINT ( 'NONE',  ( 0.7775660777938816492, 5.461502024334397909, -30.00600711720000291 ) ) ;
#7837 = ORIENTED_EDGE ( 'NONE', *, *, #29448, .T. ) ;
#7838 = CARTESIAN_POINT ( 'NONE',  ( 24.34137756859324853, -13.42980563341176037, 3.899998581000013509 ) ) ;
#7839 = CARTESIAN_POINT ( 'NONE',  ( 4.942443250116775211, -2.327596941721505441, -53.09872167392499875 ) ) ;
#7840 = VERTEX_POINT ( 'NONE', #22389 ) ;
#7841 = ORIENTED_EDGE ( 'NONE', *, *, #20220, .F. ) ;
#7842 = EDGE_CURVE ( 'NONE', #14782, #28608, #20171, .T. ) ;
#7843 = APPLICATION_PROTOCOL_DEFINITION ( 'draft international standard', 'automotive_design', 1998, #943 ) ;
#7844 = VERTEX_POINT ( 'NONE', #29762 ) ;
#7845 = ORIENTED_EDGE ( 'NONE', *, *, #8063, .F. ) ;
#7846 = CARTESIAN_POINT ( 'NONE',  ( 23.74337837439999888, -14.46065164910000078, 225.9012998019999827 ) ) ;
#7847 = CARTESIAN_POINT ( 'NONE',  ( -20.77600556904588913, -21.68409854326813146, 1.000000000000000888 ) ) ;
#7848 = EDGE_CURVE ( 'NONE', #2098, #18252, #17261, .T. ) ;
#7849 = CARTESIAN_POINT ( 'NONE',  ( 21.28666574344908469, 18.00484885041732142, 8.000000000000007105 ) ) ;
#7850 = DIRECTION ( 'NONE',  ( 0.000000000000000000, 0.000000000000000000, -1.000000000000000000 ) ) ;
#7851 = B_SPLINE_CURVE_WITH_KNOTS ( 'NONE', 3,
 ( #22432, #12361, #726, #21970, #424, #10006, #19913, #10473, #29659, #17680, #27296, #15644, #11244 ),
 .UNSPECIFIED., .F., .F.,
 ( 4, 2, 2, 1, 2, 2, 4 ),
 ( 0.000000000000000000, 0.2500000000000028866, 0.3750000000000024980, 0.4375000000000026090, 0.4687500000000026645, 0.5000000000000027756, 1.000000000000000000 ),
 .UNSPECIFIED. ) ;
#7852 = CARTESIAN_POINT ( 'NONE',  ( -4.861312627796364083, -15.07597047387718092, -33.46393288818136824 ) ) ;
#7853 = CARTESIAN_POINT ( 'NONE',  ( -3.832152770726432678, 2.440039442800121083, -0.6999999999999992895 ) ) ;
#7854 = CARTESIAN_POINT ( 'NONE',  ( -1.392415278799817635, -4.107851135794773789, -0.5756305127000010957 ) ) ;
#7855 = CARTESIAN_POINT ( 'NONE',  ( -10.69999999996523243, -41.43563524454161495, -26.99587756277172090 ) ) ;
#7856 = CARTESIAN_POINT ( 'NONE',  ( 1.348918213770420316, 4.124136235849971577, -11.57047964829999742 ) ) ;
#7857 = CARTESIAN_POINT ( 'NONE',  ( 3.473119624653126181, -3.299750202710006963, -29.11376389020000133 ) ) ;
#7858 = FACE_OUTER_BOUND ( 'NONE', #27854, .T. ) ;
#7859 = B_SPLINE_CURVE_WITH_KNOTS ( 'NONE', 4,
 ( #17051, #26650, #7604, #24451, #28701 ),
 .UNSPECIFIED., .F., .F.,
 ( 5, 5 ),
 ( -0.9817477042469999748, 0.9817477042469999748 ),
 .UNSPECIFIED. ) ;
#7860 = CARTESIAN_POINT ( 'NONE',  ( 24.93720649360215802, -13.79881813812812297, 6.099998581000020792 ) ) ;
#7861 = ADVANCED_FACE ( 'NONE', ( #29923 ), #3634, .F. ) ;
#7862 = CARTESIAN_POINT ( 'NONE',  ( 18.03085807409719621, 20.00000000003992540, -0.6999999999999784173 ) ) ;
#7863 = CARTESIAN_POINT ( 'NONE',  ( -2.625702655398183261, -2.452149595275970206, 227.6997972603546998 ) ) ;
#7864 = CARTESIAN_POINT ( 'NONE',  ( 14.85000000009999788, -29.39592972815999872, -32.78571994937999534 ) ) ;
#7865 = CARTESIAN_POINT ( 'NONE',  ( -1.782928038406565774, 3.983823234458339080, -22.73780126169999605 ) ) ;
#7866 = EDGE_CURVE ( 'NONE', #11539, #30733, #12750, .T. ) ;
#7867 = DIRECTION ( 'NONE',  ( -0.9915824307782121760, -0.1294769592320275942, 4.045530494348897360E-18 ) ) ;
#7868 = CARTESIAN_POINT ( 'NONE',  ( 14.76223730231795273, -25.56820193551933329, -23.45324323474691042 ) ) ;
#7869 = FACE_OUTER_BOUND ( 'NONE', #8109, .T. ) ;
#7870 = ORIENTED_EDGE ( 'NONE', *, *, #3586, .F. ) ;
#7871 = DIRECTION ( 'NONE',  ( 0.8775825618903718706, -0.4794255386042047262, 0.000000000000000000 ) ) ;
#7872 = CARTESIAN_POINT ( 'NONE',  ( 27.23548386990000125, -3.335274659639999982E-15, 141.6604601740000078 ) ) ;
#7873 = EDGE_LOOP ( 'NONE', ( #28910, #14518, #12384, #30578 ) ) ;
#7874 = CARTESIAN_POINT ( 'NONE',  ( 1.484924240490000047, 1.484924240490000047, 226.6412452697800006 ) ) ;
#7875 = CARTESIAN_POINT ( 'NONE',  ( 0.5057536231481327693, -27.79562098839016571, 3.899998581000013509 ) ) ;
#7876 = ORIENTED_EDGE ( 'NONE', *, *, #18737, .T. ) ;
#7877 = CARTESIAN_POINT ( 'NONE',  ( -4.670117344778931034, 0.7466779630707167659, -44.10000000002499121 ) ) ;
#7878 = ORIENTED_EDGE ( 'NONE', *, *, #380, .F. ) ;
#7879 = ORIENTED_EDGE ( 'NONE', *, *, #18098, .T. ) ;
#7880 = SURFACE_SIDE_STYLE ('',( #29290 ) ) ;
#7881 = ORIENTED_EDGE ( 'NONE', *, *, #26927, .F. ) ;
#7882 = CARTESIAN_POINT ( 'NONE',  ( 13.67718073920000066, 21.70000000000000284, -57.16242423349999768 ) ) ;
#7883 = EDGE_CURVE ( 'NONE', #8486, #902, #8006, .T. ) ;
#7884 = DIRECTION ( 'NONE',  ( 1.224606353819999829E-16, 1.000000000000000000, 0.000000000000000000 ) ) ;
#7885 = CARTESIAN_POINT ( 'NONE',  ( -7.999999999653060634, -17.20645473190809227, -37.69618843468767722 ) ) ;
#7886 = ORIENTED_EDGE ( 'NONE', *, *, #21521, .T. ) ;
#7887 = CARTESIAN_POINT ( 'NONE',  ( -20.30396346370000060, 20.00000000000000000, 227.0000000000000000 ) ) ;
#7888 = B_SPLINE_CURVE_WITH_KNOTS ( 'NONE', 1,
 ( #23150, #18569 ),
 .UNSPECIFIED., .F., .F.,
 ( 2, 2 ),
 ( -4.314404719430000596E-12, 0.7012472868949999327 ),
 .UNSPECIFIED. ) ;
#7889 = DIRECTION ( 'NONE',  ( 1.000000000000000000, 0.000000000000000000, 0.000000000000000000 ) ) ;
#7890 = DIRECTION ( 'NONE',  ( -1.000000000000000000, 0.000000000000000000, 0.000000000000000000 ) ) ;
#7891 = CARTESIAN_POINT ( 'NONE',  ( 23.51325844009999955, -14.83130343779999905, 224.7916311099999973 ) ) ;
#7892 = ORIENTED_EDGE ( 'NONE', *, *, #24020, .T. ) ;
#7893 = EDGE_CURVE ( 'NONE', #5070, #27866, #28531, .T. ) ;
#7894 = AXIS2_PLACEMENT_3D ( 'NONE', #19632, #24661, #3095 ) ;
#7895 = CARTESIAN_POINT ( 'NONE',  ( 27.23548387180000319, -3.335274659869999873E-15, 41.66046017409999536 ) ) ;
#7896 = CARTESIAN_POINT ( 'NONE',  ( -4.873044981369978323, 1.499374375125315684, -21.38539663400000634 ) ) ;
#7897 = CARTESIAN_POINT ( 'NONE',  ( -0.2873368412495915791, -28.49911791804343153, 223.9262120796962563 ) ) ;
#7898 = AXIS2_PLACEMENT_3D ( 'NONE', #18699, #1571, #28298 ) ;
#7899 = DIRECTION ( 'NONE',  ( 0.7071067811868757547, -0.6804000508938797820, -0.1924987551729659130 ) ) ;
#7900 = CARTESIAN_POINT ( 'NONE',  ( -4.884981308350000102E-15, -2.100000000000000089, 226.6412452697800006 ) ) ;
#7901 = ADVANCED_FACE ( 'NONE', ( #13873 ), #16535, .T. ) ;
#7902 = CARTESIAN_POINT ( 'NONE',  ( 9.999999999979998222, -27.00000000000000000, -31.39999999999999858 ) ) ;
#7903 = CARTESIAN_POINT ( 'NONE',  ( -23.53263993751885153, -14.22965940645031324, 224.0404533955600073 ) ) ;
#7904 = CARTESIAN_POINT ( 'NONE',  ( -3.529820002201436324, 0.01646793492178095022, -0.6999999999999783062 ) ) ;
#7905 = ADVANCED_FACE ( 'NONE', ( #28495 ), #1916, .T. ) ;
#7906 = CARTESIAN_POINT ( 'NONE',  ( -11.06030392579999955, -24.60936423849999954, -1.629296567100001258 ) ) ;
#7907 = CARTESIAN_POINT ( 'NONE',  ( 23.24663841809999809, -14.69162354060000020, 225.0000000000000000 ) ) ;
#7908 = ORIENTED_EDGE ( 'NONE', *, *, #2133, .F. ) ;
#7909 = CARTESIAN_POINT ( 'NONE',  ( -4.385510522250850585, 2.177216032694683445, -56.04877225282501030 ) ) ;
#7910 = CARTESIAN_POINT ( 'NONE',  ( -12.39067510636454728, -25.55074214220865514, -23.46327875140281094 ) ) ;
#7911 = PRODUCT_DEFINITION ( 'UNKNOWN', '', #29425, #26674 ) ;
#7912 = CARTESIAN_POINT ( 'NONE',  ( -24.87718597855597125, 13.58193782283921536, 0.5514320120000304470 ) ) ;
#7913 = CARTESIAN_POINT ( 'NONE',  ( -4.223277344473779671, 0.7255220498998576906, -68.10000000002501963 ) ) ;
#7914 = VERTEX_POINT ( 'NONE', #25989 ) ;
#7915 = VECTOR ( 'NONE', #20512, 1000.000000000000000 ) ;
#7916 = CARTESIAN_POINT ( 'NONE',  ( -3.376316311743029708, -1.036715029292714529, -96.83838116384302452 ) ) ;
#7917 = CIRCLE ( 'NONE', #2899, 2.999999999999999112 ) ;
#7918 = EDGE_LOOP ( 'NONE', ( #9437, #4379, #17329, #12179 ) ) ;
#7919 = CARTESIAN_POINT ( 'NONE',  ( 17.16657240420000008, 10.97998838177520931, -1.452769935612311825 ) ) ;
#7920 = ADVANCED_FACE ( 'NONE', ( #4428 ), #6938, .F. ) ;
#7921 = B_SPLINE_CURVE_WITH_KNOTS ( 'NONE', 1,
 ( #20413, #921 ),
 .UNSPECIFIED., .F., .F.,
 ( 2, 2 ),
 ( 1.500000000000000000, 3.500000000000000000 ),
 .UNSPECIFIED. ) ;
#7922 = CARTESIAN_POINT ( 'NONE',  ( -7.999999999985950794, -116.8591659214701792, 11.34031266722930908 ) ) ;
#7923 = VERTEX_POINT ( 'NONE', #30232 ) ;
#7924 = CARTESIAN_POINT ( 'NONE',  ( -5.973670867983248201, -0.3179945487330332332, -65.08421022022500324 ) ) ;
#7925 = CARTESIAN_POINT ( 'NONE',  ( -13.47758776899999944, -27.06128935389999768, 229.9172011129999760 ) ) ;
#7926 = EDGE_CURVE ( 'NONE', #7386, #20468, #7, .T. ) ;
#7927 = CARTESIAN_POINT ( 'NONE',  ( -28.58473218748631339, 4.397531023511127124, 0.7595836940000044724 ) ) ;
#7928 = CARTESIAN_POINT ( 'NONE',  ( -24.34663841809999951, -12.78636765230000094, 5.000000000000000000 ) ) ;
#7929 = DIRECTION ( 'NONE',  ( 0.9316362575375356503, 0.3633921898465274913, 0.000000000000000000 ) ) ;
#7930 = EDGE_CURVE ( 'NONE', #30214, #68, #1604, .T. ) ;
#7931 = CARTESIAN_POINT ( 'NONE',  ( -4.861278087196373221, -17.82179692228118384, -28.78689802532309372 ) ) ;
#7932 = MECHANICAL_DESIGN_GEOMETRIC_PRESENTATION_REPRESENTATION (  '', ( #19498 ), #5423 ) ;
#7933 = ORIENTED_EDGE ( 'NONE', *, *, #22913, .F. ) ;
#7934 = CARTESIAN_POINT ( 'NONE',  ( 24.74993095443131352, -14.13250376055072266, 3.957489350000009676 ) ) ;
#7935 = CARTESIAN_POINT ( 'NONE',  ( 18.31087175629999919, 19.88197256460000162, 229.9783849850000195 ) ) ;
#7936 = VERTEX_POINT ( 'NONE', #5350 ) ;
#7937 = CARTESIAN_POINT ( 'NONE',  ( 14.83997978847352783, -31.99986765628636576, -28.84563171583047492 ) ) ;
#7938 = CARTESIAN_POINT ( 'NONE',  ( -24.36724936496760918, -13.38201651699120021, 4.999998581000003384 ) ) ;
#7939 = CARTESIAN_POINT ( 'NONE',  ( -22.97723753882890918, 16.89265275057793403, 7.000000021000013284 ) ) ;
#7940 = VECTOR ( 'NONE', #23938, 1000.000000000000000 ) ;
#7941 = CARTESIAN_POINT ( 'NONE',  ( 26.80000000000000071, -1.776356839399999804E-15, 143.2171415880000040 ) ) ;
#7942 = CARTESIAN_POINT ( 'NONE',  ( -7.107063564515523346, -25.84129680694969267, 208.0588908682941565 ) ) ;
#7943 = CARTESIAN_POINT ( 'NONE',  ( 3.043036374812654099, -2.823920995556914004, -0.6999999999999992895 ) ) ;
#7944 = AXIS2_PLACEMENT_3D ( 'NONE', #20207, #29958, #22890 ) ;
#7945 = CARTESIAN_POINT ( 'NONE',  ( 13.73773747404255552, -26.37022765825810922, -0.6999999999999784173 ) ) ;
#7946 = CARTESIAN_POINT ( 'NONE',  ( 0.9895645837522295540, -27.48220350653630817, 4.514327848603801208 ) ) ;
#7947 = DIRECTION ( 'NONE',  ( 0.000000000000000000, 0.3420201433259318913, -0.9396926207858126157 ) ) ;
#7948 = CYLINDRICAL_SURFACE ( 'NONE', #569, 27.50000000000000000 ) ;
#7949 = CARTESIAN_POINT ( 'NONE',  ( -24.76171951330574927, -10.25169584067251094, 93.21714158839991171 ) ) ;
#7950 = CARTESIAN_POINT ( 'NONE',  ( 0.2722179827725955126, -28.49915599500044650, 6.079792140000011891 ) ) ;
#7951 = VERTEX_POINT ( 'NONE', #24401 ) ;
#7952 = CARTESIAN_POINT ( 'NONE',  ( 8.700000000244115128, -26.99999999999395328, -28.39999999994493862 ) ) ;
#7953 = PRESENTATION_STYLE_ASSIGNMENT (( #5754 ) ) ;
#7954 = CARTESIAN_POINT ( 'NONE',  ( -9.000000000000000000, -55.00000000000000000, -44.10000000000000142 ) ) ;
#7955 = CARTESIAN_POINT ( 'NONE',  ( -6.999999999884560786, -60.75400889059761766, -3.446705952697758590 ) ) ;
#7956 = EDGE_CURVE ( 'NONE', #9016, #7923, #5188, .T. ) ;
#7957 = AXIS2_PLACEMENT_3D ( 'NONE', #15435, #29600, #18250 ) ;
#7958 = CARTESIAN_POINT ( 'NONE',  ( 0.9016190905398319133, 4.836326944446648568, -64.17744533512500027 ) ) ;
#7959 = ORIENTED_EDGE ( 'NONE', *, *, #11817, .F. ) ;
#7960 = ORIENTED_EDGE ( 'NONE', *, *, #22021, .T. ) ;
#7961 = EDGE_CURVE ( 'NONE', #12226, #7590, #6888, .T. ) ;
#7963 = CARTESIAN_POINT ( 'NONE',  ( 27.52676963214367944, 0.5008603480904590954, 0.2686740700000300741 ) ) ;
#7962 = AXIS2_PLACEMENT_3D ( 'NONE', #23102, #6406, #4204 ) ;
#7964 = EDGE_CURVE ( 'NONE', #7840, #8976, #16877, .T. ) ;
#7965 = VERTEX_POINT ( 'NONE', #26450 ) ;
#7966 = ORIENTED_EDGE ( 'NONE', *, *, #17591, .F. ) ;
#7967 = CARTESIAN_POINT ( 'NONE',  ( -23.45048833551293654, -12.97319122232136479, 225.9951937281581706 ) ) ;
#7968 = CARTESIAN_POINT ( 'NONE',  ( -19.80535357367646654, 19.50875577052770993, 8.000000000000007105 ) ) ;
#7969 = CARTESIAN_POINT ( 'NONE',  ( -10.99999999969999998, 20.99999999999999645, -67.09999999999999432 ) ) ;
#7970 = CARTESIAN_POINT ( 'NONE',  ( -24.49999999589999788, 3.000285566369999841E-15, 140.0000000000000000 ) ) ;
#7971 = CARTESIAN_POINT ( 'NONE',  ( -0.6521609807820000215, -27.79292263629999837, 224.0990923460000204 ) ) ;
#7972 = ORIENTED_EDGE ( 'NONE', *, *, #840, .T. ) ;
#7973 = CARTESIAN_POINT ( 'NONE',  ( 2.219048841976018593, -3.599394683114398585, -44.10000000002499121 ) ) ;
#7974 = LINE ( 'NONE', #918, #27845 ) ;
#7975 = AXIS2_PLACEMENT_3D ( 'NONE', #18820, #16000, #13796 ) ;
#7976 = CARTESIAN_POINT ( 'NONE',  ( -4.430040892179064826, 1.363067613765865937, -22.82289663400000279 ) ) ;
#7977 = CARTESIAN_POINT ( 'NONE',  ( 23.73992238018677270, -12.43607998452291064, 4.902940994718408163 ) ) ;
#7978 = DIRECTION ( 'NONE',  ( -0.9316362575375349842, 0.3633921898465292122, -0.000000000000000000 ) ) ;
#7979 = FILL_AREA_STYLE_COLOUR ( '', #24199 ) ;
#7980 = CARTESIAN_POINT ( 'NONE',  ( -0.1113126268018901771, -2.615810859419198664, -36.20335296945926018 ) ) ;
#7981 = CARTESIAN_POINT ( 'NONE',  ( 2.137930486642451555, 6.059703978454344941, -45.49079303332499791 ) ) ;
#7982 = CARTESIAN_POINT ( 'NONE',  ( 0.000000000000000000, 0.000000000000000000, 40.00000000000000000 ) ) ;
#7983 = CARTESIAN_POINT ( 'NONE',  ( 8.966526567020551397, -25.25634759429104292, 205.5763919674312206 ) ) ;
#7984 = CARTESIAN_POINT ( 'NONE',  ( -18.15901341782211276, 19.99997668335234735, 230.6866300220142421 ) ) ;
#7985 = VECTOR ( 'NONE', #24944, 1000.000000000000114 ) ;
#7986 = DIRECTION ( 'NONE',  ( 0.000000000000000000, 0.000000000000000000, -1.000000000000000000 ) ) ;
#7987 = CIRCLE ( 'NONE', #30635, 3.000000000000001332 ) ;
#7988 = ADVANCED_FACE ( 'NONE', ( #2384 ), #18712, .F. ) ;
#7989 = EDGE_CURVE ( 'NONE', #18476, #21685, #8615, .T. ) ;
#7990 = CARTESIAN_POINT ( 'NONE',  ( -10.89131017139999891, -2.500000000000002220, -1.811764705899998606 ) ) ;
#7991 = VERTEX_POINT ( 'NONE', #30520 ) ;
#7992 = CARTESIAN_POINT ( 'NONE',  ( -4.346598770676711965, -0.007247149673127636568, -28.66856466010000304 ) ) ;
#7993 = ORIENTED_EDGE ( 'NONE', *, *, #7930, .F. ) ;
#7994 = DIRECTION ( 'NONE',  ( 0.000000000000000000, 0.000000000000000000, 1.000000000000000000 ) ) ;
#7995 = CARTESIAN_POINT ( 'NONE',  ( 0.6613659943794023555, -4.850238491497668392, -49.76468436622499780 ) ) ;
#7996 = ORIENTED_EDGE ( 'NONE', *, *, #6362, .F. ) ;
#7997 = EDGE_LOOP ( 'NONE', ( #5760, #17935, #24723, #4487 ) ) ;
#7998 = DIRECTION ( 'NONE',  ( 1.000000000000000000, 0.000000000000000000, 0.000000000000000000 ) ) ;
#7999 = ORIENTED_EDGE ( 'NONE', *, *, #29496, .T. ) ;
#8000 = ORIENTED_EDGE ( 'NONE', *, *, #21687, .T. ) ;
#8001 = CARTESIAN_POINT ( 'NONE',  ( 24.62873585949999722, -14.34148440729999940, 226.0959678990000157 ) ) ;
#8002 = CARTESIAN_POINT ( 'NONE',  ( -4.785279987089964493, -31.71089578132167119, 1.000000000000000888 ) ) ;
#8003 = DIRECTION ( 'NONE',  ( -1.000000000000000000, 0.000000000000000000, 0.000000000000000000 ) ) ;
#8004 = CYLINDRICAL_SURFACE ( 'NONE', #1399, 1.999999999999999334 ) ;
#8005 = VECTOR ( 'NONE', #11432, 1000.000000000000000 ) ;
#8006 = CIRCLE ( 'NONE', #10516, 3.200000000000000178 ) ;
#8007 = DIRECTION ( 'NONE',  ( -2.764840495839172918E-12, -0.9128796883888953273, 0.4082287037029530552 ) ) ;
#8008 = CARTESIAN_POINT ( 'NONE',  ( -21.81244463630000396, 17.27887638289999828, 224.0000000000000000 ) ) ;
#8009 = CARTESIAN_POINT ( 'NONE',  ( -3.983623483853893088, 2.386763808281609389, -0.6999999999999992895 ) ) ;
#8010 = PLANE ( 'NONE',  #18248 ) ;
#8011 = DIRECTION ( 'NONE',  ( -1.000000000000000000, 0.000000000000000000, 0.000000000000000000 ) ) ;
#8012 = CARTESIAN_POINT ( 'NONE',  ( -19.80535357367646654, 19.50875577052770993, 3.000000106999994642 ) ) ;
#8013 = CARTESIAN_POINT ( 'NONE',  ( 6.034652528523337445, 2.501332855249893683, -11.49261350020000449 ) ) ;
#8014 = CARTESIAN_POINT ( 'NONE',  ( 3.157381476932438868, -2.999772911539577702, -30.05126389020000488 ) ) ;
#8015 = CLOSED_SHELL ( 'NONE', ( #24255, #27972, #27471, #13113, #3078, #26307, #2196, #19760, #19880 ) ) ;
#8016 = DIRECTION ( 'NONE',  ( 0.000000000000000000, 0.000000000000000000, -1.000000000000000000 ) ) ;
#8017 = EDGE_CURVE ( 'NONE', #24648, #7844, #17925, .T. ) ;
#8018 = CARTESIAN_POINT ( 'NONE',  ( 18.41918092979155119, 20.00000737198188716, -0.6632381549999954995 ) ) ;
#8019 = CARTESIAN_POINT ( 'NONE',  ( -7.747305753407632167, -7.605135679882327970, -37.10770248100441648 ) ) ;
#8020 = CARTESIAN_POINT ( 'NONE',  ( 27.79539923781684507, 0.5057481689249235801, 8.000000000000007105 ) ) ;
#8021 = CARTESIAN_POINT ( 'NONE',  ( 2.450607853129164848, -3.579122932049590755, -27.13292313650000764 ) ) ;
#8022 = ADVANCED_FACE ( 'NONE', ( #3921 ), #2880, .F. ) ;
#8023 = CARTESIAN_POINT ( 'NONE',  ( 0.5746121234326042604, -27.79431838510023312, 6.098651075000017130 ) ) ;
#8024 = CARTESIAN_POINT ( 'NONE',  ( 8.000000000229924524, -28.07052495763006661, -25.59750966822355522 ) ) ;
#8025 = CARTESIAN_POINT ( 'NONE',  ( -0.5944614571882205212, -27.79380703160649446, 4.999998581000003384 ) ) ;
#8026 = EDGE_LOOP ( 'NONE', ( #29944, #22146, #23630, #24667 ) ) ;
#8027 = ADVANCED_FACE ( 'NONE', ( #30194 ), #23600, .T. ) ;
#8028 = CARTESIAN_POINT ( 'NONE',  ( 7.105427357599999217E-15, 8.881784197000000993E-16, 227.7662452697800006 ) ) ;
#8029 = DIRECTION ( 'NONE',  ( 0.000000000000000000, -2.257157423930000049E-12, -1.000000000000000000 ) ) ;
#8030 = VERTEX_POINT ( 'NONE', #28457 ) ;
#8031 = PLANE ( 'NONE',  #13839 ) ;
#8032 = CARTESIAN_POINT ( 'NONE',  ( -5.861312627756135818, -5.597492073868338025, -34.74908987245776615 ) ) ;
#8033 = VERTEX_POINT ( 'NONE', #2036 ) ;
#8034 = CARTESIAN_POINT ( 'NONE',  ( -0.2892551163132154324, -26.79878419087592789, 3.928509618683601712 ) ) ;
#8035 = ORIENTED_EDGE ( 'NONE', *, *, #26211, .T. ) ;
#8036 = ORIENTED_EDGE ( 'NONE', *, *, #27582, .F. ) ;
#8037 = VERTEX_POINT ( 'NONE', #9099 ) ;
#8038 = CARTESIAN_POINT ( 'NONE',  ( 16.89916710682537371, -10.07620797776944777, -0.000000000000000000 ) ) ;
#8039 = CARTESIAN_POINT ( 'NONE',  ( -1.065814103639999922E-14, 1.421085471519999843E-14, 186.3944487249999895 ) ) ;
#8040 = EDGE_CURVE ( 'NONE', #4224, #18028, #23130, .T. ) ;
#8041 = DIRECTION ( 'NONE',  ( 0.000000000000000000, 0.000000000000000000, -1.000000000000000000 ) ) ;
#8042 = CARTESIAN_POINT ( 'NONE',  ( 26.05511440549999946, -14.93230011260000012, 222.0000000000000000 ) ) ;
#8043 = CARTESIAN_POINT ( 'NONE',  ( -24.32472894358752313, 13.45989150749028873, 6.099998581000020792 ) ) ;
#8044 = AXIS2_PLACEMENT_3D ( 'NONE', #22963, #25647, #8466 ) ;
#8045 = CARTESIAN_POINT ( 'NONE',  ( -14.60916135985672071, 28.04296594682689658, 1.000000000000000888 ) ) ;
#8046 = CARTESIAN_POINT ( 'NONE',  ( -18.00000000000000000, 3.980648276280000204E-15, 229.6412452697800006 ) ) ;
#8047 = EDGE_CURVE ( 'NONE', #14390, #13946, #28920, .T. ) ;
#8048 = CARTESIAN_POINT ( 'NONE',  ( -7.999999999657077865, -13.50174601094418669, -36.11802512054224223 ) ) ;
#8049 = B_SPLINE_CURVE_WITH_KNOTS ( 'NONE', 5,
 ( #4038, #13636, #18508, #23241, #10809, #28110, #6548, #25284, #11434, #16145, #30638, #9063, #20403, #29990, #15672, #13317, #8424, #22928, #1369, #10964, #219 ),
 .UNSPECIFIED., .F., .F.,
 ( 6, 3, 3, 3, 3, 3, 6 ),
 ( -15.54987830269999982, -12.96130453750000022, -10.36904362289999959, -7.776782722830000161, -5.184521831730000585, -2.592260920730000251, 0.000000000000000000 ),
 .UNSPECIFIED. ) ;
#8050 = CARTESIAN_POINT ( 'NONE',  ( 5.003468744149685676, 2.348385630676867564, -3.479170051700001043 ) ) ;
#8051 = CARTESIAN_POINT ( 'NONE',  ( 5.516020573121914516, 0.1374401492888292498, -19.67661200060000226 ) ) ;
#8052 = CARTESIAN_POINT ( 'NONE',  ( 0.000000000000000000, -130.0000000000000000, -44.10000000000000142 ) ) ;
#8053 = CARTESIAN_POINT ( 'NONE',  ( -0.8790545793981902056, -27.48597397712025980, 5.665333839370780389 ) ) ;
#8054 = CARTESIAN_POINT ( 'NONE',  ( -17.79876841479999783, 11.52736809289999620, -1.399999999999998579 ) ) ;
#8055 = CARTESIAN_POINT ( 'NONE',  ( -22.19203486339999998, 17.78346196859999750, 230.2432540810000319 ) ) ;
#8056 = DIRECTION ( 'NONE',  ( -1.000000000000000000, 0.000000000000000000, 0.000000000000000000 ) ) ;
#8057 = CARTESIAN_POINT ( 'NONE',  ( 0.01646793492177278315, 3.529820002201416784, -0.6999999999999783062 ) ) ;
#8058 = CARTESIAN_POINT ( 'NONE',  ( 13.33996102200000244, -12.49969090709999975, 230.6999999999999886 ) ) ;
#8059 = CARTESIAN_POINT ( 'NONE',  ( 23.56630063259553864, -14.17280417119362035, 224.0051167707288755 ) ) ;
#8060 = VERTEX_POINT ( 'NONE', #8788 ) ;
#8061 = CARTESIAN_POINT ( 'NONE',  ( -2.158984558600606007, 5.217364672555318883, -57.14652090042499566 ) ) ;
#8062 = CARTESIAN_POINT ( 'NONE',  ( 9.738910687886932038, -24.96785170200595161, 193.2171415880000040 ) ) ;
#8063 = EDGE_CURVE ( 'NONE', #28983, #14390, #24415, .T. ) ;
#8064 = CARTESIAN_POINT ( 'NONE',  ( 4.190083271651539043, -3.954132654223795562, -18.03565260999999964 ) ) ;
#8065 = B_SPLINE_CURVE_WITH_KNOTS ( 'NONE', 5,
 ( #5511, #17765, #14966, #10244, #3302, #22515, #10397, #809, #19988 ),
 .UNSPECIFIED., .F., .F.,
 ( 6, 3, 6 ),
 ( 8.011061266649999624, 9.372199858680000162, 10.73333845069999981 ),
 .UNSPECIFIED. ) ;
#8066 = CARTESIAN_POINT ( 'NONE',  ( -4.499842235593497719, -29.81936866046843093, -0.6999999999999784173 ) ) ;
#8067 = CARTESIAN_POINT ( 'NONE',  ( -4.217110537010221982, 0.6683951208602848526, -68.10000000002500542 ) ) ;
#8068 = ORIENTED_EDGE ( 'NONE', *, *, #30535, .T. ) ;
#8069 = ORIENTED_EDGE ( 'NONE', *, *, #3136, .T. ) ;
#8070 = CARTESIAN_POINT ( 'NONE',  ( 1.609514238142041975, 3.181902231760902477, -88.52261276241718235 ) ) ;
#8071 = ORIENTED_EDGE ( 'NONE', *, *, #20909, .T. ) ;
#8072 = CARTESIAN_POINT ( 'NONE',  ( -11.50543609154933300, 21.00000000000056488, -55.48449806767045800 ) ) ;
#8073 = CARTESIAN_POINT ( 'NONE',  ( 23.39354070784786543, 15.01969649483752001, 5.760134169000008519 ) ) ;
#8074 = EDGE_CURVE ( 'NONE', #9436, #30789, #4385, .T. ) ;
#8075 = CARTESIAN_POINT ( 'NONE',  ( -4.919493655976348023, -0.2618778636732672083, -64.81421022022499301 ) ) ;
#8076 = CARTESIAN_POINT ( 'NONE',  ( -18.29999999989999893, -29.81628579456999972, -29.19678346420899828 ) ) ;
#8077 = ADVANCED_FACE ( 'NONE', ( #22965 ), #3384, .F. ) ;
#8078 = AXIS2_PLACEMENT_3D ( 'NONE', #24490, #15353, #7643 ) ;
#8079 = CARTESIAN_POINT ( 'NONE',  ( -27.17149341551030162, 9.183264753288028714, -0.2432540810000105580 ) ) ;
#8080 = FACE_OUTER_BOUND ( 'NONE', #10097, .T. ) ;
#8081 =( NAMED_UNIT ( * ) SI_UNIT ( $, .STERADIAN. ) SOLID_ANGLE_UNIT ( ) );
#8082 = DIRECTION ( 'NONE',  ( -0.8090169943751909232, 0.5877852522921378498, 0.000000000000000000 ) ) ;
#8083 = ORIENTED_EDGE ( 'NONE', *, *, #4894, .T. ) ;
#8084 = UNCERTAINTY_MEASURE_WITH_UNIT (LENGTH_MEASURE( 1.000000000000000082E-05 ), #18925, 'distance_accuracy_value', 'NONE');
#8085 = EDGE_CURVE ( 'NONE', #27430, #30479, #27023, .T. ) ;
#8086 = CARTESIAN_POINT ( 'NONE',  ( 0.8784916548508220346, -26.78562594433358868, 5.666076087045988530 ) ) ;
#8087 = CARTESIAN_POINT ( 'NONE',  ( 14.84775334008999970, -29.39779533080000107, -32.78913491209999620 ) ) ;
#8088 = ORIENTED_EDGE ( 'NONE', *, *, #7409, .F. ) ;
#8089 = CARTESIAN_POINT ( 'NONE',  ( 8.699999999944495244, -116.0414483704658579, 19.89613934358818170 ) ) ;
#8090 = CARTESIAN_POINT ( 'NONE',  ( -22.78981481891096550, -14.10205219198089388, 4.262772992854607423 ) ) ;
#8091 = FACE_OUTER_BOUND ( 'NONE', #15434, .T. ) ;
#8092 = CARTESIAN_POINT ( 'NONE',  ( -3.378474373710000034, -11.51459555979999827, 232.0000000000000000 ) ) ;
#8093 = CARTESIAN_POINT ( 'NONE',  ( -23.32129337776675015, -14.57293380274186134, 4.443835645165135517 ) ) ;
#8094 = CARTESIAN_POINT ( 'NONE',  ( 0.6576816962115121790, -3.783751283609423144, -0.6999999999999992895 ) ) ;
#8095 = EDGE_CURVE ( 'NONE', #8882, #6309, #1383, .T. ) ;
#8096 = CARTESIAN_POINT ( 'NONE',  ( -28.49528339128749366, -0.5184828350247674411, 1.000000000000000888 ) ) ;
#8097 = CARTESIAN_POINT ( 'NONE',  ( -23.50695179570000093, -14.84192241259999889, 225.0000014190000002 ) ) ;
#8098 = ORIENTED_EDGE ( 'NONE', *, *, #27878, .T. ) ;
#8099 = CARTESIAN_POINT ( 'NONE',  ( 28.49999999959999641, 10.47094317839999889, 229.0000000000000000 ) ) ;
#8100 = AXIS2_PLACEMENT_3D ( 'NONE', #28036, #28504, #9146 ) ;
#8101 = CARTESIAN_POINT ( 'NONE',  ( -8.730899654840367674, -25.33966640892204580, 23.96123044120707846 ) ) ;
#8102 = DIRECTION ( 'NONE',  ( -0.6941258031311203780, -0.7198537139083029945, 0.000000000000000000 ) ) ;
#8103 = VERTEX_POINT ( 'NONE', #6742 ) ;
#8104 = ADVANCED_FACE ( 'NONE', ( #25951 ), #27830, .T. ) ;
#8105 = CARTESIAN_POINT ( 'NONE',  ( 11.51411768920000078, -24.20066399999999973, -0.7084723288000027708 ) ) ;
#8106 = CARTESIAN_POINT ( 'NONE',  ( -11.69999999989999928, 19.99999999999999645, -2.399999999999999467 ) ) ;
#8107 = CARTESIAN_POINT ( 'NONE',  ( -24.35939747514432696, 11.38309468199551766, -0.6999999999999992895 ) ) ;
#8108 = CARTESIAN_POINT ( 'NONE',  ( 0.8372177269581373427, 4.490875019823951320, -63.82744533512499885 ) ) ;
#8109 = EDGE_LOOP ( 'NONE', ( #15872, #29321, #20673, #25855 ) ) ;
#8110 = ORIENTED_EDGE ( 'NONE', *, *, #6355, .T. ) ;
#8111 = CARTESIAN_POINT ( 'NONE',  ( 22.88013437149966833, -19.49504814935155039, 0.02487579700000130956 ) ) ;
#8112 = ORIENTED_EDGE ( 'NONE', *, *, #11935, .F. ) ;
#8113 = DIRECTION ( 'NONE',  ( 5.962915006522623408E-16, 0.4383711467890811231, 0.8987940462991652613 ) ) ;
#8114 = CARTESIAN_POINT ( 'NONE',  ( 25.46368747440213198, -12.80129684534102807, 4.999998581000003384 ) ) ;
#8115 = LINE ( 'NONE', #20102, #27002 ) ;
#8116 = B_SPLINE_CURVE_WITH_KNOTS ( 'NONE', 3,
 ( #9415, #11937, #21545, #26571, #16808, #26422, #5011, #21860, #11631, #11787, #23606, #4864 ),
 .UNSPECIFIED., .F., .F.,
 ( 4, 2, 2, 2, 2, 4 ),
 ( 0.000000000000000000, 0.2499999999999725775, 0.4999999999999451550, 0.6249999999999481526, 0.7499999999999512612, 1.000000000000000000 ),
 .UNSPECIFIED. ) ;
#8117 = CARTESIAN_POINT ( 'NONE',  ( -27.62819771675075486, 4.248502122600195996, 8.000000000000007105 ) ) ;
#8118 = B_SPLINE_CURVE_WITH_KNOTS ( 'NONE', 3,
 ( #3114, #3421, #27490, #928, #26889, #13022 ),
 .UNSPECIFIED., .F., .F.,
 ( 4, 2, 4 ),
 ( 0.000000000000000000, 0.5000000000000000000, 1.000000000000000000 ),
 .UNSPECIFIED. ) ;
#8119 = CYLINDRICAL_SURFACE ( 'NONE', #891, 1.099999999999999867 ) ;
#8120 = LINE ( 'NONE', #24822, #24573 ) ;
#8121 = ORIENTED_EDGE ( 'NONE', *, *, #19217, .F. ) ;
#8122 = CARTESIAN_POINT ( 'NONE',  ( 1.927687739761373198, -3.697324211539649852, -44.10000000002500542 ) ) ;
#8123 = CARTESIAN_POINT ( 'NONE',  ( 0.3233900739386466605, 6.101867874933233793, -23.54418644580000120 ) ) ;
#8124 = CARTESIAN_POINT ( 'NONE',  ( -12.48413792322910965, -22.90323034870550600, -31.80782553739934571 ) ) ;
#8125 = CARTESIAN_POINT ( 'NONE',  ( -12.30000000006999805, -24.00000000000000000, -28.40000000020000215 ) ) ;
#8126 = EDGE_CURVE ( 'NONE', #30938, #10989, #13138, .T. ) ;
#8127 = SURFACE_SIDE_STYLE ('',( #10826 ) ) ;
#8128 = CARTESIAN_POINT ( 'NONE',  ( 10.45000000009999930, -29.81704525737000111, -27.60590580922099946 ) ) ;
#8129 = CARTESIAN_POINT ( 'NONE',  ( -2.577814338686791107, 4.205191132749348526, -44.30531229042500740 ) ) ;
#8130 = ADVANCED_FACE ( 'NONE', ( #11159 ), #7212, .F. ) ;
#8131 = DIRECTION ( 'NONE',  ( 0.000000000000000000, 0.000000000000000000, -1.000000000000000000 ) ) ;
#8132 = EDGE_CURVE ( 'NONE', #18237, #18212, #28507, .T. ) ;
#8133 = CARTESIAN_POINT ( 'NONE',  ( 3.674376064820728427, -26.54820124389934577, 209.8046840415867109 ) ) ;
#8134 = CARTESIAN_POINT ( 'NONE',  ( 10.99999999979999998, 21.69999999919999212, -70.09999999999999432 ) ) ;
#8135 = CARTESIAN_POINT ( 'NONE',  ( -27.71720220739999974, -1.978379369349999957E-11, 229.4485730569999760 ) ) ;
#8136 = CARTESIAN_POINT ( 'NONE',  ( -2.045530030620520634, 0.5496038860227483447, 226.6412452697800575 ) ) ;
#8137 = ORIENTED_EDGE ( 'NONE', *, *, #21170, .T. ) ;
#8138 = PRODUCT_DEFINITION_SHAPE ( 'NONE', 'NONE',  #31122 ) ;
#8139 = CARTESIAN_POINT ( 'NONE',  ( -0.3280975466111932248, 4.681158999438244983, -34.89518930510001127 ) ) ;
#8140 = ORIENTED_EDGE ( 'NONE', *, *, #28038, .T. ) ;
#8141 = DIRECTION ( 'NONE',  ( 0.000000000000000000, 0.000000000000000000, 1.000000000000000000 ) ) ;
#8142 = CARTESIAN_POINT ( 'NONE',  ( 4.172426907288941500, -2.584475198598515266, -50.08324460762499797 ) ) ;
#8143 = ORIENTED_EDGE ( 'NONE', *, *, #15472, .T. ) ;
#8144 = ORIENTED_EDGE ( 'NONE', *, *, #9999, .F. ) ;
#8145 = DIRECTION ( 'NONE',  ( 0.3359158147882104206, 0.5818232582787822293, -0.7407038959672308520 ) ) ;
#8146 = B_SPLINE_CURVE_WITH_KNOTS ( 'NONE', 3,
 ( #15640, #19909, #5578, #25251, #29655, #5733 ),
 .UNSPECIFIED., .F., .F.,
 ( 4, 2, 4 ),
 ( 0.000000000000000000, 0.5000000000000000000, 1.000000000000000000 ),
 .UNSPECIFIED. ) ;
#8147 = VERTEX_POINT ( 'NONE', #28922 ) ;
#8148 = CIRCLE ( 'NONE', #19226, 1.000000000000000888 ) ;
#8149 = ORIENTED_EDGE ( 'NONE', *, *, #12638, .T. ) ;
#8150 = CARTESIAN_POINT ( 'NONE',  ( 17.16657240420000008, 12.45283507331071426, -1.972246272986471594 ) ) ;
#8151 = DIRECTION ( 'NONE',  ( 0.000000000000000000, 1.000000000000000000, 0.000000000000000000 ) ) ;
#8152 = PLANE ( 'NONE',  #8407 ) ;
#8153 = CARTESIAN_POINT ( 'NONE',  ( 8.000000000659929000, -16.02040192323402223, -38.09843960558792730 ) ) ;
#8154 = DIRECTION ( 'NONE',  ( 1.000000000000000000, 0.000000000000000000, 0.000000000000000000 ) ) ;
#8155 = CARTESIAN_POINT ( 'NONE',  ( -3.942867718245478770, 0.7271718878511516104, -0.6999999999999992895 ) ) ;
#8156 = DIRECTION ( 'NONE',  ( 0.000000000000000000, 0.000000000000000000, 1.000000000000000000 ) ) ;
#8157 = AXIS2_PLACEMENT_3D ( 'NONE', #4832, #28735, #28590 ) ;
#8158 = CARTESIAN_POINT ( 'NONE',  ( -3.427383197786517677, -1.063472793697235241, 227.6973195743569249 ) ) ;
#8159 = DIRECTION ( 'NONE',  ( 0.7071067811870476172, 0.000000000000000000, -0.7071067811860475283 ) ) ;
#8160 = CARTESIAN_POINT ( 'NONE',  ( 3.665953941183818010, 4.858601989977915814, -14.22796858840000311 ) ) ;
#8161 = CARTESIAN_POINT ( 'NONE',  ( 1.456545767631115096, -4.104408573385633474, -29.75632401680000427 ) ) ;
#8162 = DIRECTION ( 'NONE',  ( 1.635844237846128888E-12, -0.6889064844606307414, -0.7248502298186121351 ) ) ;
#8163 = CARTESIAN_POINT ( 'NONE',  ( -10.69999999989999928, 19.99999999999999645, -2.399999999999999467 ) ) ;
#8164 = CARTESIAN_POINT ( 'NONE',  ( -6.999999999891231006, -60.06002009430259392, -1.894810482436639409 ) ) ;
#8165 = CARTESIAN_POINT ( 'NONE',  ( -7.800204957127538030, -115.2761342570987466, 21.60753225385484200 ) ) ;
#8166 = CARTESIAN_POINT ( 'NONE',  ( 1.882647771056455976, 3.960165260869605408, -32.15113063600000487 ) ) ;
#8167 = FACE_OUTER_BOUND ( 'NONE', #26322, .T. ) ;
#8168 = B_SPLINE_CURVE_WITH_KNOTS ( 'NONE', 1,
 ( #26483, #4927 ),
 .UNSPECIFIED., .F., .F.,
 ( 2, 2 ),
 ( -9.355471259890000464E-07, 0.7003637394550000783 ),
 .UNSPECIFIED. ) ;
#8169 = DIRECTION ( 'NONE',  ( 0.000000000000000000, 2.257145581549999994E-12, 1.000000000000000000 ) ) ;
#8170 = CARTESIAN_POINT ( 'NONE',  ( 19.80526555962148549, 19.50877392102342256, 1.000000000000000888 ) ) ;
#8171 = ADVANCED_FACE ( 'NONE', ( #9882 ), #20991, .T. ) ;
#8172 = ORIENTED_EDGE ( 'NONE', *, *, #25238, .T. ) ;
#8173 = CARTESIAN_POINT ( 'NONE',  ( 23.23277125981546476, 15.26692728828886025, 5.104183903999998329 ) ) ;
#8174 = CARTESIAN_POINT ( 'NONE',  ( 2.687036963354079155, 2.345727656310530485, 230.7977248921758928 ) ) ;
#8175 = ORIENTED_EDGE ( 'NONE', *, *, #29212, .F. ) ;
#8176 = AXIS2_PLACEMENT_3D ( 'NONE', #15127, #24578, #667 ) ;
#8177 = B_SPLINE_CURVE_WITH_KNOTS ( 'NONE', 3,
 ( #17233, #6165, #15766, #25380, #3817, #13404 ),
 .UNSPECIFIED., .F., .F.,
 ( 4, 2, 4 ),
 ( 0.000000000000000000, 0.5000000000000000000, 1.000000000000000000 ),
 .UNSPECIFIED. ) ;
#8178 = CARTESIAN_POINT ( 'NONE',  ( -7.999999999694088260, -25.22378963202354996, -30.84934466693886534 ) ) ;
#8179 = CARTESIAN_POINT ( 'NONE',  ( -8.699999999693680763, -27.86541989007905329, -31.29929855357051949 ) ) ;
#8181 = ORIENTED_EDGE ( 'NONE', *, *, #22299, .F. ) ;
#8180 = CIRCLE ( 'NONE', #22775, 27.69999999999999929 ) ;
#8182 = CARTESIAN_POINT ( 'NONE',  ( -8.095177325567840754, -26.28419651245281585, 22.67157132346132187 ) ) ;
#8183 = VERTEX_POINT ( 'NONE', #14612 ) ;
#8184 = VERTEX_POINT ( 'NONE', #4543 ) ;
#8185 = ORIENTED_EDGE ( 'NONE', *, *, #18082, .T. ) ;
#8186 = CARTESIAN_POINT ( 'NONE',  ( 27.04041630560000087, 4.566211381850000528, 230.6999999999999886 ) ) ;
#8187 = CARTESIAN_POINT ( 'NONE',  ( -16.85343921394901301, 12.09981795542885585, -0.6999999999999784173 ) ) ;
#8188 = CARTESIAN_POINT ( 'NONE',  ( -7.999999999657623206, -18.06128338792058230, -36.89507724070023897 ) ) ;
#8189 = ORIENTED_EDGE ( 'NONE', *, *, #6739, .T. ) ;
#8190 = SURFACE_STYLE_FILL_AREA ( #3632 ) ;
#8191 = CARTESIAN_POINT ( 'NONE',  ( -0.3775595308337927891, -28.49777658967324356, 5.680150179000031940 ) ) ;
#8192 = CARTESIAN_POINT ( 'NONE',  ( 3.928578988383309323, -27.21916582938554541, 209.8062029264887656 ) ) ;
#8193 = CARTESIAN_POINT ( 'NONE',  ( -0.3831792618880000556, -28.49793954440000121, 226.0423263479999889 ) ) ;
#8194 = VERTEX_POINT ( 'NONE', #4857 ) ;
#8196 = ADVANCED_FACE ( 'NONE', ( #12393 ), #12940, .T. ) ;
#8195 = AXIS2_PLACEMENT_3D ( 'NONE', #27683, #20610, #12910 ) ;
#8197 = CARTESIAN_POINT ( 'NONE',  ( 3.123710955063065509, -2.074832491810036039, -0.4587547302000010707 ) ) ;
#8198 = CARTESIAN_POINT ( 'NONE',  ( -2.942059828035410440, -4.605008556695580957, -20.70891267849999906 ) ) ;
#8199 = AXIS2_PLACEMENT_3D ( 'NONE', #13140, #29822, #20388 ) ;
#8200 = DIRECTION ( 'NONE',  ( -1.000000000000000000, 0.000000000000000000, 0.000000000000000000 ) ) ;
#8201 = LINE ( 'NONE', #24749, #22074 ) ;
#8202 = CARTESIAN_POINT ( 'NONE',  ( 1.125778434080668244, -3.298781954526681215, -90.35662574872537789 ) ) ;
#8203 = CARTESIAN_POINT ( 'NONE',  ( -18.17096239019999970, 20.37181511190000194, 230.6577119970000069 ) ) ;
#8204 = DIRECTION ( 'NONE',  ( 0.000000000000000000, 0.000000000000000000, -1.000000000000000000 ) ) ;
#8205 = CARTESIAN_POINT ( 'NONE',  ( -13.75032424529999986, -27.60893268180000248, 222.0000000000000000 ) ) ;
#8206 = CARTESIAN_POINT ( 'NONE',  ( -19.80526803560000104, 19.50877411510000314, 227.0000000000000000 ) ) ;
#8207 = DIRECTION ( 'NONE',  ( 0.000000000000000000, -1.000000000000000000, 2.257145581549999994E-12 ) ) ;
#8208 = ORIENTED_EDGE ( 'NONE', *, *, #1297, .T. ) ;
#8209 = CARTESIAN_POINT ( 'NONE',  ( 3.992508014903327407, 4.044424149039453908, -56.90805965152499368 ) ) ;
#8210 = CARTESIAN_POINT ( 'NONE',  ( -14.94562240850000023, -8.628859120750000500, 5.000000000000000000 ) ) ;
#8211 = CARTESIAN_POINT ( 'NONE',  ( 1.699015317690025118, 6.330513620609809600, -2.053410702900000828 ) ) ;
#8212 = ORIENTED_EDGE ( 'NONE', *, *, #5009, .F. ) ;
#8213 = CARTESIAN_POINT ( 'NONE',  ( -24.90119785323401302, 12.82531120033124594, 8.000000000000007105 ) ) ;
#8214 = CARTESIAN_POINT ( 'NONE',  ( -4.643748704705192409, 0.8058717780413064968, -68.10000000002500542 ) ) ;
#8215 = AXIS2_PLACEMENT_3D ( 'NONE', #28705, #28084, #6837 ) ;
#8216 = EDGE_CURVE ( 'NONE', #11991, #9796, #21853, .T. ) ;
#8217 = AXIS2_PLACEMENT_3D ( 'NONE', #2626, #7193, #30962 ) ;
#8218 = ORIENTED_EDGE ( 'NONE', *, *, #28751, .F. ) ;
#8219 = ORIENTED_EDGE ( 'NONE', *, *, #3563, .T. ) ;
#8220 = CARTESIAN_POINT ( 'NONE',  ( -3.373344672752120132, 1.082959996301855021, -88.52261276241732446 ) ) ;
#8221 = ORIENTED_EDGE ( 'NONE', *, *, #15029, .F. ) ;
#8222 = AXIS2_PLACEMENT_3D ( 'NONE', #4537, #23124, #9244 ) ;
#8223 = LINE ( 'NONE', #26974, #4432 ) ;
#8224 = PLANE ( 'NONE',  #30555 ) ;
#8225 = CARTESIAN_POINT ( 'NONE',  ( -3.135263495375002485, -4.229858287293371433, -64.38409070562499892 ) ) ;
#8226 = CARTESIAN_POINT ( 'NONE',  ( -27.77512470389999777, -10.20462277120000039, 229.2930777930000090 ) ) ;
#8227 = CARTESIAN_POINT ( 'NONE',  ( 16.40303402075260308, 10.20816091466531716, 0.000000000000000000 ) ) ;
#8228 = CARTESIAN_POINT ( 'NONE',  ( -27.03927855759999943, -7.087469713119999959, 222.0000000000000000 ) ) ;
#8229 = PRESENTATION_LAYER_ASSIGNMENT (  '', '', ( #17802 ) ) ;
#8230 =( NAMED_UNIT ( * ) PLANE_ANGLE_UNIT ( ) SI_UNIT ( $, .RADIAN. ) );
#8231 = ADVANCED_FACE ( 'NONE', ( #26563 ), #141, .F. ) ;
#8232 = CARTESIAN_POINT ( 'NONE',  ( -25.46368746804859740, 12.80129684245613575, 4.895780543000022078 ) ) ;
#8233 = ORIENTED_EDGE ( 'NONE', *, *, #12057, .T. ) ;
#8234 = DIRECTION ( 'NONE',  ( 0.000000000000000000, -0.3420201433259318913, 0.9396926207858126157 ) ) ;
#8235 = CIRCLE ( 'NONE', #26857, 1.500000000000000222 ) ;
#8236 = DIRECTION ( 'NONE',  ( -1.000000000000000000, 0.000000000000000000, 0.000000000000000000 ) ) ;
#8237 = ORIENTED_EDGE ( 'NONE', *, *, #25937, .T. ) ;
#8238 = FACE_OUTER_BOUND ( 'NONE', #29224, .T. ) ;
#8239 = CARTESIAN_POINT ( 'NONE',  ( 16.47629287236006590, -8.131162914937760888, -0.6999999999999784173 ) ) ;
#8240 = STYLED_ITEM ( 'NONE', ( #17546 ), #21535 ) ;
#8241 = VECTOR ( 'NONE', #13416, 1000.000000000000114 ) ;
#8242 = CARTESIAN_POINT ( 'NONE',  ( -23.78314118801539934, -14.39461388281613097, 6.098654095000016540 ) ) ;
#8243 = AXIS2_PLACEMENT_3D ( 'NONE', #21352, #30492, #30792 ) ;
#8244 = CARTESIAN_POINT ( 'NONE',  ( 25.72310959295360533, 9.312057329555777585, 0.000000000000000000 ) ) ;
#8245 = AXIS2_PLACEMENT_3D ( 'NONE', #16271, #14081, #14392 ) ;
#8246 = DIRECTION ( 'NONE',  ( -1.000000000000000000, 0.000000000000000000, 0.000000000000000000 ) ) ;
#8247 = CARTESIAN_POINT ( 'NONE',  ( -0.1094138230076618645, -3.801899662088418008, -0.6999999999999994005 ) ) ;
#8248 = B_SPLINE_CURVE_WITH_KNOTS ( 'NONE', 3,
 ( #28956, #12426, #4889, #15104, #10077, #14799 ),
 .UNSPECIFIED., .F., .F.,
 ( 4, 2, 4 ),
 ( 0.000000000000000000, 0.5000000000000000000, 1.000000000000000000 ),
 .UNSPECIFIED. ) ;
#8249 = CARTESIAN_POINT ( 'NONE',  ( 11.00000000000000000, 25.22617105830878614, -61.82510970417090590 ) ) ;
#8250 = CARTESIAN_POINT ( 'NONE',  ( 22.71519155913117061, -14.22192772740461209, 224.4424652943675937 ) ) ;
#8251 = ORIENTED_EDGE ( 'NONE', *, *, #5539, .F. ) ;
#8252 = ADVANCED_FACE ( 'NONE', ( #16646 ), #25760, .F. ) ;
#8253 = CARTESIAN_POINT ( 'NONE',  ( 0.000000000000000000, 5.495185456771864096, -69.00660115587162124 ) ) ;
#8254 = DIRECTION ( 'NONE',  ( 0.8090169943751909232, 0.5877852522921378498, 0.000000000000000000 ) ) ;
#8255 = ADVANCED_FACE ( 'NONE', ( #21538 ), #17111, .F. ) ;
#8256 = CARTESIAN_POINT ( 'NONE',  ( -9.738910687886855655, -24.96785170200598714, 27.99999999999999645 ) ) ;
#8257 = CARTESIAN_POINT ( 'NONE',  ( 0.4831567132655384955, -28.49614615030703391, 6.099998581000020792 ) ) ;
#8258 = CARTESIAN_POINT ( 'NONE',  ( -10.46446609379999870, 21.70000000000000284, -54.63553390589999736 ) ) ;
#8259 = EDGE_CURVE ( 'NONE', #5262, #23982, #9022, .T. ) ;
#8260 = SURFACE_STYLE_FILL_AREA ( #27008 ) ;
#8261 = CARTESIAN_POINT ( 'NONE',  ( -8.699999999715885224, -26.99999999997790923, -28.40000000002690683 ) ) ;
#8262 = CARTESIAN_POINT ( 'NONE',  ( 0.000000000000000000, 0.000000000000000000, 190.0000000000000000 ) ) ;
#8263 = AXIS2_PLACEMENT_3D ( 'NONE', #15318, #24919, #15936 ) ;
#8264 = CARTESIAN_POINT ( 'NONE',  ( 3.178712542294670040, -4.426710093576285310, -62.32197827312499783 ) ) ;
#8265 = EDGE_LOOP ( 'NONE', ( #27781, #1029, #20308, #22611, #2372, #30065, #20942, #31050, #8817, #12537, #9946, #14384, #9980, #27622, #11726, #7908, #8973, #14684, #4174, #22832, #16867, #1119, #2299, #9055, #23858, #1441, #18349, #976, #17784, #14023, #15652, #7423, #27351, #5032, #1868, #2889, #17705, #21604, #24021, #24579, #27495, #21069, #24534, #14403 ) ) ;
#8266 = CARTESIAN_POINT ( 'NONE',  ( 18.26224557211887145, 20.00000411661503108, 230.6762370528171004 ) ) ;
#8267 = ORIENTED_EDGE ( 'NONE', *, *, #28720, .T. ) ;
#8269 = EDGE_CURVE ( 'NONE', #15738, #18576, #24201, .T. ) ;
#8268 = CARTESIAN_POINT ( 'NONE',  ( 27.71078648026139390, -9.612516398576929078, 0.2686740700000300741 ) ) ;
#8270 = ORIENTED_EDGE ( 'NONE', *, *, #24379, .F. ) ;
#8271 = CARTESIAN_POINT ( 'NONE',  ( 18.63941909573550859, 10.97998838177520931, -1.972246272986471594 ) ) ;
#8272 = CARTESIAN_POINT ( 'NONE',  ( -12.30000000005458460, -24.00000000000000711, -28.79269908189872851 ) ) ;
#8273 = CARTESIAN_POINT ( 'NONE',  ( -25.94284618478185322, -6.948772836044507351, 143.2171415880000040 ) ) ;
#8274 = MECHANICAL_DESIGN_GEOMETRIC_PRESENTATION_REPRESENTATION (  '', ( #272 ), #28405 ) ;
#8275 = CARTESIAN_POINT ( 'NONE',  ( -17.45872973692355501, -25.26842553675004410, -33.17377770962026062 ) ) ;
#8276 = CARTESIAN_POINT ( 'NONE',  ( -6.000000000000000000, -29.96004123392021157, -79.78289277550334191 ) ) ;
#8277 = CARTESIAN_POINT ( 'NONE',  ( -0.4702726640079999965, -27.79650200060000031, 223.9974845609999932 ) ) ;
#8278 = ORIENTED_EDGE ( 'NONE', *, *, #5377, .T. ) ;
#8279 = CARTESIAN_POINT ( 'NONE',  ( -8.699999999737658030, -25.77531388886905006, -25.66136093486021608 ) ) ;
#8280 = CARTESIAN_POINT ( 'NONE',  ( 27.63177356800000339, -3.383804547859999682E-15, 137.3605236429999934 ) ) ;
#8281 = ADVANCED_FACE ( 'NONE', ( #6891 ), #30977, .F. ) ;
#8282 = CARTESIAN_POINT ( 'NONE',  ( 4.725722714813314518, -3.873618144263061946, -23.99674734060000603 ) ) ;
#8283 = CARTESIAN_POINT ( 'NONE',  ( -24.68204616399999907, -14.25020164319999871, 226.1000014189999945 ) ) ;
#8284 = DIRECTION ( 'NONE',  ( -1.000000000000000000, 5.665498452320000818E-16, 0.000000000000000000 ) ) ;
#8285 = CARTESIAN_POINT ( 'NONE',  ( 9.999999999968624209, -29.62135916550975168, -29.91085694027753306 ) ) ;
#8286 = CARTESIAN_POINT ( 'NONE',  ( 0.000000000000000000, 0.000000000000000000, 140.0000000000000000 ) ) ;
#8287 = CARTESIAN_POINT ( 'NONE',  ( -5.221537131022022216, 0.5214849208526588509, -46.87737393802500918 ) ) ;
#8288 = DIRECTION ( 'NONE',  ( 0.000000000000000000, 1.000000000000000000, 0.000000000000000000 ) ) ;
#8289 = EDGE_CURVE ( 'NONE', #24204, #25555, #19898, .T. ) ;
#8290 = CARTESIAN_POINT ( 'NONE',  ( 6.076762841307634666, -26.10292173851731690, 208.8288339172677013 ) ) ;
#8291 = CARTESIAN_POINT ( 'NONE',  ( -19.33022990401857300, 20.00006911879202320, 230.3642850961209660 ) ) ;
#8292 = CARTESIAN_POINT ( 'NONE',  ( -26.79999999999997939, -1.754055898257046664, 43.21714158836666542 ) ) ;
#8293 = CARTESIAN_POINT ( 'NONE',  ( 17.95841148951064525, -9.763538383420391042, 0.000000000000000000 ) ) ;
#8294 = ORIENTED_EDGE ( 'NONE', *, *, #18911, .F. ) ;
#8295 = CARTESIAN_POINT ( 'NONE',  ( -4.773116892509256637, 0.6906165796890335606, -35.19533976329999803 ) ) ;
#8296 = AXIS2_PLACEMENT_3D ( 'NONE', #12418, #29250, #19514 ) ;
#8297 = ORIENTED_EDGE ( 'NONE', *, *, #29051, .T. ) ;
#8298 = CARTESIAN_POINT ( 'NONE',  ( -10.69999999999999929, -27.00000000000000000, -31.39999999999999858 ) ) ;
#8299 = CARTESIAN_POINT ( 'NONE',  ( 5.329043336022200705, 2.363500563244980590, -52.67998794302499022 ) ) ;
#8300 = ORIENTED_EDGE ( 'NONE', *, *, #30470, .F. ) ;
#8301 = VERTEX_POINT ( 'NONE', #10350 ) ;
#8302 = APPLICATION_PROTOCOL_DEFINITION ( 'draft international standard', 'automotive_design', 1998, #2950 ) ;
#8303 = EDGE_LOOP ( 'NONE', ( #19560, #26626, #4810, #17387 ) ) ;
#8304 = EDGE_CURVE ( 'NONE', #17178, #13324, #14455, .T. ) ;
#8305 = ORIENTED_EDGE ( 'NONE', *, *, #19824, .F. ) ;
#8306 = CARTESIAN_POINT ( 'NONE',  ( 24.25742563242670613, 13.58028021435546684, 4.319317656000021266 ) ) ;
#8307 = CARTESIAN_POINT ( 'NONE',  ( 2.131628207279999844E-14, 1.421085471519999843E-14, 231.6999999999999886 ) ) ;
#8308 = DIRECTION ( 'NONE',  ( 1.000000000000000000, 0.000000000000000000, 0.000000000000000000 ) ) ;
#8309 = EDGE_CURVE ( 'NONE', #16475, #17862, #21485, .T. ) ;
#8310 = DIRECTION ( 'NONE',  ( -0.9316362575375356503, -0.3633921898465275468, 0.000000000000000000 ) ) ;
#8311 = DIRECTION ( 'NONE',  ( 2.966217977826874882E-25, -1.000000000000000000, 2.257145581549900232E-12 ) ) ;
#8312 = CARTESIAN_POINT ( 'NONE',  ( -3.748827661146469481, 2.120144271060945051, -0.6999999999999992895 ) ) ;
#8313 = CARTESIAN_POINT ( 'NONE',  ( 5.530149664617865390, 2.595584118083901881, -2.479170051700001043 ) ) ;
#8314 = CARTESIAN_POINT ( 'NONE',  ( -3.503090509784088091, -0.9324612817112352126, 227.7184664424322591 ) ) ;
#8315 = CARTESIAN_POINT ( 'NONE',  ( -16.04158851046123502, 10.23646161653652875, 0.000000000000000000 ) ) ;
#8316 = CARTESIAN_POINT ( 'NONE',  ( -0.7008090670319790938, 4.721317983490957992, -11.80522091660000505 ) ) ;
#8317 = CARTESIAN_POINT ( 'NONE',  ( 2.831388952324535691, -5.386915550550475551, -33.20721934060000535 ) ) ;
#8318 = CARTESIAN_POINT ( 'NONE',  ( -8.699999999638116321, -22.83323352287542463, -39.84673049988318638 ) ) ;
#8319 = CARTESIAN_POINT ( 'NONE',  ( 17.99591112602217891, 19.96082062028142090, 0.000000000000000000 ) ) ;
#8320 = CARTESIAN_POINT ( 'NONE',  ( -20.77600556914587315, -21.68409854326995045, 8.000000000000007105 ) ) ;
#8321 = CARTESIAN_POINT ( 'NONE',  ( 3.550686850769999806E-05, -28.50022181210000127, 226.1000014189999945 ) ) ;
#8322 = DIRECTION ( 'NONE',  ( 0.9915824307782121760, 0.1294769592320275942, -4.045530494348897360E-18 ) ) ;
#8323 = CARTESIAN_POINT ( 'NONE',  ( 22.77614505612612206, -14.12431931114201866, 225.7119260791445186 ) ) ;
#8324 = DIRECTION ( 'NONE',  ( -1.000000000000000000, 0.000000000000000000, 0.000000000000000000 ) ) ;
#8325 = DIRECTION ( 'NONE',  ( 1.000000000000000000, 0.000000000000000000, 0.000000000000000000 ) ) ;
#8326 = ORIENTED_EDGE ( 'NONE', *, *, #4777, .T. ) ;
#8327 = CARTESIAN_POINT ( 'NONE',  ( 23.76534794177020871, 14.42397062701149935, 6.095965061000018892 ) ) ;
#8328 = DIRECTION ( 'NONE',  ( -0.2665630446479613780, -0.9085064176298685013, -0.3218077568259533061 ) ) ;
#8329 = VERTEX_POINT ( 'NONE', #8276 ) ;
#8330 = B_SPLINE_CURVE_WITH_KNOTS ( 'NONE', 5,
 ( #20253, #3572, #24524, #24675, #5323, #922 ),
 .UNSPECIFIED., .F., .F.,
 ( 6, 6 ),
 ( 0.000000000000000000, 2.300779717520000212 ),
 .UNSPECIFIED. ) ;
#8331 = B_SPLINE_CURVE_WITH_KNOTS ( 'NONE', 5,
 ( #7027, #30791, #28117, #28427, #28729, #6861, #16463, #111, #26077, #25768, #16616, #26223, #2316, #23717, #12056 ),
 .UNSPECIFIED., .F., .F.,
 ( 6, 3, 3, 3, 6 ),
 ( 0.000000000000000000, 0.1000000000005726170, 0.4000000000022904678, 0.7000000000005726086, 1.000000000000000000 ),
 .UNSPECIFIED. ) ;
#8332 = LINE ( 'NONE', #27540, #4713 ) ;
#8333 = FACE_OUTER_BOUND ( 'NONE', #22068, .T. ) ;
#8334 = ORIENTED_EDGE ( 'NONE', *, *, #4064, .F. ) ;
#8335 = CARTESIAN_POINT ( 'NONE',  ( -6.965151789112635328, -26.60412671351617320, 21.61051234482303585 ) ) ;
#8336 = VERTEX_POINT ( 'NONE', #20104 ) ;
#8337 = ORIENTED_EDGE ( 'NONE', *, *, #28321, .T. ) ;
#8338 =( NAMED_UNIT ( * ) SI_UNIT ( $, .STERADIAN. ) SOLID_ANGLE_UNIT ( ) );
#8339 = ORIENTED_EDGE ( 'NONE', *, *, #15827, .T. ) ;
#8340 = CARTESIAN_POINT ( 'NONE',  ( 23.93626153989999850, 13.29299652659999964, 230.6999999999999886 ) ) ;
#8341 = EDGE_CURVE ( 'NONE', #23857, #27091, #5613, .T. ) ;
#8342 = CARTESIAN_POINT ( 'NONE',  ( 10.80000000000790550, -15.94902145823651907, -35.53273252494266643 ) ) ;
#8343 = DIRECTION ( 'NONE',  ( 0.000000000000000000, 0.000000000000000000, -1.000000000000000000 ) ) ;
#8344 = DIRECTION ( 'NONE',  ( 0.000000000000000000, 1.000000000000000000, 0.000000000000000000 ) ) ;
#8345 = LINE ( 'NONE', #17941, #26001 ) ;
#8346 = ADVANCED_FACE ( 'NONE', ( #14918 ), #4399, .T. ) ;
#8347 = CARTESIAN_POINT ( 'NONE',  ( 8.999999999770000869, 21.70000000000000284, -57.60000000000000142 ) ) ;
#8348 = ORIENTED_EDGE ( 'NONE', *, *, #29638, .T. ) ;
#8349 = ADVANCED_FACE ( 'NONE', ( #12860 ), #15521, .F. ) ;
#8350 = CARTESIAN_POINT ( 'NONE',  ( -3.552713678799999608E-15, 0.000000000000000000, 193.2171415880000040 ) ) ;
#8351 = DIRECTION ( 'NONE',  ( 1.020425574104003999E-15, 0.000000000000000000, -1.000000000000000000 ) ) ;
#8352 = CARTESIAN_POINT ( 'NONE',  ( 6.105340317846409626, -0.2107885887935728730, -3.285409721200005517 ) ) ;
#8353 = CARTESIAN_POINT ( 'NONE',  ( -3.251750336246070461, -5.089746299513510763, -21.70891267860000795 ) ) ;
#8354 = CARTESIAN_POINT ( 'NONE',  ( -17.93590711870954379, -8.873734598641418003, -0.6999999999999784173 ) ) ;
#8355 =( REPRESENTATION_RELATIONSHIP ('NONE','NONE', #2712, #3523 ) REPRESENTATION_RELATIONSHIP_WITH_TRANSFORMATION ( #16333 )SHAPE_REPRESENTATION_RELATIONSHIP( ) );
#8356 = CARTESIAN_POINT ( 'NONE',  ( 5.032477892872088354, 5.146895567814641304, -43.32728369091649512 ) ) ;
#8357 = CARTESIAN_POINT ( 'NONE',  ( 2.546247159447640573, -4.281382049667992185, -94.54588698005632352 ) ) ;
#8358 = CARTESIAN_POINT ( 'NONE',  ( -23.94309786570000043, 13.28188914049999880, 230.6999999999999886 ) ) ;
#8359 = CARTESIAN_POINT ( 'NONE',  ( 3.093055152476274383, -2.878722282980446412, -96.01609449156637766 ) ) ;
#8360 = LINE ( 'NONE', #3036, #16792 ) ;
#8361 = CARTESIAN_POINT ( 'NONE',  ( 24.08956650215635165, -13.26503430039987919, 224.0404533956383659 ) ) ;
#8362 = CARTESIAN_POINT ( 'NONE',  ( 17.50139513559999926, -5.282204535990000061, 230.6999999999999886 ) ) ;
#8363 = CARTESIAN_POINT ( 'NONE',  ( 23.34643930356318720, -14.53345043283277782, 224.3574895212763636 ) ) ;
#8364 = VERTEX_POINT ( 'NONE', #22764 ) ;
#8365 = CARTESIAN_POINT ( 'NONE',  ( -1.256295066205788347, -5.815478746186413694, -55.45033560642499992 ) ) ;
#8366 = DIRECTION ( 'NONE',  ( 0.000000000000000000, 0.000000000000000000, 1.000000000000000000 ) ) ;
#8367 = ORIENTED_EDGE ( 'NONE', *, *, #13800, .T. ) ;
#8368 = CARTESIAN_POINT ( 'NONE',  ( 3.665953941183818010, 4.858601989977915814, -14.22796858840000311 ) ) ;
#8369 = ORIENTED_EDGE ( 'NONE', *, *, #6177, .F. ) ;
#8370 = CARTESIAN_POINT ( 'NONE',  ( 21.02350438529999721, 19.26967166389999875, 225.9999999149999894 ) ) ;
#8371 = CARTESIAN_POINT ( 'NONE',  ( 25.94284618478187809, -6.948772836044536660, 186.7828584120000244 ) ) ;
#8372 = ORIENTED_EDGE ( 'NONE', *, *, #23999, .F. ) ;
#8373 = ORIENTED_EDGE ( 'NONE', *, *, #2023, .F. ) ;
#8374 = ADVANCED_FACE ( 'NONE', ( #7819 ), #914, .F. ) ;
#8375 = VERTEX_POINT ( 'NONE', #29692 ) ;
#8376 = CARTESIAN_POINT ( 'NONE',  ( 8.999999999770000869, 20.99999999999999645, -51.10000000000000142 ) ) ;
#8377 = SURFACE_SIDE_STYLE ('',( #25235 ) ) ;
#8378 = ORIENTED_EDGE ( 'NONE', *, *, #1443, .F. ) ;
#8379 = CARTESIAN_POINT ( 'NONE',  ( -24.37821945910799926, 14.76389285725497125, 4.791564337000009388 ) ) ;
#8380 = CARTESIAN_POINT ( 'NONE',  ( 10.00000000000000000, -130.0000000000000000, -42.39999999999999858 ) ) ;
#8381 = CARTESIAN_POINT ( 'NONE',  ( 3.916181512753878824, -4.480608557854155904, -64.49605006312501132 ) ) ;
#8382 = CARTESIAN_POINT ( 'NONE',  ( -27.53132592969999948, -10.11505073740000071, 229.7313259299999686 ) ) ;
#8383 = VECTOR ( 'NONE', #22840, 1000.000000000000000 ) ;
#8384 = AXIS2_PLACEMENT_3D ( 'NONE', #18392, #11006, #11474 ) ;
#8385 = CARTESIAN_POINT ( 'NONE',  ( 16.21708932071647524, 10.42683423810934862, -0.000000000000000000 ) ) ;
#8386 = CARTESIAN_POINT ( 'NONE',  ( 8.699999999991231192, -113.1082736041627896, 6.336644015525963347 ) ) ;
#8387 = CARTESIAN_POINT ( 'NONE',  ( 7.636659491129999644, 9.305401069029999306, 224.6412452697800290 ) ) ;
#8388 = ORIENTED_EDGE ( 'NONE', *, *, #5592, .F. ) ;
#8389 = CARTESIAN_POINT ( 'NONE',  ( 4.584724779323398280, 3.684399570781342614, -7.354586408000001185 ) ) ;
#8390 = CARTESIAN_POINT ( 'NONE',  ( -9.993285220779425160, -25.61999708228226069, 202.0000000000000000 ) ) ;
#8391 = CARTESIAN_POINT ( 'NONE',  ( -8.699999998971694737, -25.92947359974585098, -31.20249410827203107 ) ) ;
#8392 = ORIENTED_EDGE ( 'NONE', *, *, #7409, .T. ) ;
#8393 = CARTESIAN_POINT ( 'NONE',  ( 4.440892098500000496E-16, -0.1455297029551360921, -71.05965357398815740 ) ) ;
#8394 = CARTESIAN_POINT ( 'NONE',  ( 16.59368952254167340, -8.049650370620115680, -0.6999999999999784173 ) ) ;
#8395 = CARTESIAN_POINT ( 'NONE',  ( -22.36193249936582816, 17.71394520520996707, 6.000000042999998229 ) ) ;
#8396 = CARTESIAN_POINT ( 'NONE',  ( 18.13790330320517086, 20.33475721090277233, 0.08279788800003018423 ) ) ;
#8397 = CARTESIAN_POINT ( 'NONE',  ( -9.738910687886855655, -24.96785170200598714, 202.0000000000000000 ) ) ;
#8398 = CARTESIAN_POINT ( 'NONE',  ( -5.649653782182448403, -1.974543963569185046, -50.40743646232499486 ) ) ;
#8399 = AXIS2_PLACEMENT_3D ( 'NONE', #1092, #1569, #8310 ) ;
#8400 = CARTESIAN_POINT ( 'NONE',  ( 17.16657240420000008, 10.97998838177520931, 0.05106179917585291356 ) ) ;
#8401 = FACE_OUTER_BOUND ( 'NONE', #17485, .T. ) ;
#8402 = ORIENTED_EDGE ( 'NONE', *, *, #752, .T. ) ;
#8403 = ADVANCED_FACE ( 'NONE', ( #27025 ), #8119, .F. ) ;
#8404 = CARTESIAN_POINT ( 'NONE',  ( 0.000000000000000000, 0.000000000000000000, 93.60555127639999284 ) ) ;
#8405 = LINE ( 'NONE', #30463, #10608 ) ;
#8406 = EDGE_CURVE ( 'NONE', #11038, #9026, #29002, .T. ) ;
#8407 = AXIS2_PLACEMENT_3D ( 'NONE', #2989, #13187, #5496 ) ;
#8408 = CARTESIAN_POINT ( 'NONE',  ( -0.5716039299945605556, -28.49445895580190324, 5.310182064000024127 ) ) ;
#8409 = EDGE_CURVE ( 'NONE', #6473, #10428, #12038, .T. ) ;
#8410 = CARTESIAN_POINT ( 'NONE',  ( 10.35000000039999968, 19.99999999999999645, -42.39999999999999858 ) ) ;
#8411 = CARTESIAN_POINT ( 'NONE',  ( -23.88846875309505080, -13.62395840461769225, 226.1000000000000227 ) ) ;
#8412 = SHAPE_REPRESENTATION_RELATIONSHIP ( 'NONE' , 'NONE' ,  #339, #14437 ) ;
#8413 = CARTESIAN_POINT ( 'NONE',  ( 14.76126683900010761, -23.42592653034165195, -32.10972855315200292 ) ) ;
#8414 = CARTESIAN_POINT ( 'NONE',  ( 0.000000000000000000, 0.000000000000000000, 141.6604601749999972 ) ) ;
#8415 = CARTESIAN_POINT ( 'NONE',  ( 4.009291712408942665, -2.091746824018185347, -61.71790713612498536 ) ) ;
#8416 = ORIENTED_EDGE ( 'NONE', *, *, #11545, .T. ) ;
#8417 = CARTESIAN_POINT ( 'NONE',  ( -8.699999999731330647, -26.52402217114853755, -25.41208138081151091 ) ) ;
#8418 = EDGE_LOOP ( 'NONE', ( #16782, #8893, #12386, #1078 ) ) ;
#8419 = CARTESIAN_POINT ( 'NONE',  ( 8.700000000294114244, -16.25281683561194868, -40.75997113242387826 ) ) ;
#8420 = ORIENTED_EDGE ( 'NONE', *, *, #3470, .T. ) ;
#8421 = ADVANCED_FACE ( 'NONE', ( #23092 ), #21983, .F. ) ;
#8422 = FACE_BOUND ( 'NONE', #4601, .T. ) ;
#8423 = CARTESIAN_POINT ( 'NONE',  ( -12.29999999999291660, -24.60099947280545152, -30.24364016012474110 ) ) ;
#8424 = CARTESIAN_POINT ( 'NONE',  ( 1.790201522669007561, 3.063245535112757434, 0.000000000000000000 ) ) ;
#8425 = VECTOR ( 'NONE', #28822, 1000.000000000000000 ) ;
#8426 = CARTESIAN_POINT ( 'NONE',  ( 18.27566665216736297, 11.02535689755138115, -1.400000000000001910 ) ) ;
#8427 = TOROIDAL_SURFACE ( 'NONE', #24513, 29.80000000000000071, 3.000000000000000000 ) ;
#8428 = CARTESIAN_POINT ( 'NONE',  ( 10.06596365874881194, -25.80632433378973900, 190.0000000000000000 ) ) ;
#8429 = CARTESIAN_POINT ( 'NONE',  ( -0.8057362888000000334, -27.78873281839999976, 224.2403608809999866 ) ) ;
#8430 = ORIENTED_EDGE ( 'NONE', *, *, #6413, .T. ) ;
#8431 = CARTESIAN_POINT ( 'NONE',  ( -0.8531356284651092636, -3.830139717306812130, -44.10000000002499121 ) ) ;
#8432 = DIRECTION ( 'NONE',  ( 1.000000000000000000, -1.224606353819998843E-16, 0.000000000000000000 ) ) ;
#8433 = CARTESIAN_POINT ( 'NONE',  ( 1.092747331740645533, -27.77868070731554795, 225.1457540162050748 ) ) ;
#8434 = CARTESIAN_POINT ( 'NONE',  ( -2.601833019719681950, 2.493493017038428405, 230.7766559207227601 ) ) ;
#8435 = B_SPLINE_CURVE_WITH_KNOTS ( 'NONE', 3,
 ( #11619, #23442, #16183, #18541, #16026, #19007, #18388, #6883, #23274, #11470 ),
 .UNSPECIFIED., .F., .F.,
 ( 4, 2, 2, 2, 4 ),
 ( 0.000000000000000000, 0.2500000000000000000, 0.5000000000000000000, 0.7500000000000000000, 1.000000000000000000 ),
 .UNSPECIFIED. ) ;
#8436 = DIRECTION ( 'NONE',  ( 0.000000000000000000, 0.3420201433259318913, -0.9396926207858126157 ) ) ;
#8437 = FACE_BOUND ( 'NONE', #12610, .T. ) ;
#8438 = DIRECTION ( 'NONE',  ( -1.000000000000000000, 5.063197467948052462E-16, -2.257212216284997029E-12 ) ) ;
#8439 = FACE_OUTER_BOUND ( 'NONE', #16245, .T. ) ;
#8440 = CARTESIAN_POINT ( 'NONE',  ( -4.507646854653408752, 2.674235333181991692, -50.08267869292500052 ) ) ;
#8441 = CIRCLE ( 'NONE', #10982, 10.00000000000000178 ) ;
#8442 = DIRECTION ( 'NONE',  ( -5.962915006522622422E-16, -0.4383711467890810676, -0.8987940462991651502 ) ) ;
#8443 = LINE ( 'NONE', #18043, #3222 ) ;
#8444 = CARTESIAN_POINT ( 'NONE',  ( -18.12672911204381165, 19.99995619754870901, 230.6891754141428237 ) ) ;
#8445 = CARTESIAN_POINT ( 'NONE',  ( -23.82266443414332002, -12.31939917416737096, 43.21714158843889919 ) ) ;
#8446 = B_SPLINE_CURVE_WITH_KNOTS ( 'NONE', 3,
 ( #10104, #8179, #7726, #17332, #19862, #26938 ),
 .UNSPECIFIED., .F., .F.,
 ( 4, 2, 4 ),
 ( 0.000000000000000000, 0.5000000000000000000, 1.000000000000000000 ),
 .UNSPECIFIED. ) ;
#8447 = AXIS2_PLACEMENT_3D ( 'NONE', #1162, #20199, #10455 ) ;
#8448 = EDGE_CURVE ( 'NONE', #10023, #23549, #11926, .T. ) ;
#8449 = CARTESIAN_POINT ( 'NONE',  ( 23.81569860410000317, -13.75000000000000000, 226.0999999999999943 ) ) ;
#8450 = EDGE_LOOP ( 'NONE', ( #19044, #406, #15581, #13701 ) ) ;
#8451 = CARTESIAN_POINT ( 'NONE',  ( -4.901082056047598279, -4.330235462250267453, -34.43447003409999496 ) ) ;
#8452 = CIRCLE ( 'NONE', #14184, 18.16530045500000057 ) ;
#8453 = VERTEX_POINT ( 'NONE', #30320 ) ;
#8454 = CARTESIAN_POINT ( 'NONE',  ( -1.861312627816293253, -17.80543024186813383, -28.79488058872718881 ) ) ;
#8455 = CARTESIAN_POINT ( 'NONE',  ( 0.8648632234848976363, -6.342619565911398638, -49.76468436622499780 ) ) ;
#8456 = ORIENTED_EDGE ( 'NONE', *, *, #5021, .F. ) ;
#8457 = ORIENTED_EDGE ( 'NONE', *, *, #30368, .F. ) ;
#8458 = ORIENTED_EDGE ( 'NONE', *, *, #25765, .T. ) ;
#8459 = EDGE_CURVE ( 'NONE', #16870, #29062, #4118, .T. ) ;
#8460 = CARTESIAN_POINT ( 'NONE',  ( -17.93324555108848628, -9.020011617866936504, 0.000000000000000000 ) ) ;
#8461 = DIRECTION ( 'NONE',  ( 0.000000000000000000, 0.000000000000000000, -1.000000000000000000 ) ) ;
#8462 = DIRECTION ( 'NONE',  ( 0.000000000000000000, 0.000000000000000000, 1.000000000000000000 ) ) ;
#8463 = AXIS2_PLACEMENT_3D ( 'NONE', #21347, #30944, #7024 ) ;
#8464 = EDGE_CURVE ( 'NONE', #15501, #3166, #6245, .T. ) ;
#8465 = DIRECTION ( 'NONE',  ( 1.000000000000000000, 0.000000000000000000, 0.000000000000000000 ) ) ;
#8466 = DIRECTION ( 'NONE',  ( 0.2815395311429196301, 0.9595496299847262600, 0.000000000000000000 ) ) ;
#8467 = EDGE_CURVE ( 'NONE', #7653, #20431, #9914, .T. ) ;
#8468 = CARTESIAN_POINT ( 'NONE',  ( -4.062788589238770953, 2.328859124429163430, -0.6999999999999992895 ) ) ;
#8469 = CARTESIAN_POINT ( 'NONE',  ( 3.950106903291103588, 1.853988655799144958, -2.479170051700008148 ) ) ;
#8470 = CARTESIAN_POINT ( 'NONE',  ( -3.691781163152999312, -0.6055607618816524207, 227.7772386881452462 ) ) ;
#8471 = CARTESIAN_POINT ( 'NONE',  ( 3.550686847520000117E-05, -28.50022181210000127, 223.9000014189999774 ) ) ;
#8472 = EDGE_LOOP ( 'NONE', ( #3082, #25232, #17267, #4376 ) ) ;
#8473 = EDGE_CURVE ( 'NONE', #14200, #16868, #3787, .T. ) ;
#8474 = CARTESIAN_POINT ( 'NONE',  ( -4.101794773660127902, 5.071170285176791914, -14.20352819870000083 ) ) ;
#8475 = CARTESIAN_POINT ( 'NONE',  ( 3.471037982653067733, 3.337515987827158526, -34.38591724620000178 ) ) ;
#8476 = CONICAL_SURFACE ( 'NONE', #21555, 3.491271820449999286, 1.047197551199999799 ) ;
#8477 = CYLINDRICAL_SURFACE ( 'NONE', #11687, 3.000000000000000444 ) ;
#8478 = FACE_OUTER_BOUND ( 'NONE', #12410, .T. ) ;
#8479 = FACE_OUTER_BOUND ( 'NONE', #4477, .T. ) ;
#8480 = CARTESIAN_POINT ( 'NONE',  ( -17.48914026050856663, -29.21618945753110097, -32.89398511221816079 ) ) ;
#8481 = CARTESIAN_POINT ( 'NONE',  ( 20.30405755279999980, 20.00000000000000000, 227.7999999360000061 ) ) ;
#8482 = LINE ( 'NONE', #5975, #25817 ) ;
#8483 = CARTESIAN_POINT ( 'NONE',  ( -7.534632680830990026, -7.897185061638417380, -36.96526048005145526 ) ) ;
#8484 = EDGE_CURVE ( 'NONE', #27419, #4224, #9405, .T. ) ;
#8485 = ORIENTED_EDGE ( 'NONE', *, *, #25123, .F. ) ;
#8486 = VERTEX_POINT ( 'NONE', #8428 ) ;
#8487 = DIRECTION ( 'NONE',  ( -1.000000000000000000, 0.000000000000000000, 0.000000000000000000 ) ) ;
#8488 = CYLINDRICAL_SURFACE ( 'NONE', #26329, 1.099999999999998979 ) ;
#8489 = ORIENTED_EDGE ( 'NONE', *, *, #22964, .T. ) ;
#8490 = CARTESIAN_POINT ( 'NONE',  ( -1.549220603345442315, -3.499999999999999556, 227.8316576175188857 ) ) ;
#8491 = CARTESIAN_POINT ( 'NONE',  ( -25.22069443620000229, -13.27363204220000092, 224.7915656799999908 ) ) ;
#8492 = ORIENTED_EDGE ( 'NONE', *, *, #3778, .F. ) ;
#8493 = LINE ( 'NONE', #3793, #15012 ) ;
#8494 = ORIENTED_EDGE ( 'NONE', *, *, #19106, .F. ) ;
#8495 = ADVANCED_FACE ( 'NONE', ( #8588 ), #25000, .T. ) ;
#8496 = ORIENTED_EDGE ( 'NONE', *, *, #4, .F. ) ;
#8497 = SHAPE_REPRESENTATION_RELATIONSHIP ( 'NONE' , 'NONE' ,  #6935, #9916 ) ;
#8498 = VECTOR ( 'NONE', #17187, 1000.000000000000000 ) ;
#8499 = ORIENTED_EDGE ( 'NONE', *, *, #50, .T. ) ;
#8500 = CARTESIAN_POINT ( 'NONE',  ( -0.1113126274910263003, 48.20259643650151560, -60.98914630669319337 ) ) ;
#8501 = ORIENTED_EDGE ( 'NONE', *, *, #50, .F. ) ;
#8502 = DIRECTION ( 'NONE',  ( 0.000000000000000000, 1.000000000000000000, 0.000000000000000000 ) ) ;
#8503 = CARTESIAN_POINT ( 'NONE',  ( 28.49999999979999998, -7.466149220249999274, 222.0000000000000000 ) ) ;
#8504 = CYLINDRICAL_SURFACE ( 'NONE', #3474, 26.80000000000002203 ) ;
#8505 = CARTESIAN_POINT ( 'NONE',  ( 10.35000000039999968, -130.0000000000000000, -42.39999999999999858 ) ) ;
#8506 = CARTESIAN_POINT ( 'NONE',  ( -8.699999999650268379, -15.05691612485074948, -37.86814428179198444 ) ) ;
#8507 = CARTESIAN_POINT ( 'NONE',  ( 23.77307027441306531, -14.41181805765238444, 4.999998581000003384 ) ) ;
#8508 = VERTEX_POINT ( 'NONE', #18973 ) ;
#8509 = CARTESIAN_POINT ( 'NONE',  ( 2.223383862040879677, -3.430296892840221101, -0.6659393883000006564 ) ) ;
#8510 = CARTESIAN_POINT ( 'NONE',  ( -3.251750336246070461, -5.089746299513510763, -21.10891267850000119 ) ) ;
#8511 = DIRECTION ( 'NONE',  ( 0.000000000000000000, -1.000000000000000000, 0.000000000000000000 ) ) ;
#8512 = B_SPLINE_CURVE_WITH_KNOTS ( 'NONE', 5,
 ( #8025, #1740, #20769, #11173, #20931, #21091, #28163, #27848, #8964, #1426, #30686, #23459, #18236, #6909, #21241 ),
 .UNSPECIFIED., .F., .F.,
 ( 6, 3, 3, 3, 6 ),
 ( 0.000000000000000000, 0.5239017171269999551, 1.047803434249999999, 1.571705151379999998, 1.746339057089999924 ),
 .UNSPECIFIED. ) ;
#8513 = CARTESIAN_POINT ( 'NONE',  ( -10.46447140189999914, 20.99999999999999645, -54.63552859760000047 ) ) ;
#8514 = CARTESIAN_POINT ( 'NONE',  ( -0.8084728434465671132, -5.179733586367765596, -93.14092889888253524 ) ) ;
#8515 = CARTESIAN_POINT ( 'NONE',  ( -27.44635497490000020, 9.596816764059999727, 229.4982322489999831 ) ) ;
#8516 = CARTESIAN_POINT ( 'NONE',  ( -23.48198671369468116, 16.77395784647688970, 1.000000000000000888 ) ) ;
#8517 = CARTESIAN_POINT ( 'NONE',  ( 10.69999999999999929, -43.95328087560000085, -27.24755286599999948 ) ) ;
#8518 = AXIS2_PLACEMENT_3D ( 'NONE', #5841, #15443, #3476 ) ;
#8519 = CARTESIAN_POINT ( 'NONE',  ( -23.10935684530000245, -20.42749692129999772, 229.0000000000000000 ) ) ;
#8520 = CARTESIAN_POINT ( 'NONE',  ( -4.340019564239999461, -26.72143554420000200, 230.6999999999999886 ) ) ;
#8521 = CARTESIAN_POINT ( 'NONE',  ( 0.000000000000000000, 21.70000000000000284, -44.10000000017312516 ) ) ;
#8522 = EDGE_CURVE ( 'NONE', #23742, #12454, #22493, .T. ) ;
#8523 = ORIENTED_EDGE ( 'NONE', *, *, #16365, .F. ) ;
#8524 = CARTESIAN_POINT ( 'NONE',  ( 4.003591150705128499, -2.204345408526048988, -57.90843849682499211 ) ) ;
#8525 = DIRECTION ( 'NONE',  ( -5.962915006522622422E-16, -0.4383711467890810676, -0.8987940462991651502 ) ) ;
#8526 = ORIENTED_EDGE ( 'NONE', *, *, #3269, .T. ) ;
#8527 = EDGE_CURVE ( 'NONE', #26138, #13706, #13534, .T. ) ;
#8528 = CARTESIAN_POINT ( 'NONE',  ( 5.530149664617865390, 2.595584118083901881, -2.479170051700001043 ) ) ;
#8529 = ORIENTED_EDGE ( 'NONE', *, *, #3810, .F. ) ;
#8530 = EDGE_CURVE ( 'NONE', #23432, #27907, #26953, .T. ) ;
#8531 = CARTESIAN_POINT ( 'NONE',  ( -4.861312627816293030, -18.46298696203981038, -30.14307165818175704 ) ) ;
#8532 = CARTESIAN_POINT ( 'NONE',  ( -4.047171486430775289, -0.4744283861493229226, -68.10000000002499121 ) ) ;
#8533 = EDGE_CURVE ( 'NONE', #28636, #5828, #24740, .T. ) ;
#8534 = VERTEX_POINT ( 'NONE', #11591 ) ;
#8535 = CARTESIAN_POINT ( 'NONE',  ( 10.71199981179999838, 19.99999999999999645, -2.204042935800003100 ) ) ;
#8536 = ORIENTED_EDGE ( 'NONE', *, *, #13953, .T. ) ;
#8537 = ORIENTED_EDGE ( 'NONE', *, *, #12640, .F. ) ;
#8538 = CARTESIAN_POINT ( 'NONE',  ( 24.34663841809999951, -12.78636765230000094, 5.000000000000000000 ) ) ;
#8539 = PRESENTATION_STYLE_ASSIGNMENT (( #8694 ) ) ;
#8540 = VERTEX_POINT ( 'NONE', #689 ) ;
#8541 = CARTESIAN_POINT ( 'NONE',  ( 17.16657240419154462, 10.99999999996915179, -0.6999999999999784173 ) ) ;
#8542 = DIRECTION ( 'NONE',  ( -1.000000000000000000, 0.000000000000000000, 0.000000000000000000 ) ) ;
#8543 = CARTESIAN_POINT ( 'NONE',  ( -3.750715812471464350, 4.529495762826656780, -62.19933298482499850 ) ) ;
#8544 = CARTESIAN_POINT ( 'NONE',  ( -27.79999999999999716, 2.355804440410000085E-11, 229.1414213560000235 ) ) ;
#8545 = APPLICATION_CONTEXT ( 'automotive_design' ) ;
#8546 = CARTESIAN_POINT ( 'NONE',  ( -0.8355090854489903851, -26.78702287505212709, 224.2806846201137887 ) ) ;
#8547 = CARTESIAN_POINT ( 'NONE',  ( 16.20123158609999692, 11.52736809249999617, -0.7999999992999995424 ) ) ;
#8548 = VECTOR ( 'NONE', #17103, 1000.000000000000000 ) ;
#8549 = CARTESIAN_POINT ( 'NONE',  ( 8.699999999987257482, -114.1237136972522990, 7.129097341238439967 ) ) ;
#8550 = CARTESIAN_POINT ( 'NONE',  ( -24.93720648713954446, 13.79881813474513486, 3.899998581000013509 ) ) ;
#8551 = CARTESIAN_POINT ( 'NONE',  ( 5.399570250832249840, -0.9558082389699539272, -7.771482634700006109 ) ) ;
#8552 = CARTESIAN_POINT ( 'NONE',  ( 25.94284618478187809, -6.948772836044536660, 136.7828584120000244 ) ) ;
#8553 = PRODUCT_DEFINITION_SHAPE ( 'NONE', 'NONE',  #18101 ) ;
#8554 = CARTESIAN_POINT ( 'NONE',  ( 19.49298387170000169, 19.58648673140000440, 229.5592795560000070 ) ) ;
#8555 = ORIENTED_EDGE ( 'NONE', *, *, #5775, .F. ) ;
#8556 = CARTESIAN_POINT ( 'NONE',  ( 24.10986967230000033, -13.84040926149999962, 223.9013457789999961 ) ) ;
#8557 = CARTESIAN_POINT ( 'NONE',  ( -24.05769994060051786, -13.93129956160059102, 6.002748559000014694 ) ) ;
#8558 = CARTESIAN_POINT ( 'NONE',  ( -23.76534794678204321, -14.42397063190348483, 6.095965061000018892 ) ) ;
#8559 = CARTESIAN_POINT ( 'NONE',  ( 21.13530760622424864, 17.06006193249097436, 0.000000000000000000 ) ) ;
#8560 = B_SPLINE_CURVE_WITH_KNOTS ( 'NONE', 5,
 ( #26212, #28571, #25753, #21490, #9056, #23554, #31087, #4646, #28251 ),
 .UNSPECIFIED., .F., .F.,
 ( 6, 3, 6 ),
 ( 0.000000000000000000, 18.10919428740000114, 32.96201648640000315 ),
 .UNSPECIFIED. ) ;
#8561 = FACE_OUTER_BOUND ( 'NONE', #4846, .T. ) ;
#8562 = CARTESIAN_POINT ( 'NONE',  ( -5.712565024699335581, -0.3554524910389447734, -44.56408784452499816 ) ) ;
#8563 = CARTESIAN_POINT ( 'NONE',  ( -11.69999999989999928, -24.11120071670000087, -0.6999999999999992895 ) ) ;
#8564 = CARTESIAN_POINT ( 'NONE',  ( 27.54391552369999729, -3.373045395939999845E-15, 142.9562530130000084 ) ) ;
#8565 = ORIENTED_EDGE ( 'NONE', *, *, #1020, .F. ) ;
#8566 = CARTESIAN_POINT ( 'NONE',  ( 24.92013865993870425, -13.82966158318416738, 3.899998581000013509 ) ) ;
#8567 = CARTESIAN_POINT ( 'NONE',  ( 10.82908725742651512, -27.76276047461856322, 93.21714158839999698 ) ) ;
#8568 = CARTESIAN_POINT ( 'NONE',  ( 2.819655859569989431, -3.689021998396972979, -68.10000000002499121 ) ) ;
#8569 = CARTESIAN_POINT ( 'NONE',  ( 26.56187606716263971, 4.248286909032550795, -0.6999999999999784173 ) ) ;
#8570 = CARTESIAN_POINT ( 'NONE',  ( -24.14619884830422336, -13.16136950053335752, 225.8804910025767185 ) ) ;
#8571 = AXIS2_PLACEMENT_3D ( 'NONE', #24031, #2164, #6868 ) ;
#8572 = FILL_AREA_STYLE ('',( #12993 ) ) ;
#8573 = DIRECTION ( 'NONE',  ( -0.5532886644841250590, -0.8329895880221872551, 0.000000000000000000 ) ) ;
#8574 = CARTESIAN_POINT ( 'NONE',  ( 27.50000000000000000, -1.776356839399999804E-15, 136.3944487250000179 ) ) ;
#8575 = CARTESIAN_POINT ( 'NONE',  ( 2.994727039187461415, -3.426347720743794234, -64.49605006312501132 ) ) ;
#8576 = ORIENTED_EDGE ( 'NONE', *, *, #2925, .F. ) ;
#8577 = CARTESIAN_POINT ( 'NONE',  ( 18.67857132407096188, 19.99999793005311943, 230.6030643836558340 ) ) ;
#8578 = ORIENTED_EDGE ( 'NONE', *, *, #18385, .F. ) ;
#8579 = CARTESIAN_POINT ( 'NONE',  ( -26.95947219337181266, -7.589290548446620654, 0.02487529600000981667 ) ) ;
#8580 = ORIENTED_EDGE ( 'NONE', *, *, #20258, .F. ) ;
#8581 = CARTESIAN_POINT ( 'NONE',  ( 16.19548821478059963, -8.463596681405142874, -4.336808689942018722E-16 ) ) ;
#8582 = EDGE_CURVE ( 'NONE', #28608, #2437, #30943, .T. ) ;
#8583 = B_SPLINE_CURVE_WITH_KNOTS ( 'NONE', 1,
 ( #13431, #1803 ),
 .UNSPECIFIED., .F., .F.,
 ( 2, 2 ),
 ( -2.556331278550000249E-06, 0.7000000000009999335 ),
 .UNSPECIFIED. ) ;
#8584 = FACE_OUTER_BOUND ( 'NONE', #28042, .T. ) ;
#8585 = DIRECTION ( 'NONE',  ( 0.000000000000000000, 0.000000000000000000, -1.000000000000000000 ) ) ;
#8586 = CARTESIAN_POINT ( 'NONE',  ( -3.503013490857829204, -0.9326026542299333810, 230.7640337244225464 ) ) ;
#8587 = DIRECTION ( 'NONE',  ( -2.965499939100700266E-25, -1.000000000000000000, 2.257145581549900232E-12 ) ) ;
#8588 = FACE_OUTER_BOUND ( 'NONE', #19396, .T. ) ;
#8589 = CARTESIAN_POINT ( 'NONE',  ( -9.000000000229999131, 20.99999999999999645, -56.09999999999999432 ) ) ;
#8590 = VERTEX_POINT ( 'NONE', #19722 ) ;
#8591 = CARTESIAN_POINT ( 'NONE',  ( -1.027511273769999933E-13, -27.50000000000000000, 115.0000000000000000 ) ) ;
#8592 = CARTESIAN_POINT ( 'NONE',  ( -24.49999999589999788, 3.000285566369999841E-15, 140.0000000000000000 ) ) ;
#8593 = EDGE_CURVE ( 'NONE', #16796, #21922, #26793, .T. ) ;
#8594 = FACE_OUTER_BOUND ( 'NONE', #30347, .T. ) ;
#8595 = CARTESIAN_POINT ( 'NONE',  ( -3.574293702744737455, 0.8091417056767529203, 230.7417114753004341 ) ) ;
#8596 = CIRCLE ( 'NONE', #26710, 27.23548387060000309 ) ;
#8597 = CYLINDRICAL_SURFACE ( 'NONE', #25204, 3.000000000000000444 ) ;
#8598 = CARTESIAN_POINT ( 'NONE',  ( -15.86808677770000209, -9.527368092500001495, -0.7000000003999986564 ) ) ;
#8599 = CARTESIAN_POINT ( 'NONE',  ( -25.46368746804859740, 12.80129684245613575, 4.999998581000003384 ) ) ;
#8600 = CARTESIAN_POINT ( 'NONE',  ( 26.97469346668950152, -9.357175201752722771, 0.000000000000000000 ) ) ;
#8601 = CARTESIAN_POINT ( 'NONE',  ( 4.669144396295984656, -2.892150817486062397, -48.53324460762500081 ) ) ;
#8602 = CARTESIAN_POINT ( 'NONE',  ( 27.77052805885498898, 0.5052956280874453254, 0.7069222069999991920 ) ) ;
#8603 = CARTESIAN_POINT ( 'NONE',  ( 14.74121624851424528, -28.30819945631988332, -33.41822227976423676 ) ) ;
#8604 = CARTESIAN_POINT ( 'NONE',  ( 3.676328827952111578, -0.6318780627718988407, 230.7123227554324956 ) ) ;
#8605 = B_SPLINE_CURVE_WITH_KNOTS ( 'NONE', 5,
 ( #2301, #31085, #9525, #7164, #12647, #29646, #12963, #26976, #8073, #20358, #7772, #15329, #5566, #24771, #17669 ),
 .UNSPECIFIED., .F., .F.,
 ( 6, 3, 3, 3, 6 ),
 ( 0.000000000000000000, 0.1000000000011452422, 0.3999999999988547161, 0.6999999999994274136, 1.000000000000000000 ),
 .UNSPECIFIED. ) ;
#8606 = FACE_OUTER_BOUND ( 'NONE', #10678, .T. ) ;
#8607 = VERTEX_POINT ( 'NONE', #16612 ) ;
#8608 = CARTESIAN_POINT ( 'NONE',  ( 3.471037982653067733, 3.337515987827158526, -36.26091724619999468 ) ) ;
#8609 = ORIENTED_EDGE ( 'NONE', *, *, #19711, .F. ) ;
#8610 = EDGE_CURVE ( 'NONE', #7544, #22213, #4848, .T. ) ;
#8611 = CARTESIAN_POINT ( 'NONE',  ( -4.180007949804073419, -3.103635835586971758, -57.07895058492500340 ) ) ;
#8612 = ORIENTED_EDGE ( 'NONE', *, *, #22290, .F. ) ;
#8613 = APPLICATION_PROTOCOL_DEFINITION ( 'draft international standard', 'automotive_design', 1998, #3966 ) ;
#8614 = VECTOR ( 'NONE', #17721, 1000.000000000000000 ) ;
#8615 = B_SPLINE_CURVE_WITH_KNOTS ( 'NONE', 3,
 ( #17147, #7702, #4737, #23949, #11970, #9451, #497, #17304, #7556, #19524, #28651, #21581, #28, #21727, #10852, #8155, #17751, #10542, #17907, #5655, #19977, #27215, #15254, #29881, #797, #1094, #13044, #29573, #10386, #20281, #6116, #27670, #8312, #22502, #647, #3596, #22804, #20137, #24553, #2992, #27514, #12737, #13190, #25007, #7853, #18065, #8009, #29727, #8468, #22651, #10235, #17607, #24863, #5960, #29417, #15107, #19835, #3292, #952, #27370, #30035, #12896, #5810, #15408, #3441, #22346, #10685, #15554, #25164, #17456, #27062, #1255, #12582, #20438, #22190, #5500, #24702, #3138, #11320, #20753, #20918, #1412, #30360 ),
 .UNSPECIFIED., .F., .F.,
 ( 4, 2, 2, 1, 1, 1, 2, 2, 1, 1, 1, 1, 1, 2, 2, 1, 1, 1, 1, 2, 2, 1, 1, 1, 1, 1, 2, 2, 1, 1, 2, 2, 1, 1, 1, 1, 2, 2, 1, 1, 1, 2, 2, 1, 1, 2, 2, 2, 2, 1, 1, 2, 2, 1, 2, 2, 4 ),
 ( 0.000000000000000000, 0.06249999999999655831, 0.1249999999999931166, 0.1874999999999896749, 0.2187499999999879541, 0.2343749999999871214, 0.2421874999999866773, 0.2499999999999862332, 0.3124999999999829026, 0.3437499999999812372, 0.3593749999999803491, 0.3671874999999799605, 0.3710937499999797384, 0.3730468749999796274, 0.3749999999999795164, 0.4062499999999776290, 0.4218749999999767408, 0.4296874999999762967, 0.4335937499999760747, 0.4355468749999759637, 0.4374999999999758526, 0.4531249999999749090, 0.4609374999999744649, 0.4648437499999742428, 0.4667968749999741873, 0.4677734374999740763, 0.4682617187499739653, 0.4687499999999739098, 0.4843749999999711342, 0.4921874999999697464, 0.4960937499999689693, 0.4999999999999681921, 0.5156249999999658051, 0.5234374999999645839, 0.5273437499999639178, 0.5292968749999636957, 0.5302734374999636957, 0.5312499999999636957, 0.5468749999999640288, 0.5546874999999642508, 0.5585937499999643618, 0.5605468749999643618, 0.5624999999999643618, 0.5937499999999672484, 0.6093749999999685807, 0.6171874999999692468, 0.6249999999999699130, 0.6562499999999723554, 0.6874999999999749090, 0.7187499999999773515, 0.7343749999999786837, 0.7421874999999792388, 0.7499999999999797939, 0.8124999999999847899, 0.8437499999999872324, 0.8749999999999897859, 1.000000000000000000 ),
 .UNSPECIFIED. ) ;
#8616 = ORIENTED_EDGE ( 'NONE', *, *, #4999, .F. ) ;
#8617 = ORIENTED_EDGE ( 'NONE', *, *, #2913, .F. ) ;
#8618 = VECTOR ( 'NONE', #30274, 1000.000000000000114 ) ;
#8619 = CARTESIAN_POINT ( 'NONE',  ( 14.74927456580506835, -30.64616432563845549, -24.73190548423032453 ) ) ;
#8620 = DIRECTION ( 'NONE',  ( 0.000000000000000000, 0.000000000000000000, -1.000000000000000000 ) ) ;
#8621 = DIRECTION ( 'NONE',  ( 5.962915006522623408E-16, 0.4383711467890811231, 0.8987940462991652613 ) ) ;
#8622 = DIRECTION ( 'NONE',  ( 0.000000000000000000, 0.000000000000000000, 1.000000000000000000 ) ) ;
#8623 = CARTESIAN_POINT ( 'NONE',  ( -0.8184510532230938606, -27.48788286177401474, 4.263459062314771231 ) ) ;
#8624 = DIRECTION ( 'NONE',  ( 0.000000000000000000, 0.000000000000000000, -1.000000000000000000 ) ) ;
#8625 = CARTESIAN_POINT ( 'NONE',  ( 2.914708617673698932, -3.631324690002109445, -3.105321867099997135 ) ) ;
#8626 = CARTESIAN_POINT ( 'NONE',  ( -3.873164306258084277, -2.119290473559455101, -95.69213427732501032 ) ) ;
#8627 = DIRECTION ( 'NONE',  ( 0.7071067811865475727, 0.7071067811865475727, 0.000000000000000000 ) ) ;
#8628 = EDGE_CURVE ( 'NONE', #2523, #12147, #5229, .T. ) ;
#8629 = CARTESIAN_POINT ( 'NONE',  ( 1.387648159808044790, -4.113210426322153168, -15.76414732019999931 ) ) ;
#8630 = CARTESIAN_POINT ( 'NONE',  ( -4.339197174995631734, 0.6278332542688225271, -34.25783976329999092 ) ) ;
#8631 = MECHANICAL_DESIGN_GEOMETRIC_PRESENTATION_REPRESENTATION (  '', ( #22222 ), #15178 ) ;
#8632 = VECTOR ( 'NONE', #20526, 1000.000000000000000 ) ;
#8633 = DIRECTION ( 'NONE',  ( 0.000000000000000000, 1.000000000000000000, 0.000000000000000000 ) ) ;
#8634 = CARTESIAN_POINT ( 'NONE',  ( 27.29371452669260734, 0.4966198192113280285, -0.6577119969999878357 ) ) ;
#8635 = CARTESIAN_POINT ( 'NONE',  ( 0.6521647004709999473, -27.79285400239999859, 224.0990955869999937 ) ) ;
#8636 = CARTESIAN_POINT ( 'NONE',  ( -23.76243112480983655, -16.20069438324207667, 8.000000000000007105 ) ) ;
#8637 = LINE ( 'NONE', #16198, #20771 ) ;
#8638 = CARTESIAN_POINT ( 'NONE',  ( 22.68420274108862245, -14.27219891852400302, 225.4229804109004931 ) ) ;
#8639 = CARTESIAN_POINT ( 'NONE',  ( -9.599333685411828299, -15.14023671560908646, -74.38892505318962378 ) ) ;
#8640 = CARTESIAN_POINT ( 'NONE',  ( 2.020725942159999899, -3.500000000000000000, 227.9588918784999976 ) ) ;
#8641 = VERTEX_POINT ( 'NONE', #30787 ) ;
#8642 = EDGE_CURVE ( 'NONE', #1273, #15181, #1872, .T. ) ;
#8643 = EDGE_CURVE ( 'NONE', #24657, #17664, #14970, .T. ) ;
#8644 = CARTESIAN_POINT ( 'NONE',  ( 24.16679028237082960, 15.10730797463399000, 6.002747145999992817 ) ) ;
#8645 = LINE ( 'NONE', #13377, #15756 ) ;
#8646 = ORIENTED_EDGE ( 'NONE', *, *, #15294, .T. ) ;
#8647 = CARTESIAN_POINT ( 'NONE',  ( -23.16113320663907160, -13.48374052519065813, 223.9000000000012562 ) ) ;
#8648 = DIRECTION ( 'NONE',  ( 0.000000000000000000, -1.000000000000000000, 0.000000000000000000 ) ) ;
#8649 = CARTESIAN_POINT ( 'NONE',  ( 0.09707315090956633585, -26.79999999950001310, 3.899999999999991473 ) ) ;
#8650 = VERTEX_POINT ( 'NONE', #6857 ) ;
#8651 = CARTESIAN_POINT ( 'NONE',  ( 9.000000000000000000, -130.0000000000000000, -42.39999999999999858 ) ) ;
#8652 = EDGE_LOOP ( 'NONE', ( #20799, #1939, #20934, #22526 ) ) ;
#8653 = ORIENTED_EDGE ( 'NONE', *, *, #27360, .F. ) ;
#8654 = ADVANCED_FACE ( 'NONE', ( #17501 ), #16468, .T. ) ;
#8655 = SHAPE_REPRESENTATION_RELATIONSHIP ( 'NONE' , 'NONE' ,  #25228, #4675 ) ;
#8656 = ORIENTED_EDGE ( 'NONE', *, *, #29853, .T. ) ;
#8657 = CARTESIAN_POINT ( 'NONE',  ( -23.24663841809999809, -14.69162354060000020, 225.0000000000000000 ) ) ;
#8658 = ORIENTED_EDGE ( 'NONE', *, *, #26240, .F. ) ;
#8659 = B_SPLINE_CURVE_WITH_KNOTS ( 'NONE', 5,
 ( #7458, #9665, #30763, #86, #239, #19422 ),
 .UNSPECIFIED., .F., .F.,
 ( 6, 6 ),
 ( 0.000000000000000000, 21.63799706120000010 ),
 .UNSPECIFIED. ) ;
#8660 = CIRCLE ( 'NONE', #12682, 2.000000000000002220 ) ;
#8661 = CARTESIAN_POINT ( 'NONE',  ( 5.114250173790000353, 17.43050733020000109, 230.6999999999999886 ) ) ;
#8662 = ORIENTED_EDGE ( 'NONE', *, *, #18864, .F. ) ;
#8663 = CARTESIAN_POINT ( 'NONE',  ( 7.999999999949441332, -116.5561065468434947, 18.74526241744673172 ) ) ;
#8664 = CARTESIAN_POINT ( 'NONE',  ( -0.5716039299945605556, -28.49445895580190324, 5.310182064000024127 ) ) ;
#8665 = ADVANCED_FACE ( 'NONE', ( #10277 ), #27791, .T. ) ;
#8666 = CARTESIAN_POINT ( 'NONE',  ( -26.80000000000000071, 6.217248937899999413E-15, 136.7828584120000244 ) ) ;
#8667 = CARTESIAN_POINT ( 'NONE',  ( 23.48532359031332462, -12.91116100182251714, 5.957452580039663381 ) ) ;
#8668 = CARTESIAN_POINT ( 'NONE',  ( -1.089818731930000117, -28.47945802909999813, 225.3102023309999993 ) ) ;
#8669 = ORIENTED_EDGE ( 'NONE', *, *, #20661, .T. ) ;
#8670 = CARTESIAN_POINT ( 'NONE',  ( 2.914708617673689606, -3.631324690002112110, -3.605321867100001576 ) ) ;
#8671 = CARTESIAN_POINT ( 'NONE',  ( 0.2309929099465271585, 4.358477053493584386, -22.94418644579999977 ) ) ;
#8672 = CARTESIAN_POINT ( 'NONE',  ( -9.799563951679274965, -25.69477015992461233, 203.8298458494338661 ) ) ;
#8673 = LINE ( 'NONE', #3968, #24073 ) ;
#8674 = CARTESIAN_POINT ( 'NONE',  ( -2.091444806098883280, -2.888061030879386593, -88.52261276293990022 ) ) ;
#8675 = CARTESIAN_POINT ( 'NONE',  ( -24.62438106040000108, 13.65981548289999914, 230.5592437530000041 ) ) ;
#8676 = CARTESIAN_POINT ( 'NONE',  ( -25.45015929631789220, 12.82831286024188699, 5.290680260628121800 ) ) ;
#8677 = CARTESIAN_POINT ( 'NONE',  ( -2.400531359713943491, -2.916784241273735923, -0.7578093795000060418 ) ) ;
#8678 = EDGE_CURVE ( 'NONE', #30538, #23803, #27976, .T. ) ;
#8679 = CARTESIAN_POINT ( 'NONE',  ( 4.276011752472853367, -103.0613381315207988, 16.56805218640185018 ) ) ;
#8680 = CARTESIAN_POINT ( 'NONE',  ( 16.58809447609999665, 7.862979437299999041, 230.6999999999999886 ) ) ;
#8681 = ORIENTED_EDGE ( 'NONE', *, *, #22943, .F. ) ;
#8682 = CARTESIAN_POINT ( 'NONE',  ( 5.896017893897736784, 2.415859114112482775, -60.41141554682499759 ) ) ;
#8683 = DIRECTION ( 'NONE',  ( 5.962915006522622422E-16, 0.4383711467890810676, 0.8987940462991651502 ) ) ;
#8684 = ORIENTED_EDGE ( 'NONE', *, *, #10588, .T. ) ;
#8685 = CARTESIAN_POINT ( 'NONE',  ( -6.505526340826822462, -0.4164809035224065203, -4.148838774900000637 ) ) ;
#8686 = EDGE_LOOP ( 'NONE', ( #19715, #24689, #17839, #9706 ) ) ;
#8687 = CARTESIAN_POINT ( 'NONE',  ( 21.71012070049999920, 18.50699920749999805, 224.9999999359999947 ) ) ;
#8688 = DIRECTION ( 'NONE',  ( 0.3633921898465274913, -0.9316362575375355393, 0.000000000000000000 ) ) ;
#8689 = ORIENTED_EDGE ( 'NONE', *, *, #1992, .F. ) ;
#8690 = CARTESIAN_POINT ( 'NONE',  ( 10.99289321870000080, 19.99999999999999645, -1.692893218799999877 ) ) ;
#8691 = EDGE_LOOP ( 'NONE', ( #1662, #4262, #11034, #8578 ) ) ;
#8692 = ORIENTED_EDGE ( 'NONE', *, *, #623, .F. ) ;
#8693 = CARTESIAN_POINT ( 'NONE',  ( 24.34660549313368705, -12.78643034496831277, 4.854326830101610923 ) ) ;
#8694 = SURFACE_STYLE_USAGE ( .BOTH. , #6502 ) ;
#8695 = EDGE_LOOP ( 'NONE', ( #3205, #13573, #20980, #24626, #17598 ) ) ;
#8696 = CARTESIAN_POINT ( 'NONE',  ( -12.29999999981408720, -24.20388355726637641, -30.01158073719771480 ) ) ;
#8697 = DIRECTION ( 'NONE',  ( -0.000000000000000000, 1.000000000000000000, -2.257145581549999994E-12 ) ) ;
#8698 = VECTOR ( 'NONE', #1465, 1000.000000000000000 ) ;
#8699 = CARTESIAN_POINT ( 'NONE',  ( 1.644051155559919764, -5.677575162961061572, -67.22367649362500686 ) ) ;
#8700 = CIRCLE ( 'NONE', #15729, 1.119823175164191165 ) ;
#8701 = CARTESIAN_POINT ( 'NONE',  ( 27.77512470400000311, -7.276253507709999901, 229.2930777930000090 ) ) ;
#8702 = AXIS2_PLACEMENT_3D ( 'NONE', #30216, #25187, #10876 ) ;
#8703 = CARTESIAN_POINT ( 'NONE',  ( -7.999999999693026886, -27.86619909554637786, -31.29895010234936947 ) ) ;
#8704 = EDGE_CURVE ( 'NONE', #2756, #15244, #13974, .T. ) ;
#8705 = FACE_OUTER_BOUND ( 'NONE', #17782, .T. ) ;
#8706 = VECTOR ( 'NONE', #11011, 1000.000000000000000 ) ;
#8707 = CARTESIAN_POINT ( 'NONE',  ( -17.40850972537708330, -23.44589038181687712, -24.67846847529753518 ) ) ;
#8708 = ORIENTED_EDGE ( 'NONE', *, *, #21800, .T. ) ;
#8709 = CARTESIAN_POINT ( 'NONE',  ( -13.99999999969999820, 20.99999999999999645, -58.51619611000000276 ) ) ;
#8710 = EDGE_CURVE ( 'NONE', #22335, #29610, #29241, .T. ) ;
#8711 = CARTESIAN_POINT ( 'NONE',  ( 2.789765316938662476, -3.934254546267435426, -11.18638893669999668 ) ) ;
#8712 = CARTESIAN_POINT ( 'NONE',  ( -17.49999999969999820, -27.00000000000000000, -28.40000000020000215 ) ) ;
#8713 = EDGE_CURVE ( 'NONE', #22798, #11502, #7917, .T. ) ;
#8714 = CARTESIAN_POINT ( 'NONE',  ( -28.49528339128749366, -0.5184828350247674411, 1.000000000000000888 ) ) ;
#8715 = ORIENTED_EDGE ( 'NONE', *, *, #29248, .F. ) ;
#8716 = CARTESIAN_POINT ( 'NONE',  ( 24.30716200859999887, -13.49132717699999873, 223.9972514410000031 ) ) ;
#8717 = CARTESIAN_POINT ( 'NONE',  ( -22.64694720645078263, -14.33102249094126890, 4.781948427652641165 ) ) ;
#8718 = DIRECTION ( 'NONE',  ( 0.7071067811865475727, -0.7071067811865475727, 0.000000000000000000 ) ) ;
#8719 = CARTESIAN_POINT ( 'NONE',  ( 17.93344943624471810, 20.10553870840068313, 0.000000000000000000 ) ) ;
#8720 = CARTESIAN_POINT ( 'NONE',  ( 8.700000000236576270, -29.80249410823907752, -29.47052640017699687 ) ) ;
#8721 = CARTESIAN_POINT ( 'NONE',  ( -1.256295066205788347, -5.815478746186413694, -55.93033560642499680 ) ) ;
#8722 = DIRECTION ( 'NONE',  ( -1.000000000000000000, 0.000000000000000000, 0.000000000000000000 ) ) ;
#8723 = DIRECTION ( 'NONE',  ( -1.000000000000000000, 5.063197998645201881E-16, -2.257212216166322864E-12 ) ) ;
#8724 = AXIS2_PLACEMENT_3D ( 'NONE', #30888, #24117, #2555 ) ;
#8725 = EDGE_LOOP ( 'NONE', ( #19863, #11853, #30126, #7655 ) ) ;
#8726 = CARTESIAN_POINT ( 'NONE',  ( 24.88589369718092215, -13.89120818692358483, 3.904029272000009154 ) ) ;
#8727 = CARTESIAN_POINT ( 'NONE',  ( 22.83442928010000017, 16.43389279790000046, 226.2000000000000171 ) ) ;
#8728 = VECTOR ( 'NONE', #16661, 1000.000000000000114 ) ;
#8729 = VECTOR ( 'NONE', #5249, 1000.000000000000000 ) ;
#8730 = TOROIDAL_SURFACE ( 'NONE', #30843, 24.50000000000000000, 4.000000000000000000 ) ;
#8731 = CARTESIAN_POINT ( 'NONE',  ( 2.571935351011521487, -3.481578157327508194, -68.10000000002500542 ) ) ;
#8732 = B_SPLINE_CURVE_WITH_KNOTS ( 'NONE', 5,
 ( #13871, #20636, #11507, #30231, #25682, #15596, #1763, #20950, #6318, #5999, #15912, #13711, #6622, #25521, #23479 ),
 .UNSPECIFIED., .F., .F.,
 ( 6, 3, 3, 3, 6 ),
 ( 0.000000000000000000, 0.5239017171269999551, 1.047803434249999999, 1.571705151379999998, 1.746339057089999924 ),
 .UNSPECIFIED. ) ;
#8733 = CYLINDRICAL_SURFACE ( 'NONE', #17768, 1.099999999999999867 ) ;
#8734 = CARTESIAN_POINT ( 'NONE',  ( -24.34660549313262834, -12.78643034497033781, 225.1456731698328895 ) ) ;
#8735 = DIRECTION ( 'NONE',  ( 0.000000000000000000, 0.3420201433259318913, -0.9396926207858126157 ) ) ;
#8736 = DIRECTION ( 'NONE',  ( -1.000000000000000000, -7.807837518030243978E-13, -2.626330150303133688E-12 ) ) ;
#8737 = CARTESIAN_POINT ( 'NONE',  ( -4.469650141049659631, 2.071768678095493588, -66.52526299432499002 ) ) ;
#8738 = VERTEX_POINT ( 'NONE', #9234 ) ;
#8739 = CARTESIAN_POINT ( 'NONE',  ( 18.94383107422812174, 20.00027397745331115, 230.5276813009044474 ) ) ;
#8740 = ORIENTED_EDGE ( 'NONE', *, *, #21680, .T. ) ;
#8741 = CARTESIAN_POINT ( 'NONE',  ( -24.50654363593514873, -14.64341241029205065, 0.02487534799999746582 ) ) ;
#8742 = ORIENTED_EDGE ( 'NONE', *, *, #16365, .T. ) ;
#8743 = CARTESIAN_POINT ( 'NONE',  ( -11.02757632650000019, -24.42656469639999983, -0.8308237180999975546 ) ) ;
#8744 =( GEOMETRIC_REPRESENTATION_CONTEXT ( 3 ) GLOBAL_UNCERTAINTY_ASSIGNED_CONTEXT ( ( #21656 ) ) GLOBAL_UNIT_ASSIGNED_CONTEXT ( ( #620, #5931, #5781 ) ) REPRESENTATION_CONTEXT ( 'NONE', 'WORKASPACE' ) );
#8745 = VECTOR ( 'NONE', #28596, 1000.000000000000000 ) ;
#8746 = DIRECTION ( 'NONE',  ( 0.000000000000000000, -0.3420201433259318358, 0.9396926207858125046 ) ) ;
#8747 = DIRECTION ( 'NONE',  ( 1.000000000000000000, 0.000000000000000000, 0.000000000000000000 ) ) ;
#8748 = VECTOR ( 'NONE', #8204, 1000.000000000000000 ) ;
#8749 = ADVANCED_FACE ( 'NONE', ( #21060 ), #8907, .F. ) ;
#8750 = VECTOR ( 'NONE', #25131, 1000.000000000000000 ) ;
#8751 = CARTESIAN_POINT ( 'NONE',  ( -17.39611244578438232, -23.36667610088668212, -32.07580216089276348 ) ) ;
#8752 = CARTESIAN_POINT ( 'NONE',  ( -12.48017473518528320, -22.00000000000000000, -30.22182049597928000 ) ) ;
#8753 = EDGE_CURVE ( 'NONE', #18996, #18573, #27504, .T. ) ;
#8754 = CARTESIAN_POINT ( 'NONE',  ( -15.44356573478999906, -26.99999999999999289, -28.40000000003218972 ) ) ;
#8755 = VERTEX_POINT ( 'NONE', #17099 ) ;
#8756 = CYLINDRICAL_SURFACE ( 'NONE', #933, 2.000000000000003553 ) ;
#8757 = FACE_OUTER_BOUND ( 'NONE', #18696, .T. ) ;
#8758 = CYLINDRICAL_SURFACE ( 'NONE', #21839, 2.500000000000001776 ) ;
#8759 = CYLINDRICAL_SURFACE ( 'NONE', #15261, 3.000000000000002220 ) ;
#8760 = CARTESIAN_POINT ( 'NONE',  ( -24.64674669160000064, -14.31123007319999907, 226.0986578890000089 ) ) ;
#8761 = CYLINDRICAL_SURFACE ( 'NONE', #27580, 0.9999999999999988898 ) ;
#8762 = CARTESIAN_POINT ( 'NONE',  ( -1.071601127040515022, -27.47917021046086106, 225.2867514115019674 ) ) ;
#8763 = CARTESIAN_POINT ( 'NONE',  ( -11.49999999969999998, -27.00000000000000000, -28.40000000000541647 ) ) ;
#8764 = CARTESIAN_POINT ( 'NONE',  ( -0.9106536557280191513, 5.366613064759778950, -50.45792092402500373 ) ) ;
#8765 = CARTESIAN_POINT ( 'NONE',  ( 10.00166578780910065, 20.99999999999306155, -54.17273359987459003 ) ) ;
#8766 = CARTESIAN_POINT ( 'NONE',  ( 7.545803529383563024, 4.488346928486736331, -39.66828223693498501 ) ) ;
#8767 = FACE_OUTER_BOUND ( 'NONE', #5835, .T. ) ;
#8768 = AXIS2_PLACEMENT_3D ( 'NONE', #5704, #17655, #20337 ) ;
#8769 = VECTOR ( 'NONE', #13812, 1000.000000000000114 ) ;
#8770 = AXIS2_PLACEMENT_3D ( 'NONE', #9488, #21455, #12005 ) ;
#8771 = DIRECTION ( 'NONE',  ( 0.000000000000000000, -1.000000000000000000, 0.000000000000000000 ) ) ;
#8772 = ORIENTED_EDGE ( 'NONE', *, *, #27638, .T. ) ;
#8773 = CARTESIAN_POINT ( 'NONE',  ( 4.373195337096333013, -2.904765488536246387, -35.95875473020000612 ) ) ;
#8774 = ORIENTED_EDGE ( 'NONE', *, *, #17309, .F. ) ;
#8775 = CARTESIAN_POINT ( 'NONE',  ( 5.655353257545034040, 0.6391371982505194005, -55.81771407622498771 ) ) ;
#8776 = ORIENTED_EDGE ( 'NONE', *, *, #14020, .F. ) ;
#8777 = EDGE_CURVE ( 'NONE', #15341, #24264, #29204, .T. ) ;
#8778 = ORIENTED_EDGE ( 'NONE', *, *, #15831, .T. ) ;
#8779 =( REPRESENTATION_RELATIONSHIP ('NONE','NONE', #2712, #527 ) REPRESENTATION_RELATIONSHIP_WITH_TRANSFORMATION ( #21210 )SHAPE_REPRESENTATION_RELATIONSHIP( ) );
#8780 = ORIENTED_EDGE ( 'NONE', *, *, #3399, .T. ) ;
#8781 = AXIS2_PLACEMENT_3D ( 'NONE', #8712, #18318, #23679 ) ;
#8782 =( GEOMETRIC_REPRESENTATION_CONTEXT ( 3 ) GLOBAL_UNCERTAINTY_ASSIGNED_CONTEXT ( ( #9686 ) ) GLOBAL_UNIT_ASSIGNED_CONTEXT ( ( #23356, #27741, #13588 ) ) REPRESENTATION_CONTEXT ( 'NONE', 'WORKASPACE' ) );
#8783 = PRESENTATION_STYLE_ASSIGNMENT (( #20748 ) ) ;
#8784 = CARTESIAN_POINT ( 'NONE',  ( -17.83928249649999742, 19.99999999999999645, -1.049999999600002898 ) ) ;
#8785 = CARTESIAN_POINT ( 'NONE',  ( -9.974508415446116771, -129.9999999999999716, -42.66064002661978094 ) ) ;
#8786 = DIRECTION ( 'NONE',  ( 0.000000000000000000, 0.000000000000000000, 1.000000000000000000 ) ) ;
#8787 = CARTESIAN_POINT ( 'NONE',  ( 17.93011078765611543, -8.208160914697428368, 0.000000000000000000 ) ) ;
#8788 = CARTESIAN_POINT ( 'NONE',  ( -0.1113126277073478027, 4.304903297084355707, -39.57881079973518723 ) ) ;
#8789 = CARTESIAN_POINT ( 'NONE',  ( -5.111484982110231279, -0.3272349956394805526, -3.211338774900002413 ) ) ;
#8790 = CARTESIAN_POINT ( 'NONE',  ( 0.000000000000000000, 0.000000000000000000, 90.00000000000000000 ) ) ;
#8791 = CARTESIAN_POINT ( 'NONE',  ( 25.35557883893859810, -13.01417686066516488, 5.679894690497184762 ) ) ;
#8792 = VECTOR ( 'NONE', #520, 1000.000000000000000 ) ;
#8793 = CARTESIAN_POINT ( 'NONE',  ( -2.970579505556664834, -5.081274235795743444, -16.68182079290001241 ) ) ;
#8794 = CARTESIAN_POINT ( 'NONE',  ( 3.436082050571383828, -2.282315740991611719, -35.02125473019999902 ) ) ;
#8795 = B_SPLINE_CURVE_WITH_KNOTS ( 'NONE', 3,
 ( #24525, #29391, #10661, #10361, #29851, #22777, #29545, #17580, #3416, #5932, #5626, #7828 ),
 .UNSPECIFIED., .F., .F.,
 ( 4, 2, 2, 2, 2, 4 ),
 ( 0.000000000000000000, 0.1249999999999845124, 0.2499999999999690248, 0.4999999999999793499, 0.7499999999999896749, 1.000000000000000000 ),
 .UNSPECIFIED. ) ;
#8796 = B_SPLINE_CURVE_WITH_KNOTS ( 'NONE', 3,
 ( #2019, #1553, #18377, #11609, #21206, #27973, #6417, #9233, #18841, #13657 ),
 .UNSPECIFIED., .F., .F.,
 ( 4, 2, 2, 2, 4 ),
 ( 0.000000000000000000, 0.2500000000000000000, 0.5000000000000000000, 0.7500000000000000000, 1.000000000000000000 ),
 .UNSPECIFIED. ) ;
#8797 = CARTESIAN_POINT ( 'NONE',  ( -4.276011752264103016, -102.7755780389424416, 17.20706796824344309 ) ) ;
#8798 = CARTESIAN_POINT ( 'NONE',  ( 28.49528339128749366, 0.5184828350247745465, 1.000000000000000888 ) ) ;
#8799 = CARTESIAN_POINT ( 'NONE',  ( 1.099998580829999906, -27.77839262550000043, 225.0000014190000002 ) ) ;
#8800 = CARTESIAN_POINT ( 'NONE',  ( 14.96238942309071085, -23.61101023361229068, 8.000000000000007105 ) ) ;
#8801 = LINE ( 'NONE', #6599, #22280 ) ;
#8802 = CARTESIAN_POINT ( 'NONE',  ( 8.700000000232341435, -25.77531388888509056, -25.66136093477824431 ) ) ;
#8803 = CARTESIAN_POINT ( 'NONE',  ( -3.097451722119552997, -1.692897434402192092, 226.6412452697750268 ) ) ;
#8804 = CARTESIAN_POINT ( 'NONE',  ( -19.80535357377644701, 19.50875577052588739, 3.000000106999994642 ) ) ;
#8805 = AXIS2_PLACEMENT_3D ( 'NONE', #26342, #19568, #12327 ) ;
#8806 = EDGE_CURVE ( 'NONE', #2098, #29682, #20486, .T. ) ;
#8807 = PLANE ( 'NONE',  #25312 ) ;
#8808 = VERTEX_POINT ( 'NONE', #3085 ) ;
#8809 = CARTESIAN_POINT ( 'NONE',  ( 4.638687372303289536, 6.462009008358804429, -40.63090155166024431 ) ) ;
#8810 = CARTESIAN_POINT ( 'NONE',  ( -25.22658730140000216, -13.26242337740000110, 225.0000014190000002 ) ) ;
#8811 = CARTESIAN_POINT ( 'NONE',  ( 0.9876146829922234360, -26.78228247995595979, 4.508624923504668480 ) ) ;
#8812 = VERTEX_POINT ( 'NONE', #19156 ) ;
#8813 = CARTESIAN_POINT ( 'NONE',  ( -10.00000000009948309, -128.1247626082301565, -35.28103264363292624 ) ) ;
#8814 = ORIENTED_EDGE ( 'NONE', *, *, #17463, .F. ) ;
#8815 = EDGE_CURVE ( 'NONE', #13541, #27946, #4461, .T. ) ;
#8816 = EDGE_LOOP ( 'NONE', ( #26893, #29941, #17028, #29591 ) ) ;
#8817 = ORIENTED_EDGE ( 'NONE', *, *, #27081, .T. ) ;
#8818 = DIRECTION ( 'NONE',  ( -1.000000000000000000, 5.687697999151106851E-16, -6.771501495036750356E-12 ) ) ;
#8819 = ORIENTED_EDGE ( 'NONE', *, *, #10504, .T. ) ;
#8820 = CARTESIAN_POINT ( 'NONE',  ( -24.87138426050000106, -13.91768300640000078, 226.0425107039999943 ) ) ;
#8821 = FILL_AREA_STYLE_COLOUR ( '', #3044 ) ;
#8822 = CARTESIAN_POINT ( 'NONE',  ( 15.69372571266449512, 10.97998838177520931, -1.972246272986471594 ) ) ;
#8823 = CARTESIAN_POINT ( 'NONE',  ( -3.923124363200321429, -2.439375170321697706, -95.36817406305493705 ) ) ;
#8824 = CARTESIAN_POINT ( 'NONE',  ( 14.79876163761986341, -22.00000000000000000, -29.34531477793196785 ) ) ;
#8825 = CARTESIAN_POINT ( 'NONE',  ( -8.699999999648019511, -15.69115814626919914, -38.04095234954149873 ) ) ;
#8826 = FACE_OUTER_BOUND ( 'NONE', #22254, .T. ) ;
#8827 = ADVANCED_FACE ( 'NONE', ( #4990 ), #28744, .F. ) ;
#8828 = CARTESIAN_POINT ( 'NONE',  ( 4.528382002446963206, -1.659419471228278375, -6.773605321699999848 ) ) ;
#8829 = CARTESIAN_POINT ( 'NONE',  ( 4.266075142677475007, -0.9221078188639888484, -23.79036215650000230 ) ) ;
#8830 = CARTESIAN_POINT ( 'NONE',  ( 11.50000000000000000, 22.40709319595134730, -62.85117013414870257 ) ) ;
#8831 = CARTESIAN_POINT ( 'NONE',  ( -3.933116308366643388, -2.503391685379829923, -95.30338155897700858 ) ) ;
#8832 = CARTESIAN_POINT ( 'NONE',  ( -0.9592076359739227787, 3.499847752373102860, 227.7207037332364052 ) ) ;
#8833 = CARTESIAN_POINT ( 'NONE',  ( -27.79999999990000248, 3.326931647099999889, 222.0000000000000000 ) ) ;
#8834 = CARTESIAN_POINT ( 'NONE',  ( -7.861312627756135818, -5.597492073231208565, -34.74908987276850780 ) ) ;
#8835 = B_SPLINE_CURVE_WITH_KNOTS ( 'NONE', 3,
 ( #20559, #27955, #21036, #23408, #25607, #3560, #8586, #25449, #3882, #6395, #15994 ),
 .UNSPECIFIED., .F., .F.,
 ( 4, 1, 1, 1, 2, 2, 4 ),
 ( 0.000000000000000000, 0.2500000000000179301, 0.3750000000000248690, 0.4375000000000283662, 0.4687500000000269229, 0.5000000000000254241, 1.000000000000000000 ),
 .UNSPECIFIED. ) ;
#8836 = DIRECTION ( 'NONE',  ( -3.924189347185962345E-12, 0.4082287037029531107, 0.9128796883888953273 ) ) ;
#8837 = CARTESIAN_POINT ( 'NONE',  ( 0.9015611980579174567, -28.48625233387464561, 6.042323509000024906 ) ) ;
#8838 = CARTESIAN_POINT ( 'NONE',  ( 10.70000000009999930, -31.44000000000000128, -28.39999999989999679 ) ) ;
#8839 = ORIENTED_EDGE ( 'NONE', *, *, #7583, .F. ) ;
#8840 = CARTESIAN_POINT ( 'NONE',  ( -1.377718196578040954, -5.677888627607300620, -61.14311227092499479 ) ) ;
#8841 = CARTESIAN_POINT ( 'NONE',  ( 20.30405755279999980, 20.00000000000000000, 228.5999999789999890 ) ) ;
#8842 = VERTEX_POINT ( 'NONE', #31117 ) ;
#8843 = ORIENTED_EDGE ( 'NONE', *, *, #27536, .T. ) ;
#8844 = CARTESIAN_POINT ( 'NONE',  ( -6.726015838937419389, -25.94607852067422016, 21.60652066236992752 ) ) ;
#8845 = CARTESIAN_POINT ( 'NONE',  ( 6.487627055914963137, 0.6495842397260740420, -29.63116556699998938 ) ) ;
#8846 = ORIENTED_EDGE ( 'NONE', *, *, #25062, .F. ) ;
#8847 = CARTESIAN_POINT ( 'NONE',  ( -24.73474822280000041, -14.15859640590000090, 226.0959706989999916 ) ) ;
#8848 = ADVANCED_FACE ( 'NONE', ( #26697 ), #14601, .F. ) ;
#8849 = CARTESIAN_POINT ( 'NONE',  ( -2.827549391578647153, -2.736619477458235306, -68.10000000002501963 ) ) ;
#8850 = B_SPLINE_CURVE_WITH_KNOTS ( 'NONE', 5,
 ( #47, #28812, #28203, #6645, #25860, #4298, #23503, #1937, #5519, #19545, #24574, #2702, #21746, #5210, #10255 ),
 .UNSPECIFIED., .F., .F.,
 ( 6, 3, 3, 3, 6 ),
 ( 0.000000000000000000, 0.1000000000028630903, 0.3999999999999999667, 0.7000000000005727196, 1.000000000000000000 ),
 .UNSPECIFIED. ) ;
#8851 = ORIENTED_EDGE ( 'NONE', *, *, #13098, .T. ) ;
#8852 = ORIENTED_EDGE ( 'NONE', *, *, #23068, .F. ) ;
#8853 = ADVANCED_FACE ( 'NONE', ( #24189 ), #13951, .T. ) ;
#8854 = ORIENTED_EDGE ( 'NONE', *, *, #29145, .T. ) ;
#8855 = DIRECTION ( 'NONE',  ( 2.256992747040000044E-12, -0.000000000000000000, -1.000000000000000000 ) ) ;
#8856 = B_SPLINE_CURVE_WITH_KNOTS ( 'NONE', 5,
 ( #26826, #5277, #7479, #26673, #14723, #29335, #7331, #2604, #14884, #7931, #17532, #27141 ),
 .UNSPECIFIED., .F., .F.,
 ( 6, 3, 3, 6 ),
 ( 3.339306056309999882, 4.810258468129999798, 6.613963840190000276, 6.678484286069999776 ),
 .UNSPECIFIED. ) ;
#8857 = ORIENTED_EDGE ( 'NONE', *, *, #8304, .T. ) ;
#8858 = CARTESIAN_POINT ( 'NONE',  ( -8.699999999656894190, -18.16737667679718626, -36.73114375906605744 ) ) ;
#8859 = CARTESIAN_POINT ( 'NONE',  ( 1.057599857924298670, -1.834951416016458614, 226.6412452697800290 ) ) ;
#8860 = CARTESIAN_POINT ( 'NONE',  ( -1.895255389310859684, 5.229048247678121264, -69.15099036452500059 ) ) ;
#8861 = CARTESIAN_POINT ( 'NONE',  ( 27.53132592980000126, -7.212385509899999825, 229.7313259299999686 ) ) ;
#8862 = CARTESIAN_POINT ( 'NONE',  ( -1.100000000000000089, -26.77741585740000119, 225.0000000000000000 ) ) ;
#8863 = CARTESIAN_POINT ( 'NONE',  ( -14.53037274729999950, -23.87930420520000041, 222.0000000000000000 ) ) ;
#8864 = EDGE_CURVE ( 'NONE', #21489, #25001, #3707, .T. ) ;
#8865 = DIRECTION ( 'NONE',  ( -8.077935669463159094E-28, -0.9128796883888953273, 0.4082287037029530552 ) ) ;
#8866 = ORIENTED_EDGE ( 'NONE', *, *, #5539, .T. ) ;
#8867 = CARTESIAN_POINT ( 'NONE',  ( 11.02757639490000052, -24.42656466549999905, -0.8308236885000014338 ) ) ;
#8868 = CARTESIAN_POINT ( 'NONE',  ( -1.499765329346335108, -5.740821375879678001, -11.55022317839999424 ) ) ;
#8869 = CARTESIAN_POINT ( 'NONE',  ( 18.95046173579999760, -18.95046173579999760, 136.7828584120000244 ) ) ;
#8870 = ADVANCED_FACE ( 'NONE', ( #24805 ), #13966, .T. ) ;
#8871 = DIRECTION ( 'NONE',  ( 1.000000000000000000, 0.000000000000000000, 0.000000000000000000 ) ) ;
#8872 = VERTEX_POINT ( 'NONE', #24959 ) ;
#8873 = DIRECTION ( 'NONE',  ( 1.000000000000000000, 3.757855673434259506E-24, -2.257150022441365115E-12 ) ) ;
#8874 = CARTESIAN_POINT ( 'NONE',  ( -10.69999999999999929, -130.0000000000000000, -41.24671599790000442 ) ) ;
#8875 = PRODUCT_DEFINITION ( 'UNKNOWN', '', #17365, #3681 ) ;
#8876 = CARTESIAN_POINT ( 'NONE',  ( 8.700000000301640668, -14.95611408989196711, -40.37595097046296644 ) ) ;
#8877 = CARTESIAN_POINT ( 'NONE',  ( 27.24406355354269849, 0.4957164003158900378, 0.08279779300002232389 ) ) ;
#8878 = CARTESIAN_POINT ( 'NONE',  ( 22.71671780426621723, -14.21943167003267838, 4.451031837088323506 ) ) ;
#8879 = CARTESIAN_POINT ( 'NONE',  ( 5.975646968830259809, -0.1056191442178888718, -58.09793411332499602 ) ) ;
#8880 = CARTESIAN_POINT ( 'NONE',  ( -23.69427943501400691, -14.54081806258934861, 6.079851352000009257 ) ) ;
#8881 = CYLINDRICAL_SURFACE ( 'NONE', #4739, 18.00000000000000000 ) ;
#8882 = VERTEX_POINT ( 'NONE', #8574 ) ;
#8883 = CARTESIAN_POINT ( 'NONE',  ( 24.52721838744982463, -14.51532614974687796, 4.239732040000027347 ) ) ;
#8884 = CARTESIAN_POINT ( 'NONE',  ( 19.80538173169999894, 19.50875421069999760, 226.2000000000000171 ) ) ;
#8885 = B_SPLINE_CURVE_WITH_KNOTS ( 'NONE', 3,
 ( #10894, #20803, #4121, #8672, #3965, #28032, #25529, #18271, #11361, #1771, #20485, #28346, #6477, #27714, #27881, #18592, #13400, #13563, #1459, #8992, #6160, #18112, #25374, #6326, #16078, #28188 ),
 .UNSPECIFIED., .F., .F.,
 ( 4, 2, 2, 2, 2, 2, 2, 2, 2, 2, 2, 2, 4 ),
 ( 0.000000000000000000, 0.001576069497370726673, 0.002364104246056131318, 0.003152138994741535746, 0.004728208492112424832, 0.005516243240797868291, 0.006304277989483312618, 0.007880347486854262853, 0.008668382235539714986, 0.009456416984225165384, 0.01024445173291061752, 0.01103248648159606791, 0.01260855597896695483 ),
 .UNSPECIFIED. ) ;
#8886 = CARTESIAN_POINT ( 'NONE',  ( 2.446868394388314272, -3.520846267504715854, -68.10000000002500542 ) ) ;
#8887 = EDGE_CURVE ( 'NONE', #31042, #17004, #15508, .T. ) ;
#8888 = PRODUCT_DEFINITION_SHAPE ( 'NONE', 'NONE',  #22352 ) ;
#8889 =( GEOMETRIC_REPRESENTATION_CONTEXT ( 3 ) GLOBAL_UNCERTAINTY_ASSIGNED_CONTEXT ( ( #15067 ) ) GLOBAL_UNIT_ASSIGNED_CONTEXT ( ( #19091, #7438, #7739 ) ) REPRESENTATION_CONTEXT ( 'NONE', 'WORKASPACE' ) );
#8890 = DIRECTION ( 'NONE',  ( 0.000000000000000000, -2.256505319260000033E-12, -1.000000000000000000 ) ) ;
#8891 = CARTESIAN_POINT ( 'NONE',  ( -4.367877465460095365, 1.136530670978911362, -44.10000000002498410 ) ) ;
#8892 = EDGE_CURVE ( 'NONE', #24657, #25641, #405, .T. ) ;
#8893 = ORIENTED_EDGE ( 'NONE', *, *, #2892, .F. ) ;
#8894 = DIRECTION ( 'NONE',  ( 3.590123367689346428E-13, 0.9128796883888948832, -0.4082287037029536658 ) ) ;
#8895 = COLOUR_RGB ( '', 0.09019608, 0.27058824, 0.51372549) ;
#8896 = CARTESIAN_POINT ( 'NONE',  ( 2.994727039187459194, -3.426347720743798231, -64.89605006312500279 ) ) ;
#8897 = ORIENTED_EDGE ( 'NONE', *, *, #1516, .T. ) ;
#8898 = EDGE_CURVE ( 'NONE', #10599, #9943, #22292, .T. ) ;
#8899 = DIRECTION ( 'NONE',  ( 1.224606353819999829E-16, 1.000000000000000000, 0.000000000000000000 ) ) ;
#8900 = ORIENTED_EDGE ( 'NONE', *, *, #29829, .T. ) ;
#8901 = CARTESIAN_POINT ( 'NONE',  ( -27.66290831536099759, -7.787312998881454895, 0.8585786439999909536 ) ) ;
#8902 = EDGE_LOOP ( 'NONE', ( #10969, #23510, #21139, #28446, #10907 ) ) ;
#8903 = CARTESIAN_POINT ( 'NONE',  ( 19.80526555972147307, 19.50877392102524155, 3.000000000000002665 ) ) ;
#8904 = CARTESIAN_POINT ( 'NONE',  ( -26.80000000000000071, 9.769962616700000205E-15, 186.7828584120000244 ) ) ;
#8905 = CARTESIAN_POINT ( 'NONE',  ( 8.000000000264140709, -18.27877680372071723, -30.94409471150577318 ) ) ;
#8906 = CARTESIAN_POINT ( 'NONE',  ( -15.94126856105729573, 10.34054669365686152, -0.6999999999999783062 ) ) ;
#8907 = B_SPLINE_SURFACE_WITH_KNOTS ( 'NONE', 5, 1, ( 
 ( #4529, #4214 ),
 ( #4063, #2173 ),
 ( #18681, #30660 ),
 ( #11764, #13817 ),
 ( #6875, #16328 ),
 ( #26092, #1703 ),
 ( #18531, #21368 ),
 ( #30964, #11304 ),
 ( #21207, #28282 ),
 ( #28133, #28602 ),
 ( #20905, #6571 ),
 ( #6723, #11610 ),
 ( #4370, #28443 ),
 ( #9394, #18997 ),
 ( #7042, #16632 ) ),
 .UNSPECIFIED., .F., .F., .F.,
 ( 6, 3, 3, 3, 6 ),
 ( 2, 2 ),
 ( 0.000000000000000000, 0.5239055192729999977, 1.047811038550000129, 1.571716557820000082, 1.746351730910000066 ),
 ( -0.7000000000009999335, 2.557302930970000000E-06 ),
 .UNSPECIFIED. ) ;
#8908 = CARTESIAN_POINT ( 'NONE',  ( -0.6094664100040195764, -28.49364619262437870, 4.895947184000021046 ) ) ;
#8909 = DIRECTION ( 'NONE',  ( 5.962915006522623408E-16, 0.4383711467890811231, 0.8987940462991652613 ) ) ;
#8910 = PLANE ( 'NONE',  #10509 ) ;
#8911 = VERTEX_POINT ( 'NONE', #17701 ) ;
#8912 = PLANE ( 'NONE',  #8965 ) ;
#8913 = CARTESIAN_POINT ( 'NONE',  ( 10.82908725742652933, -27.76276047461856322, 36.78285841159999592 ) ) ;
#8914 = CARTESIAN_POINT ( 'NONE',  ( 19.76610007289999871, 19.51851078889999869, 229.2246588520000046 ) ) ;
#8915 = VECTOR ( 'NONE', #19008, 1000.000000000000000 ) ;
#8916 = CARTESIAN_POINT ( 'NONE',  ( -2.212956828297914846, 3.167046338434466257, 230.6345832158275186 ) ) ;
#8917 = CARTESIAN_POINT ( 'NONE',  ( 9.738910687886868089, -24.96785170200598358, 115.0000000000000000 ) ) ;
#8918 = CARTESIAN_POINT ( 'NONE',  ( 8.136960026420000602, 8.894733314490000708, 230.6412452697800006 ) ) ;
#8919 = VECTOR ( 'NONE', #2877, 1000.000000000000000 ) ;
#8920 = B_SPLINE_CURVE_WITH_KNOTS ( 'NONE', 3,
 ( #15896, #25499, #23144, #28472, #1891, #23294 ),
 .UNSPECIFIED., .F., .F.,
 ( 4, 2, 4 ),
 ( 0.000000000000000000, 0.5000000000000000000, 1.000000000000000000 ),
 .UNSPECIFIED. ) ;
#8921 = CARTESIAN_POINT ( 'NONE',  ( 23.74378135472953488, 14.46011237893922008, 3.899998580999998854 ) ) ;
#8922 = CYLINDRICAL_SURFACE ( 'NONE', #26183, 10.00000000000000178 ) ;
#8923 = CARTESIAN_POINT ( 'NONE',  ( 4.762123832160154890, 2.112064333128992555, -51.12998794302500016 ) ) ;
#8924 = CARTESIAN_POINT ( 'NONE',  ( 14.76418395427317343, -23.44536579588614700, -24.67876632261722136 ) ) ;
#8925 = CARTESIAN_POINT ( 'NONE',  ( 14.76504187223401487, -28.44906468419981138, -33.33684912348113727 ) ) ;
#8926 = DIRECTION ( 'NONE',  ( -1.000000000000000000, 0.000000000000000000, 0.000000000000000000 ) ) ;
#8927 = EDGE_CURVE ( 'NONE', #23122, #20043, #10867, .T. ) ;
#8928 = PLANE ( 'NONE',  #20798 ) ;
#8929 = ORIENTED_EDGE ( 'NONE', *, *, #25405, .T. ) ;
#8930 = ADVANCED_FACE ( 'NONE', ( #22450 ), #5906, .F. ) ;
#8931 = DIRECTION ( 'NONE',  ( 0.000000000000000000, 1.000000000000000000, 0.000000000000000000 ) ) ;
#8932 = VECTOR ( 'NONE', #16872, 1000.000000000000000 ) ;
#8933 = EDGE_CURVE ( 'NONE', #21911, #26831, #3720, .T. ) ;
#8934 = ORIENTED_EDGE ( 'NONE', *, *, #27309, .F. ) ;
#8935 = CARTESIAN_POINT ( 'NONE',  ( 6.136659917674307074, 0.6935318534554493208, -55.49771407622499453 ) ) ;
#8936 = VERTEX_POINT ( 'NONE', #22752 ) ;
#8937 = TOROIDAL_SURFACE ( 'NONE', #21503, 5.792819795519999815, 2.000000000000000000 ) ;
#8938 = SHAPE_DEFINITION_REPRESENTATION ( #30171, #30659 ) ;
#8939 = ORIENTED_EDGE ( 'NONE', *, *, #16011, .T. ) ;
#8940 = CARTESIAN_POINT ( 'NONE',  ( -17.49285076559436902, -29.59593888003697870, -32.67472628167575266 ) ) ;
#8941 = ORIENTED_EDGE ( 'NONE', *, *, #6964, .F. ) ;
#8942 = DIRECTION ( 'NONE',  ( 0.000000000000000000, -1.000000000000000000, 0.000000000000000000 ) ) ;
#8943 = CARTESIAN_POINT ( 'NONE',  ( -9.993285220779425160, -25.61999708228226069, 36.39444872359999295 ) ) ;
#8944 = CARTESIAN_POINT ( 'NONE',  ( -17.39988487663317329, -30.61060157591113651, -24.71107910008982245 ) ) ;
#8945 = CARTESIAN_POINT ( 'NONE',  ( -6.704241792037686665, 4.607281334802888928, -43.06409624422267513 ) ) ;
#8946 = CARTESIAN_POINT ( 'NONE',  ( 3.466821295769682159E-14, -2.890242878314739659E-13, 277.5163816122566800 ) ) ;
#8947 = CARTESIAN_POINT ( 'NONE',  ( -7.105427357599999217E-15, 7.105427357599999217E-15, 86.39444872449999480 ) ) ;
#8948 = CARTESIAN_POINT ( 'NONE',  ( 5.003468744149685676, 2.348385630676867564, -1.479170051700001487 ) ) ;
#8949 = CARTESIAN_POINT ( 'NONE',  ( 26.05511440539999768, -14.93230011240000010, 229.2404163060000144 ) ) ;
#8950 = ORIENTED_EDGE ( 'NONE', *, *, #29279, .F. ) ;
#8951 = DIRECTION ( 'NONE',  ( 0.000000000000000000, 0.3420201433259318358, -0.9396926207858125046 ) ) ;
#8952 = CONICAL_SURFACE ( 'NONE', #23028, 1.656072167390155281, 0.3728633601815770082 ) ;
#8953 = CARTESIAN_POINT ( 'NONE',  ( -2.766209873889304394, 4.939907206908331183, -17.67761783620000671 ) ) ;
#8954 = CARTESIAN_POINT ( 'NONE',  ( 5.317483451773077796, 6.418870144806576583, -40.60986132251716185 ) ) ;
#8955 = SHAPE_REPRESENTATION ( 'Washer', ( #17722 ), #22285 ) ;
#8956 = EDGE_CURVE ( 'NONE', #22879, #10748, #28138, .T. ) ;
#8957 = CARTESIAN_POINT ( 'NONE',  ( 8.000000000856587690, -26.13380090421571111, -25.50104989771282149 ) ) ;
#8958 = CARTESIAN_POINT ( 'NONE',  ( -1.419173379619999950E-06, -27.80022181310000207, 223.9000014189999774 ) ) ;
#8959 = CARTESIAN_POINT ( 'NONE',  ( -3.397257074621320871, -28.55879647729619109, 8.000000000000007105 ) ) ;
#8960 = DIRECTION ( 'NONE',  ( -0.9316362575375349842, 0.3633921898465292122, -0.000000000000000000 ) ) ;
#8961 = EDGE_CURVE ( 'NONE', #20043, #30907, #22607, .T. ) ;
#8962 = CARTESIAN_POINT ( 'NONE',  ( 0.5184513693225726305, -28.49550581263314086, 6.099998581000020792 ) ) ;
#8963 = CARTESIAN_POINT ( 'NONE',  ( 3.458129700889219116, -0.5397582531354582214, 226.6412452697749984 ) ) ;
#8964 = CARTESIAN_POINT ( 'NONE',  ( 0.03549436698350039859, -27.80040766163043031, 3.997479608999987555 ) ) ;
#8965 = AXIS2_PLACEMENT_3D ( 'NONE', #28116, #13798, #23414 ) ;
#8966 = DIRECTION ( 'NONE',  ( -1.000000000000000000, 0.000000000000000000, 0.000000000000000000 ) ) ;
#8967 = VERTEX_POINT ( 'NONE', #10952 ) ;
#8968 = LINE ( 'NONE', #30059, #15835 ) ;
#8969 = DIRECTION ( 'NONE',  ( -9.228728892150466515E-13, -0.9128796883888956604, 0.4082287037029523336 ) ) ;
#8970 = CARTESIAN_POINT ( 'NONE',  ( 1.191496624263074233, -5.005312061620236008, -0.6999976953858815243 ) ) ;
#8971 = VERTEX_POINT ( 'NONE', #15202 ) ;
#8972 = DIRECTION ( 'NONE',  ( 0.9316362575375356503, 0.3633921898465274913, 0.000000000000000000 ) ) ;
#8973 = ORIENTED_EDGE ( 'NONE', *, *, #26458, .T. ) ;
#8974 = ORIENTED_EDGE ( 'NONE', *, *, #21946, .T. ) ;
#8975 = AXIS2_PLACEMENT_3D ( 'NONE', #6547, #23407, #30317 ) ;
#8976 = VERTEX_POINT ( 'NONE', #10491 ) ;
#8977 = CARTESIAN_POINT ( 'NONE',  ( 18.94276922629999760, 21.23709851079999922, 229.4982322489999831 ) ) ;
#8978 = ORIENTED_EDGE ( 'NONE', *, *, #30602, .F. ) ;
#8979 = CARTESIAN_POINT ( 'NONE',  ( -24.46845037339999962, -13.19716075180000026, 225.7602695470000072 ) ) ;
#8980 = CARTESIAN_POINT ( 'NONE',  ( 24.38199545065365115, 14.75707034588002564, 3.901343066999990228 ) ) ;
#8981 = CARTESIAN_POINT ( 'NONE',  ( -16.83342759582943060, -8.999999999996580513, -0.6999999999999784173 ) ) ;
#8982 = CARTESIAN_POINT ( 'NONE',  ( -16.06988921231594603, 11.79183908526949054, -0.6999999999999784173 ) ) ;
#8983 = CARTESIAN_POINT ( 'NONE',  ( -0.3440332070342348447, -5.174969878487565289, -93.21726054315809051 ) ) ;
#8984 = VECTOR ( 'NONE', #15530, 1000.000000000000000 ) ;
#8985 = CARTESIAN_POINT ( 'NONE',  ( 14.83544356365203498, -22.00000000000000355, -28.95333575274569426 ) ) ;
#8986 = CARTESIAN_POINT ( 'NONE',  ( 23.35305511532094869, -13.14889042229386895, 6.071490516007937543 ) ) ;
#8987 = CARTESIAN_POINT ( 'NONE',  ( -19.68707896189999929, 19.53815547089999782, 229.3695869349999725 ) ) ;
#8988 = EDGE_CURVE ( 'NONE', #13739, #5647, #27742, .T. ) ;
#8989 = ORIENTED_EDGE ( 'NONE', *, *, #21563, .T. ) ;
#8990 = CARTESIAN_POINT ( 'NONE',  ( -3.673964118181757943, -4.849481262180703744, -4.328945369300001289 ) ) ;
#8991 = CARTESIAN_POINT ( 'NONE',  ( 0.2540922009626206957, 4.794324758835501576, -22.00668644580000688 ) ) ;
#8992 = CARTESIAN_POINT ( 'NONE',  ( -4.941595660341803864, -27.05346828916500712, 209.5085898789650116 ) ) ;
#8993 = CARTESIAN_POINT ( 'NONE',  ( -3.666003079838183965, -0.7920474239279197137, -93.44355375713804790 ) ) ;
#8994 = CARTESIAN_POINT ( 'NONE',  ( 0.9176177227138302417, 3.499836378220442690, 227.7144805344090059 ) ) ;
#8995 = CARTESIAN_POINT ( 'NONE',  ( -16.83342759575507586, 10.99999999997565503, -0.6999999999999784173 ) ) ;
#8996 = CARTESIAN_POINT ( 'NONE',  ( -24.09883371379999772, -15.21565466309999870, 225.0000014190000002 ) ) ;
#8997 = EDGE_CURVE ( 'NONE', #17381, #17245, #22001, .T. ) ;
#8998 = CARTESIAN_POINT ( 'NONE',  ( 25.22625794089999829, -13.26224522399999906, 225.0000014190000002 ) ) ;
#8999 = FACE_OUTER_BOUND ( 'NONE', #28176, .T. ) ;
#9000 = CARTESIAN_POINT ( 'NONE',  ( 0.6731456005949999488, -4.118494162357343669, -70.37733883405731206 ) ) ;
#9001 = VERTEX_POINT ( 'NONE', #23229 ) ;
#9002 = CARTESIAN_POINT ( 'NONE',  ( -5.623491485972666126, 3.092612689740418919, -59.33908057272499548 ) ) ;
#9003 = LINE ( 'NONE', #30254, #28367 ) ;
#9004 = ORIENTED_EDGE ( 'NONE', *, *, #18821, .F. ) ;
#9005 = CARTESIAN_POINT ( 'NONE',  ( 8.700000000278096834, -14.92844969908683517, -33.25053330388887218 ) ) ;
#9006 = CARTESIAN_POINT ( 'NONE',  ( 5.245096043587340162, -0.2338077457563897399, -35.69999999999999574 ) ) ;
#9007 = AXIS2_PLACEMENT_3D ( 'NONE', #3844, #29651, #30118 ) ;
#9008 = EDGE_LOOP ( 'NONE', ( #577, #18886, #10497, #15515 ) ) ;
#9009 = CARTESIAN_POINT ( 'NONE',  ( -24.18586237362070435, 13.70852494847550673, 3.927704946426889610 ) ) ;
#9010 = PLANE ( 'NONE',  #13789 ) ;
#9011 = VECTOR ( 'NONE', #17036, 1000.000000000000000 ) ;
#9012 = ORIENTED_EDGE ( 'NONE', *, *, #25988, .F. ) ;
#9013 = ORIENTED_EDGE ( 'NONE', *, *, #12551, .F. ) ;
#9014 = ORIENTED_EDGE ( 'NONE', *, *, #4, .T. ) ;
#9015 =( NAMED_UNIT ( * ) PLANE_ANGLE_UNIT ( ) SI_UNIT ( $, .RADIAN. ) );
#9016 = VERTEX_POINT ( 'NONE', #9200 ) ;
#9017 = CARTESIAN_POINT ( 'NONE',  ( 24.37165445055180157, -14.77472140295711434, 5.104215870000011535 ) ) ;
#9018 = EDGE_CURVE ( 'NONE', #12383, #23813, #30772, .T. ) ;
#9019 = CARTESIAN_POINT ( 'NONE',  ( 6.000000000000000000, -15.86465192213301556, -74.65259062561435144 ) ) ;
#9020 = CARTESIAN_POINT ( 'NONE',  ( -1.595193757947241497, 6.212219048941578059, -65.72876360962500542 ) ) ;
#9021 = CARTESIAN_POINT ( 'NONE',  ( 27.79999999980000069, -7.282770092329999834, 229.0000000000000000 ) ) ;
#9022 = B_SPLINE_CURVE_WITH_KNOTS ( 'NONE', 5,
 ( #21385, #16958, #19172, #26712, #14761, #19013 ),
 .UNSPECIFIED., .F., .F.,
 ( 6, 6 ),
 ( -2.300779731039999998, 0.000000000000000000 ),
 .UNSPECIFIED. ) ;
#9023 = CYLINDRICAL_SURFACE ( 'NONE', #29226, 3.000000000000002220 ) ;
#9024 = CARTESIAN_POINT ( 'NONE',  ( 8.000000000735605354, -29.98791861930862268, -27.92402217156406152 ) ) ;
#9025 = PLANE ( 'NONE',  #3515 ) ;
#9026 = VERTEX_POINT ( 'NONE', #14098 ) ;
#9027 = CARTESIAN_POINT ( 'NONE',  ( 10.79767714369999965, -24.52928866599999935, -0.9448357716000042039 ) ) ;
#9028 = CIRCLE ( 'NONE', #27618, 2.000000000000002220 ) ;
#9029 = CARTESIAN_POINT ( 'NONE',  ( 2.618538529469167653, 3.470429992801025154, -13.72796858840000489 ) ) ;
#9030 = FACE_OUTER_BOUND ( 'NONE', #23593, .T. ) ;
#9031 = CARTESIAN_POINT ( 'NONE',  ( 24.68173674080000168, -14.25001227039999918, 223.9000014189999774 ) ) ;
#9032 = ORIENTED_EDGE ( 'NONE', *, *, #24083, .T. ) ;
#9033 = CARTESIAN_POINT ( 'NONE',  ( -23.35870914495593809, -15.07359600611589912, 4.322692715549829146 ) ) ;
#9034 = DIRECTION ( 'NONE',  ( 1.000000000000000000, 0.000000000000000000, 0.000000000000000000 ) ) ;
#9035 = CARTESIAN_POINT ( 'NONE',  ( -23.72449085899999943, 15.79286685369999788, 222.0000000000000000 ) ) ;
#9036 = EDGE_CURVE ( 'NONE', #2487, #6694, #11589, .T. ) ;
#9037 = LINE ( 'NONE', #18634, #7130 ) ;
#9038 = DIRECTION ( 'NONE',  ( 0.000000000000000000, 0.000000000000000000, -1.000000000000000000 ) ) ;
#9039 = B_SPLINE_CURVE_WITH_KNOTS ( 'NONE', 5,
 ( #20190, #5862, #29317, #17660, #8066, #15469, #5710, #3504, #29164 ),
 .UNSPECIFIED., .F., .F.,
 ( 6, 3, 6 ),
 ( 0.000000000000000000, 54.03331039209999886, 92.56095350929999199 ),
 .UNSPECIFIED. ) ;
#9040 = CARTESIAN_POINT ( 'NONE',  ( 0.9406167415608388538, 5.909121140422558760, -54.41500058692499664 ) ) ;
#9041 = CARTESIAN_POINT ( 'NONE',  ( -27.50000000000000000, 3.367667473009999970E-15, 230.0000000000000000 ) ) ;
#9042 = DIRECTION ( 'NONE',  ( 0.7071067811780483714, -0.6644630243965946592, -0.2418447626510653037 ) ) ;
#9043 = VERTEX_POINT ( 'NONE', #30933 ) ;
#9044 = CARTESIAN_POINT ( 'NONE',  ( 19.80538173169999894, 19.50875421069999760, 229.0000000000000000 ) ) ;
#9045 = CARTESIAN_POINT ( 'NONE',  ( 2.841892371157072716, -3.648336829434535300, -68.10000000002500542 ) ) ;
#9046 = EDGE_CURVE ( 'NONE', #28677, #29912, #2614, .T. ) ;
#9047 = STYLED_ITEM ( 'NONE', ( #1023 ), #941 ) ;
#9048 = EDGE_CURVE ( 'NONE', #17900, #11176, #11421, .T. ) ;
#9049 = DIRECTION ( 'NONE',  ( -5.551115123049999208E-18, 0.000000000000000000, -1.000000000000000000 ) ) ;
#9050 = CARTESIAN_POINT ( 'NONE',  ( -4.205204442357076466, 0.5518332366461318195, -44.10000000002499121 ) ) ;
#9051 = SURFACE_STYLE_USAGE ( .BOTH. , #25748 ) ;
#9052 = ORIENTED_EDGE ( 'NONE', *, *, #7700, .T. ) ;
#9053 = FACE_BOUND ( 'NONE', #10376, .T. ) ;
#9054 = CARTESIAN_POINT ( 'NONE',  ( -5.973670867977711296, -0.3179945487246996216, -66.04421022022501120 ) ) ;
#9055 = ORIENTED_EDGE ( 'NONE', *, *, #2018, .T. ) ;
#9056 = CARTESIAN_POINT ( 'NONE',  ( -24.49554752220392118, 11.47491990610730106, 0.000000000000000000 ) ) ;
#9057 = ADVANCED_FACE ( 'NONE', ( #9053, #1989, #21024 ), #26057, .T. ) ;
#9058 = CARTESIAN_POINT ( 'NONE',  ( -26.79556473285982321, -0.4875557887251112388, 0.000000000000000000 ) ) ;
#9059 = ORIENTED_EDGE ( 'NONE', *, *, #17231, .F. ) ;
#9060 = DIRECTION ( 'NONE',  ( -1.000000000000000000, 0.000000000000000000, 0.000000000000000000 ) ) ;
#9061 = CARTESIAN_POINT ( 'NONE',  ( -26.84464185210000053, 3.287411897809999814E-15, 187.4375040470000044 ) ) ;
#9062 = FACE_OUTER_BOUND ( 'NONE', #21284, .T. ) ;
#9063 = CARTESIAN_POINT ( 'NONE',  ( -1.074123786107241241, 3.361570641823106165, 0.000000000000000000 ) ) ;
#9064 = DIRECTION ( 'NONE',  ( 1.000000000000000000, 0.000000000000000000, 0.000000000000000000 ) ) ;
#9065 = EDGE_CURVE ( 'NONE', #17448, #12078, #2235, .T. ) ;
#9066 = CARTESIAN_POINT ( 'NONE',  ( -7.482563026693744845, 3.808884430402179166, -42.67469205533632959 ) ) ;
#9067 = DIRECTION ( 'NONE',  ( 0.000000000000000000, 2.255973186040000320E-12, 1.000000000000000000 ) ) ;
#9068 = ORIENTED_EDGE ( 'NONE', *, *, #15047, .F. ) ;
#9069 = DIRECTION ( 'NONE',  ( 0.000000000000000000, 0.000000000000000000, 1.000000000000000000 ) ) ;
#9070 = CARTESIAN_POINT ( 'NONE',  ( -10.69999999999999929, 19.99999999999999645, -42.39999999999999858 ) ) ;
#9071 = CARTESIAN_POINT ( 'NONE',  ( 19.99469103059999853, 20.00000688379999758, 229.8491879540000014 ) ) ;
#9072 = B_SPLINE_CURVE_WITH_KNOTS ( 'NONE', 3,
 ( #17300, #7247, #23, #16679, #21890, #10230, #5346, #7397, #26289, #175 ),
 .UNSPECIFIED., .F., .F.,
 ( 4, 2, 2, 2, 4 ),
 ( 0.000000000000000000, 0.2500000000000000000, 0.5000000000000000000, 0.7500000000000000000, 1.000000000000000000 ),
 .UNSPECIFIED. ) ;
#9073 = CARTESIAN_POINT ( 'NONE',  ( -4.130757957910000097E-10, -1.288485762530000039E-09, 230.0000000000000000 ) ) ;
#9074 = CARTESIAN_POINT ( 'NONE',  ( -1.484924240490000047, -1.484924240490000047, 227.6412452697800006 ) ) ;
#9075 = CARTESIAN_POINT ( 'NONE',  ( -1.064429458170000231, -12.07977735470000091, 230.6412452697800006 ) ) ;
#9076 = CYLINDRICAL_SURFACE ( 'NONE', #29343, 1.100000000000002309 ) ;
#9077 = DIRECTION ( 'NONE',  ( 1.000000000000000000, 0.000000000000000000, 0.000000000000000000 ) ) ;
#9078 = CARTESIAN_POINT ( 'NONE',  ( 4.101176313917077820, -1.931410228222282921, -52.29872167392500160 ) ) ;
#9079 = EDGE_CURVE ( 'NONE', #16428, #21606, #16597, .T. ) ;
#9080 = CIRCLE ( 'NONE', #23176, 3.176829269159998859 ) ;
#9081 = CARTESIAN_POINT ( 'NONE',  ( 9.130136616458420562, 20.99999999999704059, -52.40873942179641887 ) ) ;
#9082 = CARTESIAN_POINT ( 'NONE',  ( 6.906785458558747592, 5.540328039990938258, -40.18136770757133291 ) ) ;
#9083 = CARTESIAN_POINT ( 'NONE',  ( 2.523699655483016446, -2.628482120109524089, 230.7531903453053133 ) ) ;
#9084 = CARTESIAN_POINT ( 'NONE',  ( -24.34663841808528062, -12.78636765232545969, 224.9035402871930387 ) ) ;
#9085 = CARTESIAN_POINT ( 'NONE',  ( 5.132309988016721114, -0.8582124304006011339, -36.74517599850001659 ) ) ;
#9086 = ORIENTED_EDGE ( 'NONE', *, *, #20348, .F. ) ;
#9087 = CARTESIAN_POINT ( 'NONE',  ( 3.615638736159595634, -2.931608942543439067, -56.15923804942499231 ) ) ;
#9088 = ORIENTED_EDGE ( 'NONE', *, *, #1567, .T. ) ;
#9089 = ORIENTED_EDGE ( 'NONE', *, *, #15359, .F. ) ;
#9090 = DIRECTION ( 'NONE',  ( -9.982533390641031007E-25, -1.000000000000000000, 2.257145581550764975E-12 ) ) ;
#9091 = ORIENTED_EDGE ( 'NONE', *, *, #12521, .T. ) ;
#9092 = CARTESIAN_POINT ( 'NONE',  ( 14.71164558017502699, -28.14786721053526009, -23.28957834311704289 ) ) ;
#9093 = CARTESIAN_POINT ( 'NONE',  ( 19.80526555962148549, 19.50877392102342256, 1.000000000000000888 ) ) ;
#9094 = CYLINDRICAL_SURFACE ( 'NONE', #1893, 3.000000000000003109 ) ;
#9095 =( GEOMETRIC_REPRESENTATION_CONTEXT ( 3 ) GLOBAL_UNCERTAINTY_ASSIGNED_CONTEXT ( ( #872 ) ) GLOBAL_UNIT_ASSIGNED_CONTEXT ( ( #5198, #23958, #21904 ) ) REPRESENTATION_CONTEXT ( 'NONE', 'WORKASPACE' ) );
#9096 = CARTESIAN_POINT ( 'NONE',  ( -4.861312627696712241, 5.146895567854025799, -43.32728369093569398 ) ) ;
#9097 = DIRECTION ( 'NONE',  ( 0.000000000000000000, 0.9396926207858125046, 0.3420201433259318358 ) ) ;
#9098 = EDGE_CURVE ( 'NONE', #3279, #4043, #11111, .T. ) ;
#9099 = CARTESIAN_POINT ( 'NONE',  ( 8.700000000245887932, -28.22468611110281245, -31.13863906511161517 ) ) ;
#9100 = CARTESIAN_POINT ( 'NONE',  ( -1.814319851916122772, 5.833166587536846137, -4.774955258300003891 ) ) ;
#9101 = CARTESIAN_POINT ( 'NONE',  ( -23.69119896560000171, -20.94188573509999785, 229.0000000000000000 ) ) ;
#9102 = EDGE_LOOP ( 'NONE', ( #3503, #25090, #7993, #11188 ) ) ;
#9103 = CARTESIAN_POINT ( 'NONE',  ( 22.97596755210000197, 15.65128466780000061, 222.0000000000000000 ) ) ;
#9104 = EDGE_CURVE ( 'NONE', #15917, #23236, #21507, .T. ) ;
#9105 = CARTESIAN_POINT ( 'NONE',  ( 2.326244606069574505, 3.379075471592551949, -17.21259163650000446 ) ) ;
#9106 = CARTESIAN_POINT ( 'NONE',  ( 6.666786106329811723, 5.756039377145860669, -40.28657715642490444 ) ) ;
#9107 = EDGE_CURVE ( 'NONE', #8060, #22535, #1107, .T. ) ;
#9108 = FACE_OUTER_BOUND ( 'NONE', #7997, .T. ) ;
#9109 = CARTESIAN_POINT ( 'NONE',  ( -24.12724309970000292, -13.81083407110000039, 223.9040321390000088 ) ) ;
#9110 = CARTESIAN_POINT ( 'NONE',  ( 27.62819777866805637, -4.248501485358312735, 8.000000000000007105 ) ) ;
#9111 = CARTESIAN_POINT ( 'NONE',  ( -4.041451884379999804, 9.156941871420000667E-11, 227.9588918784999976 ) ) ;
#9112 = B_SPLINE_CURVE_WITH_KNOTS ( 'NONE', 3,
 ( #8087, #15808, #27294, #25419, #13123, #15491, #22895, #25252, #15179, #22731, #3368 ),
 .UNSPECIFIED., .F., .F.,
 ( 4, 1, 1, 1, 2, 2, 4 ),
 ( 0.000000000000000000, 0.2500000000000045519, 0.3750000000000033862, 0.4374999999999993894, 0.4687499999999993339, 0.4999999999999992228, 1.000000000000000000 ),
 .UNSPECIFIED. ) ;
#9113 = CARTESIAN_POINT ( 'NONE',  ( 7.132997404352039439, -5.572998883428931904, -27.02754848604616456 ) ) ;
#9114 = CARTESIAN_POINT ( 'NONE',  ( 49.56288048729999218, -32.92067553680000458, 44.14124526979999530 ) ) ;
#9115 = CARTESIAN_POINT ( 'NONE',  ( -17.62526668104891314, 11.76353838341477953, 0.000000000000000000 ) ) ;
#9116 = DIRECTION ( 'NONE',  ( 0.000000000000000000, 0.3420201433259318358, -0.9396926207858125046 ) ) ;
#9117 = ORIENTED_EDGE ( 'NONE', *, *, #7167, .T. ) ;
#9118 = CARTESIAN_POINT ( 'NONE',  ( 4.000000000000000000, -31.83942647549183746, -80.46693306215520636 ) ) ;
#9119 = CARTESIAN_POINT ( 'NONE',  ( -24.30742244220000003, -13.49161940279999961, 223.9971936000000028 ) ) ;
#9120 = CARTESIAN_POINT ( 'NONE',  ( 0.9003580991302461145, -26.78512134311359105, 4.366512425711518652 ) ) ;
#9121 = VERTEX_POINT ( 'NONE', #28866 ) ;
#9122 = DIRECTION ( 'NONE',  ( 0.000000000000000000, 0.000000000000000000, 1.000000000000000000 ) ) ;
#9123 = EDGE_LOOP ( 'NONE', ( #21845, #28690, #5857, #28016 ) ) ;
#9124 = ORIENTED_EDGE ( 'NONE', *, *, #11822, .F. ) ;
#9125 =( NAMED_UNIT ( * ) PLANE_ANGLE_UNIT ( ) SI_UNIT ( $, .RADIAN. ) );
#9126 = ORIENTED_EDGE ( 'NONE', *, *, #6809, .T. ) ;
#9127 = CARTESIAN_POINT ( 'NONE',  ( -11.69999999989999928, -2.500000000000002220, -2.399999999999999467 ) ) ;
#9128 = VERTEX_POINT ( 'NONE', #29326 ) ;
#9129 = CARTESIAN_POINT ( 'NONE',  ( 5.689665389580000010, 17.26167590659999718, 230.6999999999999886 ) ) ;
#9130 =( NAMED_UNIT ( * ) SI_UNIT ( $, .STERADIAN. ) SOLID_ANGLE_UNIT ( ) );
#9131 = DIRECTION ( 'NONE',  ( 0.6941258031311203780, 0.7198537139083029945, 0.000000000000000000 ) ) ;
#9132 = CARTESIAN_POINT ( 'NONE',  ( 2.004564144564168870, 3.412403539796502461, -35.69999999999999574 ) ) ;
#9133 = LINE ( 'NONE', #21424, #28657 ) ;
#9134 = CARTESIAN_POINT ( 'NONE',  ( 14.67576675165364719, -22.00000000000000000, -30.22138740828507508 ) ) ;
#9135 = CARTESIAN_POINT ( 'NONE',  ( 3.668680263715867973, -0.6456593865231384788, 227.7673180537741473 ) ) ;
#9136 = CARTESIAN_POINT ( 'NONE',  ( -19.79257232079999795, 19.51192870039999860, 229.1494017060000203 ) ) ;
#9137 = ORIENTED_EDGE ( 'NONE', *, *, #27518, .F. ) ;
#9138 = AXIS2_PLACEMENT_3D ( 'NONE', #18197, #15683, #25294 ) ;
#9139 = CARTESIAN_POINT ( 'NONE',  ( -3.052679639724400928, 3.117809041995142749, -4.568732180599999637 ) ) ;
#9140 = CARTESIAN_POINT ( 'NONE',  ( -3.834000099192785616, 2.652495916366752304, -24.96779765530000361 ) ) ;
#9141 = FACE_OUTER_BOUND ( 'NONE', #1055, .T. ) ;
#9142 = PRODUCT ( 'Handle Housing', 'Handle Housing', '', ( #25514 ) ) ;
#9143 = ADVANCED_FACE ( 'NONE', ( #21794 ), #23855, .T. ) ;
#9144 = CARTESIAN_POINT ( 'NONE',  ( -23.67414648238567665, -12.56096907814344732, 224.4424652941504235 ) ) ;
#9145 = CARTESIAN_POINT ( 'NONE',  ( 2.910560681360000016E-11, 19.99999999999999645, -45.10000000000000142 ) ) ;
#9146 = DIRECTION ( 'NONE',  ( 1.000000000000000000, 0.000000000000000000, 0.000000000000000000 ) ) ;
#9147 = FACE_OUTER_BOUND ( 'NONE', #20506, .T. ) ;
#9148 = CARTESIAN_POINT ( 'NONE',  ( 24.18731408344101297, -13.70592755508744531, 6.073251382590931335 ) ) ;
#9149 = CARTESIAN_POINT ( 'NONE',  ( 1.605176535610508326, -27.75389821387976852, 5.104056378000016103 ) ) ;
#9150 = LINE ( 'NONE', #21127, #19340 ) ;
#9151 = ORIENTED_EDGE ( 'NONE', *, *, #30591, .F. ) ;
#9152 = CARTESIAN_POINT ( 'NONE',  ( -3.855177830964256813, -4.571422008809257420, -59.17407541852499975 ) ) ;
#9153 = CARTESIAN_POINT ( 'NONE',  ( -27.24857305720000156, 4.594528870269999565, 229.9172022069999741 ) ) ;
#9154 = EDGE_LOOP ( 'NONE', ( #30693, #8218, #20397, #7876 ) ) ;
#9155 = FACE_OUTER_BOUND ( 'NONE', #13715, .T. ) ;
#9156 = CARTESIAN_POINT ( 'NONE',  ( 6.096654317653251276, 0.1519075334279890166, -20.67661200060000226 ) ) ;
#9157 = ORIENTED_EDGE ( 'NONE', *, *, #3684, .T. ) ;
#9158 = CARTESIAN_POINT ( 'NONE',  ( 25.17364887440000132, -13.36205984479999920, 225.5069763079999916 ) ) ;
#9159 = CARTESIAN_POINT ( 'NONE',  ( 23.55447121679999967, 16.04539731370000055, 222.0000000000000000 ) ) ;
#9161 = ORIENTED_EDGE ( 'NONE', *, *, #29031, .T. ) ;
#9160 = CIRCLE ( 'NONE', #5136, 7.354069295110000404 ) ;
#9162 = ORIENTED_EDGE ( 'NONE', *, *, #24734, .T. ) ;
#9163 = VERTEX_POINT ( 'NONE', #19431 ) ;
#9164 = B_SPLINE_SURFACE_WITH_KNOTS ( 'NONE', 5, 1, ( 
 ( #21313, #25891 ),
 ( #30916, #9343 ),
 ( #18944, #1970 ),
 ( #9035, #13760 ),
 ( #11562, #26191 ),
 ( #6994, #20690 ),
 ( #13924, #18479 ),
 ( #16582, #18633 ),
 ( #4626, #21158 ),
 ( #23060, #6674 ),
 ( #6523, #28396 ),
 ( #11095, #30287 ) ),
 .UNSPECIFIED., .F., .F., .F.,
 ( 6, 3, 3, 6 ),
 ( 2, 2 ),
 ( 71.78637897720000183, 72.28968605440000772, 84.34526466259998756, 88.66823396320000938 ),
 ( -4.314404719430000596E-12, 0.7012472868949999327 ),
 .UNSPECIFIED. ) ;
#9165 = EDGE_LOOP ( 'NONE', ( #4849, #8388 ) ) ;
#9166 = CARTESIAN_POINT ( 'NONE',  ( -8.699999999660043670, -18.28443321518998133, -36.42483785847389299 ) ) ;
#9167 = CARTESIAN_POINT ( 'NONE',  ( 28.03861306157277866, 0.5101735396241771081, -0.2432540810000105580 ) ) ;
#9168 = CARTESIAN_POINT ( 'NONE',  ( 5.384875807261761516, 2.601783486389667832, -66.37315453652500707 ) ) ;
#9169 = EDGE_CURVE ( 'NONE', #24538, #6269, #250, .T. ) ;
#9170 = CARTESIAN_POINT ( 'NONE',  ( 20.44762307379999910, -20.57851214589999955, 229.7313246180000021 ) ) ;
#9171 = B_SPLINE_CURVE_WITH_KNOTS ( 'NONE', 5,
 ( #24866, #15256, #27064, #10084, #28961, #799 ),
 .UNSPECIFIED., .F., .F.,
 ( 6, 6 ),
 ( 0.000000000000000000, 2.300779653749999820 ),
 .UNSPECIFIED. ) ;
#9172 = DIRECTION ( 'NONE',  ( 0.000000000000000000, 0.000000000000000000, -1.000000000000000000 ) ) ;
#9173 = CARTESIAN_POINT ( 'NONE',  ( 28.50002393070000295, -0.8733865600460000156, 222.0000000000000000 ) ) ;
#9174 = CARTESIAN_POINT ( 'NONE',  ( 1.557513348718032375, -4.881019519337725043, -0.7000303665504261641 ) ) ;
#9175 = ORIENTED_EDGE ( 'NONE', *, *, #4629, .T. ) ;
#9176 = CARTESIAN_POINT ( 'NONE',  ( -18.64452468818404540, 19.99990995005524752, -0.6110695939093615525 ) ) ;
#9177 = CARTESIAN_POINT ( 'NONE',  ( -5.527020701484460119, 0.1640065206915941320, -12.18304957889999862 ) ) ;
#9178 = CARTESIAN_POINT ( 'NONE',  ( 18.95046173579999760, -18.95046173579999760, -2.842170943039999687E-14 ) ) ;
#9179 = CARTESIAN_POINT ( 'NONE',  ( -10.69999999967889259, -27.83695679439218651, -31.51688268319167463 ) ) ;
#9180 = CIRCLE ( 'NONE', #16219, 4.000000000000000888 ) ;
#9181 = ORIENTED_EDGE ( 'NONE', *, *, #17382, .T. ) ;
#9182 = DIRECTION ( 'NONE',  ( -1.000000000000000000, 0.000000000000000000, 0.000000000000000000 ) ) ;
#9183 = CARTESIAN_POINT ( 'NONE',  ( 1.592882851206511186, -27.75460863273100998, 4.791883387999989807 ) ) ;
#9184 = FACE_BOUND ( 'NONE', #21498, .T. ) ;
#9185 = CARTESIAN_POINT ( 'NONE',  ( 9.221751571650358414, -25.90851042236079849, 24.42522152380284339 ) ) ;
#9186 = B_SPLINE_CURVE_WITH_KNOTS ( 'NONE', 3,
 ( #20530, #3855, #13444, #6524, #16122, #30756, #12131, #9185, #21160, #190, #351, #7413, #6675, #9780, #11406, #9934, #24105, #7565, #2545, #26612, #16273, #19538, #21905, #19381, #14662, #29121 ),
 .UNSPECIFIED., .F., .F.,
 ( 4, 2, 2, 2, 2, 2, 2, 2, 2, 2, 2, 2, 4 ),
 ( 0.000000000000000000, 0.001576069497370868920, 0.002364104246056298285, 0.003152138994741727866, 0.004728208492112593968, 0.005516243240798030488, 0.006304277989483467008, 0.007880347486854335712, 0.008668382235539772232, 0.009456416984225208752, 0.01024445173291064354, 0.01103248648159608006, 0.01260855597896695136 ),
 .UNSPECIFIED. ) ;
#9187 = PLANE ( 'NONE',  #12962 ) ;
#9188 = CARTESIAN_POINT ( 'NONE',  ( 5.896017893897736784, 2.415859114112482775, -60.89141554682500157 ) ) ;
#9189 = CARTESIAN_POINT ( 'NONE',  ( 1.030019577584204020E-10, -102.7755780389355778, 17.20706796825876239 ) ) ;
#9190 = CARTESIAN_POINT ( 'NONE',  ( 8.000000000248304488, -25.92947504235655032, -31.20249033167290165 ) ) ;
#9191 = ORIENTED_EDGE ( 'NONE', *, *, #668, .T. ) ;
#9192 = DIRECTION ( 'NONE',  ( -1.000000000000000000, 0.000000000000000000, 0.000000000000000000 ) ) ;
#9193 = FACE_OUTER_BOUND ( 'NONE', #7431, .T. ) ;
#9194 = CARTESIAN_POINT ( 'NONE',  ( 2.667210884058451636, -3.897237072852844264, -68.10000000002501963 ) ) ;
#9195 = AXIS2_PLACEMENT_3D ( 'NONE', #27303, #12517, #19921 ) ;
#9196 = ADVANCED_FACE ( 'NONE', ( #7770 ), #4643, .F. ) ;
#9197 = CARTESIAN_POINT ( 'NONE',  ( 19.73189145681168100, 18.31187121618595270, -0.6999999999999784173 ) ) ;
#9198 = CARTESIAN_POINT ( 'NONE',  ( 10.00000000000000000, -13.98526668056139144, -73.96855033896248699 ) ) ;
#9199 = EDGE_LOOP ( 'NONE', ( #15875, #13895, #8402, #21682, #24076, #10186, #26136, #1405, #26354, #20300 ) ) ;
#9200 = CARTESIAN_POINT ( 'NONE',  ( 10.70000000009999930, -22.55999999999999872, -28.39999999989999679 ) ) ;
#9201 = CIRCLE ( 'NONE', #2675, 5.792819795729999832 ) ;
#9202 = CARTESIAN_POINT ( 'NONE',  ( -3.135263495386069632, -4.229858287310033660, -65.88409070562501313 ) ) ;
#9203 = ORIENTED_EDGE ( 'NONE', *, *, #23887, .F. ) ;
#9204 = EDGE_CURVE ( 'NONE', #5609, #15947, #911, .T. ) ;
#9205 = CARTESIAN_POINT ( 'NONE',  ( 24.32472724076343695, -13.45989056521276872, 3.899998581000013509 ) ) ;
#9206 = CARTESIAN_POINT ( 'NONE',  ( -25.14597776469910428, -15.02549348198344603, 1.000000001000006522 ) ) ;
#9207 = ORIENTED_EDGE ( 'NONE', *, *, #6531, .F. ) ;
#9208 = CARTESIAN_POINT ( 'NONE',  ( 27.23548387100000312, -1.776356839399999804E-15, 88.33953982530000815 ) ) ;
#9209 = SURFACE_SIDE_STYLE ('',( #18656 ) ) ;
#9210 = CARTESIAN_POINT ( 'NONE',  ( 9.989498421329999545, 19.99999999999999645, -42.57860042107999732 ) ) ;
#9211 = CARTESIAN_POINT ( 'NONE',  ( -17.39988487662844108, -23.38939842406737313, -32.08892090029773669 ) ) ;
#9212 = DIRECTION ( 'NONE',  ( -1.000000000000000000, 1.380859481889999837E-13, -9.437625531729999712E-14 ) ) ;
#9213 = CARTESIAN_POINT ( 'NONE',  ( 8.700000000240452280, -29.66169484525095612, -29.83890322678064777 ) ) ;
#9214 = ORIENTED_EDGE ( 'NONE', *, *, #19248, .T. ) ;
#9215 = DIRECTION ( 'NONE',  ( -1.000000000000000000, 5.665498452320000818E-16, 0.000000000000000000 ) ) ;
#9216 = EDGE_CURVE ( 'NONE', #19078, #7630, #7459, .T. ) ;
#9217 = CARTESIAN_POINT ( 'NONE',  ( 0.9891023284355177081, -26.78175549087869101, 225.4866061618205606 ) ) ;
#9218 = TOROIDAL_SURFACE ( 'NONE', #13770, 24.50000000000000000, 3.200000000000000178 ) ;
#9219 = VECTOR ( 'NONE', #22205, 1000.000000000000000 ) ;
#9220 = CARTESIAN_POINT ( 'NONE',  ( 14.85000000009999788, -27.00000000000000000, -28.39999999989999679 ) ) ;
#9221 = ADVANCED_FACE ( 'NONE', ( #407 ), #23037, .F. ) ;
#9222 = CARTESIAN_POINT ( 'NONE',  ( -15.89343021241115039, -9.582866096052068627, 0.000000000000000000 ) ) ;
#9223 = CARTESIAN_POINT ( 'NONE',  ( -12.34886039477888175, -30.24848416943050822, -32.29798948241971601 ) ) ;
#9224 = CARTESIAN_POINT ( 'NONE',  ( -0.8958568848300000331, -28.48628573779999940, 225.6801695290000112 ) ) ;
#9225 = FACE_OUTER_BOUND ( 'NONE', #15375, .T. ) ;
#9226 = DIRECTION ( 'NONE',  ( 1.000000000000000000, 0.000000000000000000, 0.000000000000000000 ) ) ;
#9227 = CARTESIAN_POINT ( 'NONE',  ( 0.7746255519315137228, 4.866335056773794854, -53.66500058692498953 ) ) ;
#9228 = ADVANCED_FACE ( 'NONE', ( #2595 ), #17213, .F. ) ;
#9229 = B_SPLINE_CURVE_WITH_KNOTS ( 'NONE', 1,
 ( #11392, #20989 ),
 .UNSPECIFIED., .F., .F.,
 ( 2, 2 ),
 ( -2.555882144480000001E-06, 0.7000000000009999335 ),
 .UNSPECIFIED. ) ;
#9230 = DIRECTION ( 'NONE',  ( -1.000000000000000000, 1.224606353819999829E-16, 0.000000000000000000 ) ) ;
#9231 = DIRECTION ( 'NONE',  ( 0.000000000000000000, 0.000000000000000000, -1.000000000000000000 ) ) ;
#9232 = CARTESIAN_POINT ( 'NONE',  ( 2.020725942159999899, -3.500000000000000000, 230.5235986622430175 ) ) ;
#9233 = CARTESIAN_POINT ( 'NONE',  ( -0.2182390032459076146, -27.49908342132812322, 223.9122931967829970 ) ) ;
#9234 = CARTESIAN_POINT ( 'NONE',  ( 9.738910687886932038, -24.96785170200595161, 93.21714158839999698 ) ) ;
#9235 = EDGE_CURVE ( 'NONE', #12069, #13409, #11946, .T. ) ;
#9236 = CARTESIAN_POINT ( 'NONE',  ( 2.743362564037614248, -4.941860934411918649, -56.06172062782499665 ) ) ;
#9237 = AXIS2_PLACEMENT_3D ( 'NONE', #3895, #4205, #2010 ) ;
#9238 = VERTEX_POINT ( 'NONE', #24305 ) ;
#9239 = AXIS2_PLACEMENT_3D ( 'NONE', #30727, #11531, #21132 ) ;
#9240 = AXIS2_PLACEMENT_3D ( 'NONE', #6522, #23378, #18478 ) ;
#9241 = ORIENTED_EDGE ( 'NONE', *, *, #1101, .F. ) ;
#9242 = DIRECTION ( 'NONE',  ( 0.000000000000000000, 0.000000000000000000, -1.000000000000000000 ) ) ;
#9243 = ORIENTED_EDGE ( 'NONE', *, *, #20954, .T. ) ;
#9244 = DIRECTION ( 'NONE',  ( 1.000000000000000000, -1.224606353819999582E-16, 0.000000000000000000 ) ) ;
#9245 = ADVANCED_FACE ( 'NONE', ( #5263, #14252 ), #9672, .F. ) ;
#9246 = CARTESIAN_POINT ( 'NONE',  ( -24.09883371379999772, -15.21565466309999870, 225.0000014190000002 ) ) ;
#9247 = SURFACE_STYLE_USAGE ( .BOTH. , #19479 ) ;
#9248 = DIRECTION ( 'NONE',  ( 1.000000000000000000, 0.000000000000000000, 0.000000000000000000 ) ) ;
#9249 = CARTESIAN_POINT ( 'NONE',  ( -24.07583586439999834, -13.90018868249999962, 223.9000014189999774 ) ) ;
#9250 = CARTESIAN_POINT ( 'NONE',  ( -3.552713678799999608E-15, 0.000000000000000000, 36.39444872449999480 ) ) ;
#9251 = CARTESIAN_POINT ( 'NONE',  ( 2.246931792404676997, -6.149078805876593279, -6.260585232200001293 ) ) ;
#9252 = COLOUR_RGB ( '', 0.09019608, 0.27058824, 0.51372549) ;
#9253 = CARTESIAN_POINT ( 'NONE',  ( -27.56257419720000357, -10.12653142719999799, 230.5592437530000041 ) ) ;
#9254 = EDGE_LOOP ( 'NONE', ( #1686, #28328, #28141, #7595 ) ) ;
#9255 = DIRECTION ( 'NONE',  ( 0.000000000000000000, 2.259525899719999991E-12, 1.000000000000000000 ) ) ;
#9256 = CARTESIAN_POINT ( 'NONE',  ( 4.130711734062736618, 1.221343755424965316, -17.54190840230000248 ) ) ;
#9257 = CARTESIAN_POINT ( 'NONE',  ( -27.79999999999999716, -2.356913896269999927E-11, 224.8000000000000114 ) ) ;
#9258 = CARTESIAN_POINT ( 'NONE',  ( -8.699999999694114194, -28.22468611108677194, -31.13863906519358693 ) ) ;
#9259 = EDGE_CURVE ( 'NONE', #29063, #18612, #6730, .T. ) ;
#9260 = AXIS2_PLACEMENT_3D ( 'NONE', #26616, #24109, #14668 ) ;
#9261 = CARTESIAN_POINT ( 'NONE',  ( -0.09707459578013553914, -26.79999999950000955, 6.099999999999997868 ) ) ;
#9262 = CARTESIAN_POINT ( 'NONE',  ( -24.11017618899999704, -13.84060607850000046, 223.9013449680000178 ) ) ;
#9263 = AXIS2_PLACEMENT_3D ( 'NONE', #13411, #8366, #3979 ) ;
#9264 = CARTESIAN_POINT ( 'NONE',  ( -7.999999999634344938, -21.57658477890130655, -40.40133997131670185 ) ) ;
#9265 = CARTESIAN_POINT ( 'NONE',  ( -2.036891525988612894, -5.569677580567498509, -43.50640794712499826 ) ) ;
#9266 = VECTOR ( 'NONE', #22360, 1000.000000000000000 ) ;
#9267 = LINE ( 'NONE', #20929, #7695 ) ;
#9268 = CARTESIAN_POINT ( 'NONE',  ( -1.430228209136418238, -3.227294851201703896, 226.6412452697749700 ) ) ;
#9269 = FACE_OUTER_BOUND ( 'NONE', #1206, .T. ) ;
#9270 = CARTESIAN_POINT ( 'NONE',  ( 2.020725942159999899, 3.500000000000000000, 230.5235986622430175 ) ) ;
#9271 = EDGE_LOOP ( 'NONE', ( #18914, #10534, #22295, #23003 ) ) ;
#9272 = CARTESIAN_POINT ( 'NONE',  ( 4.644419429734489846, -31.74345175796718621, -80.43200112173411753 ) ) ;
#9273 = CARTESIAN_POINT ( 'NONE',  ( -12.29999999970000069, -32.40000000036999950, -28.40000000001083080 ) ) ;
#9274 = CARTESIAN_POINT ( 'NONE',  ( -24.11017618899999704, -13.84060607850000046, 223.9013449680000178 ) ) ;
#9275 = EDGE_CURVE ( 'NONE', #25912, #7575, #25872, .T. ) ;
#9276 = AXIS2_PLACEMENT_3D ( 'NONE', #7448, #9499, #19100 ) ;
#9277 = CYLINDRICAL_SURFACE ( 'NONE', #13697, 26.80000000000002203 ) ;
#9278 =( GEOMETRIC_REPRESENTATION_CONTEXT ( 3 ) GLOBAL_UNCERTAINTY_ASSIGNED_CONTEXT ( ( #2150 ) ) GLOBAL_UNIT_ASSIGNED_CONTEXT ( ( #3991, #18302, #23512 ) ) REPRESENTATION_CONTEXT ( 'NONE', 'WORKASPACE' ) );
#9279 = ORIENTED_EDGE ( 'NONE', *, *, #17819, .F. ) ;
#9280 = CARTESIAN_POINT ( 'NONE',  ( -2.036891525988612894, -5.569677580567498509, -44.46640794712500622 ) ) ;
#9281 = VERTEX_POINT ( 'NONE', #3355 ) ;
#9282 = ORIENTED_EDGE ( 'NONE', *, *, #1741, .T. ) ;
#9283 = EDGE_CURVE ( 'NONE', #28570, #24922, #26533, .T. ) ;
#9284 =( NAMED_UNIT ( * ) SI_UNIT ( $, .STERADIAN. ) SOLID_ANGLE_UNIT ( ) );
#9285 = ORIENTED_EDGE ( 'NONE', *, *, #12162, .T. ) ;
#9286 = CARTESIAN_POINT ( 'NONE',  ( -1.421085471519999843E-14, -1.421085471519999843E-14, 87.93968498540000667 ) ) ;
#9287 = VECTOR ( 'NONE', #4367, 999.9999999999998863 ) ;
#9288 = ORIENTED_EDGE ( 'NONE', *, *, #29785, .F. ) ;
#9290 = CARTESIAN_POINT ( 'NONE',  ( -24.60124998910000116, -12.94761260449999973, 225.2084371580000095 ) ) ;
#9289 = AXIS2_PLACEMENT_3D ( 'NONE', #30540, #25348, #15579 ) ;
#9291 = CARTESIAN_POINT ( 'NONE',  ( 23.98258507289250474, 15.39789216307533160, 4.239862992999999136 ) ) ;
#9292 = CARTESIAN_POINT ( 'NONE',  ( -10.35000000009999965, -130.0000000000000000, -42.40000000045999684 ) ) ;
#9293 = DIRECTION ( 'NONE',  ( -0.000000000000000000, 0.5000000000001900702, 0.8660254037843290176 ) ) ;
#9294 = CARTESIAN_POINT ( 'NONE',  ( 19.67976622696308198, 20.00040984567383617, -0.1488513631577831065 ) ) ;
#9295 = CARTESIAN_POINT ( 'NONE',  ( 14.40197535836999876, -22.00000000000000000, -31.28675134584999640 ) ) ;
#9296 = CARTESIAN_POINT ( 'NONE',  ( -8.000000000050000892, -13.98526668056139144, -73.96855033896248699 ) ) ;
#9297 = CARTESIAN_POINT ( 'NONE',  ( -8.999999999883337765, 20.99999999999999645, -44.83820061220109210 ) ) ;
#9298 = VERTEX_POINT ( 'NONE', #22718 ) ;
#9299 = CARTESIAN_POINT ( 'NONE',  ( -2.723504195107721237, -4.795398582787750108, -7.685065142700002738 ) ) ;
#9300 = CIRCLE ( 'NONE', #10810, 3.176829269159998859 ) ;
#9301 = CARTESIAN_POINT ( 'NONE',  ( -4.913246905806704312, -2.484498147601009510, -26.96472909260000250 ) ) ;
#9302 = DIRECTION ( 'NONE',  ( -0.8660254037843290176, 0.5000000000001899592, -1.018673689593249976E-32 ) ) ;
#9303 = AXIS2_PLACEMENT_3D ( 'NONE', #12624, #22086, #15303 ) ;
#9304 = CARTESIAN_POINT ( 'NONE',  ( -3.635410520752169194, -1.296028149944132402, -93.15928300860232980 ) ) ;
#9305 = CARTESIAN_POINT ( 'NONE',  ( -7.132997404018626142, -115.1185614902475436, 21.95989595831449748 ) ) ;
#9306 = DIRECTION ( 'NONE',  ( -2.764840495839172918E-12, -0.9128796883888953273, 0.4082287037029531107 ) ) ;
#9307 = CARTESIAN_POINT ( 'NONE',  ( -23.83777999500000178, -14.30502388290000049, 226.0028091380000035 ) ) ;
#9308 = B_SPLINE_CURVE_WITH_KNOTS ( 'NONE', 5,
 ( #510, #27227, #8023, #9783, #10248, #21741, #5364, #29273, #29123, #7717, #10094, #21908, #19384, #24416, #29431 ),
 .UNSPECIFIED., .F., .F.,
 ( 6, 3, 3, 3, 6 ),
 ( 0.000000000000000000, 0.1000000000028630903, 0.3999999999999999667, 0.7000000000005727196, 1.000000000000000000 ),
 .UNSPECIFIED. ) ;
#9309 = DIRECTION ( 'NONE',  ( 0.000000000000000000, 0.000000000000000000, -1.000000000000000000 ) ) ;
#9310 = CARTESIAN_POINT ( 'NONE',  ( 0.5401834767575381946, -27.79499634052776358, 6.099998581000020792 ) ) ;
#9311 = CARTESIAN_POINT ( 'NONE',  ( -22.38914258936776491, -14.77116484369720339, -1.399999999999998579 ) ) ;
#9312 = ORIENTED_EDGE ( 'NONE', *, *, #4885, .T. ) ;
#9313 = CARTESIAN_POINT ( 'NONE',  ( -21.97984812610000205, 17.61343233899999916, 229.2930777540000236 ) ) ;
#9314 = EDGE_LOOP ( 'NONE', ( #3208, #23603, #3510, #25476 ) ) ;
#9315 = DIRECTION ( 'NONE',  ( -0.1090476345695678556, -0.6986477033489640887, -0.7071067811865475727 ) ) ;
#9316 = FACE_OUTER_BOUND ( 'NONE', #12687, .T. ) ;
#9317 = ORIENTED_EDGE ( 'NONE', *, *, #16848, .T. ) ;
#9318 = DIRECTION ( 'NONE',  ( 0.1090476345695682997, 0.6986477033489653099, 0.7071067811865462405 ) ) ;
#9319 = CARTESIAN_POINT ( 'NONE',  ( 8.699999999505822146, -29.73863906516063693, -27.17531388883607590 ) ) ;
#9320 = ADVANCED_FACE ( 'NONE', ( #30112 ), #17523, .F. ) ;
#9321 = EDGE_LOOP ( 'NONE', ( #5914, #7202, #7427, #9940 ) ) ;
#9322 = ORIENTED_EDGE ( 'NONE', *, *, #15087, .T. ) ;
#9323 = ORIENTED_EDGE ( 'NONE', *, *, #12491, .F. ) ;
#9324 = ORIENTED_EDGE ( 'NONE', *, *, #28426, .F. ) ;
#9325 = CARTESIAN_POINT ( 'NONE',  ( -17.49999999969999820, -29.61919234679800894, -29.91462304360321411 ) ) ;
#9326 = ADVANCED_FACE ( 'NONE', ( #712 ), #20048, .T. ) ;
#9327 = ADVANCED_FACE ( 'NONE', ( #20355 ), #29645, .T. ) ;
#9328 = PRODUCT_DEFINITION_FORMATION_WITH_SPECIFIED_SOURCE ( 'ANY', '', #3526, .NOT_KNOWN. ) ;
#9329 = CARTESIAN_POINT ( 'NONE',  ( -8.699999999656061078, -13.80112230385522487, -36.85362565245412725 ) ) ;
#9330 = CARTESIAN_POINT ( 'NONE',  ( -1.560798555979769464, 4.306275027539294697, -68.40099036452500059 ) ) ;
#9331 = PRESENTATION_STYLE_ASSIGNMENT (( #14066 ) ) ;
#9332 = CARTESIAN_POINT ( 'NONE',  ( 24.58974021188865322, -12.96866346451374774, 225.2881025212954000 ) ) ;
#9333 = CARTESIAN_POINT ( 'NONE',  ( -8.035257673360000297, -26.87837576509999593, 222.0000000000000000 ) ) ;
#9334 = CARTESIAN_POINT ( 'NONE',  ( 1.127732790480000080, -28.47784299079999926, 225.1040528159999781 ) ) ;
#9335 = ORIENTED_EDGE ( 'NONE', *, *, #7893, .F. ) ;
#9336 = CARTESIAN_POINT ( 'NONE',  ( 11.69999999989999928, -24.11120071670000087, -0.6999999999999992895 ) ) ;
#9337 = CARTESIAN_POINT ( 'NONE',  ( 1.942707423728255778, -5.758494596869851989, -14.66414732020000855 ) ) ;
#9338 = CARTESIAN_POINT ( 'NONE',  ( 2.107992564109750333, -27.41908764619381245, 20.00000000000000355 ) ) ;
#9339 = CARTESIAN_POINT ( 'NONE',  ( -1.906343950897046113, -12.18129130007007888, 232.6627637558541437 ) ) ;
#9340 = ORIENTED_EDGE ( 'NONE', *, *, #28092, .T. ) ;
#9341 = DIRECTION ( 'NONE',  ( -0.7071067811780483714, -0.6644630243965946592, -0.2418447626510653037 ) ) ;
#9342 = CARTESIAN_POINT ( 'NONE',  ( 0.9015611980529183445, -28.48625233387473799, 3.957673652000032405 ) ) ;
#9343 = CARTESIAN_POINT ( 'NONE',  ( -23.03132590089999709, 15.56947127769999994, 222.0000000000000000 ) ) ;
#9344 = CARTESIAN_POINT ( 'NONE',  ( 22.63996098036280458, -14.34127493679882903, 4.854121447380539855 ) ) ;
#9345 = DIRECTION ( 'NONE',  ( 0.000000000000000000, 0.3420201433259318358, -0.9396926207858125046 ) ) ;
#9346 = CARTESIAN_POINT ( 'NONE',  ( 9.999999999959999997, -24.95051888640000115, -26.20881396970000310 ) ) ;
#9347 = CARTESIAN_POINT ( 'NONE',  ( -16.83342759582943060, -8.999999999996580513, -0.6999999999999784173 ) ) ;
#9348 = ORIENTED_EDGE ( 'NONE', *, *, #9999, .T. ) ;
#9349 = CARTESIAN_POINT ( 'NONE',  ( -10.69999999999999929, -24.03509441459999962, -28.95432817779999723 ) ) ;
#9350 = CARTESIAN_POINT ( 'NONE',  ( -17.52370712817340248, -8.131162915109298339, -0.6999999999999784173 ) ) ;
#9351 = EDGE_CURVE ( 'NONE', #15990, #19446, #8223, .T. ) ;
#9352 = CARTESIAN_POINT ( 'NONE',  ( -27.79539923781684863, -0.5057481689248937151, 0.8585786439999909536 ) ) ;
#9353 = CARTESIAN_POINT ( 'NONE',  ( -4.679640823766034963, -1.817694234202872350, -68.10000000002500542 ) ) ;
#9354 = CARTESIAN_POINT ( 'NONE',  ( 17.16657240420000008, 10.97998838177520931, 0.5194763363741546902 ) ) ;
#9355 = CARTESIAN_POINT ( 'NONE',  ( -4.500610150543032262, 1.045894616594410076, -44.10000000002499831 ) ) ;
#9356 = ORIENTED_EDGE ( 'NONE', *, *, #17106, .T. ) ;
#9357 = CARTESIAN_POINT ( 'NONE',  ( 9.993285220779439371, -25.61999708228226069, 115.0000000000000000 ) ) ;
#9358 = CARTESIAN_POINT ( 'NONE',  ( -4.155524648305278568, -2.455537445457764978, -68.72382590962500615 ) ) ;
#9359 = ORIENTED_EDGE ( 'NONE', *, *, #24049, .F. ) ;
#9360 = LINE ( 'NONE', #16602, #15425 ) ;
#9361 = B_SPLINE_CURVE_WITH_KNOTS ( 'NONE', 5,
 ( #25214, #3645, #24483, #30090, #8516, #18117 ),
 .UNSPECIFIED., .F., .F.,
 ( 6, 6 ),
 ( 0.000000000000000000, 24.02090357630000028 ),
 .UNSPECIFIED. ) ;
#9362 = CARTESIAN_POINT ( 'NONE',  ( -1.650988191866306742, 3.989749455477753504, -57.14652090042499566 ) ) ;
#9363 = ORIENTED_EDGE ( 'NONE', *, *, #2854, .T. ) ;
#9364 = CARTESIAN_POINT ( 'NONE',  ( -9.999999999909999104, -2.500000000000002220, -2.399999999999999467 ) ) ;
#9365 = DIRECTION ( 'NONE',  ( 0.000000000000000000, -1.000000000000000000, 2.257145581549999994E-12 ) ) ;
#9366 = DIRECTION ( 'NONE',  ( 2.965499939100700266E-25, -1.000000000000000000, 2.257145581549900232E-12 ) ) ;
#9367 = CARTESIAN_POINT ( 'NONE',  ( -17.04621913067799710, -22.00000000000000000, -31.28675134614999820 ) ) ;
#9368 = CARTESIAN_POINT ( 'NONE',  ( -13.00000000000000000, 24.54213077165692525, -59.94572446259928711 ) ) ;
#9369 = CARTESIAN_POINT ( 'NONE',  ( -10.00000000050000004, -29.23060343719999921, -26.39054106440000069 ) ) ;
#9370 = VERTEX_POINT ( 'NONE', #27130 ) ;
#9371 = CARTESIAN_POINT ( 'NONE',  ( 23.55411374389464285, 16.04538543789061933, 8.000000000000007105 ) ) ;
#9372 = ADVANCED_FACE ( 'NONE', ( #22255 ), #8937, .F. ) ;
#9373 = PLANE ( 'NONE',  #17287 ) ;
#9374 = FACE_OUTER_BOUND ( 'NONE', #6829, .T. ) ;
#9375 = EDGE_CURVE ( 'NONE', #20468, #12912, #427, .T. ) ;
#9376 = CARTESIAN_POINT ( 'NONE',  ( -9.897162125400486232, -25.37356426577148127, 38.33953982530000104 ) ) ;
#9377 = CARTESIAN_POINT ( 'NONE',  ( 10.89131017080000063, -24.86557399950000047, -1.811764705399995901 ) ) ;
#9378 = CARTESIAN_POINT ( 'NONE',  ( 7.636616881710000193, 9.305349148710000406, 230.6412452697800006 ) ) ;
#9379 = APPLICATION_CONTEXT ( 'automotive_design' ) ;
#9380 = CARTESIAN_POINT ( 'NONE',  ( 17.16657240420000008, -9.000000000000001776, -0.8000000000000020428 ) ) ;
#9381 = DIRECTION ( 'NONE',  ( 0.3633921898465291567, 0.9316362575375349842, 0.000000000000000000 ) ) ;
#9382 = CARTESIAN_POINT ( 'NONE',  ( 0.000000000000000000, -2.000000000000000000, 227.6412452703700069 ) ) ;
#9383 = CARTESIAN_POINT ( 'NONE',  ( -3.221934060415182710, 3.671197199736151440, -53.58587006832498645 ) ) ;
#9384 = EDGE_CURVE ( 'NONE', #24262, #11888, #22842, .T. ) ;
#9385 = CIRCLE ( 'NONE', #27986, 3.200000000000000178 ) ;
#9386 = CARTESIAN_POINT ( 'NONE',  ( 8.359832557563507294, -8.751033282714830719, 232.0000002394077683 ) ) ;
#9387 = CARTESIAN_POINT ( 'NONE',  ( -16.25056150175689496, -8.060002615884259924, 0.000000000000000000 ) ) ;
#9388 = CARTESIAN_POINT ( 'NONE',  ( 0.000000000000000000, 0.000000000000000000, 136.3944487260000074 ) ) ;
#9389 = B_SPLINE_CURVE_WITH_KNOTS ( 'NONE', 3,
 ( #6965, #11535, #19080, #7117, #26470, #26623, #26164, #17023, #21602, #21442 ),
 .UNSPECIFIED., .F., .F.,
 ( 4, 2, 2, 2, 4 ),
 ( 0.000000000000000000, 0.2500000000000000000, 0.5000000000000000000, 0.7500000000000000000, 1.000000000000000000 ),
 .UNSPECIFIED. ) ;
#9390 = B_SPLINE_CURVE_WITH_KNOTS ( 'NONE', 3,
 ( #18949, #21473, #4332, #26195, #11715, #25736 ),
 .UNSPECIFIED., .F., .F.,
 ( 4, 2, 4 ),
 ( 0.000000000000000000, 0.5000000000000000000, 1.000000000000000000 ),
 .UNSPECIFIED. ) ;
#9391 = ORIENTED_EDGE ( 'NONE', *, *, #11633, .T. ) ;
#9392 = DIRECTION ( 'NONE',  ( 0.000000000000000000, -0.8660254037843289066, 0.5000000000001899592 ) ) ;
#9393 = ORIENTED_EDGE ( 'NONE', *, *, #15927, .T. ) ;
#9394 = CARTESIAN_POINT ( 'NONE',  ( -24.66442003930000126, -14.28072947929999970, 223.9000014189999774 ) ) ;
#9395 = EDGE_CURVE ( 'NONE', #19325, #7575, #10085, .T. ) ;
#9396 = CARTESIAN_POINT ( 'NONE',  ( -0.06088579265679563285, 5.203211362304668519, -58.11818518972498993 ) ) ;
#9397 = VERTEX_POINT ( 'NONE', #25237 ) ;
#9398 = VERTEX_POINT ( 'NONE', #15166 ) ;
#9399 = CARTESIAN_POINT ( 'NONE',  ( -17.45644675878136098, -30.19649537162369057, -32.32803605695916360 ) ) ;
#9400 = EDGE_LOOP ( 'NONE', ( #28401, #18922, #20863, #20723 ) ) ;
#9401 = DIRECTION ( 'NONE',  ( -1.000000000000000000, 1.224606353819999829E-16, 0.000000000000000000 ) ) ;
#9402 = DIRECTION ( 'NONE',  ( 0.000000000000000000, 0.000000000000000000, -1.000000000000000000 ) ) ;
#9403 = CARTESIAN_POINT ( 'NONE',  ( 9.620427249210001364, 19.99999999999999645, -43.18760499467699532 ) ) ;
#9404 = AXIS2_PLACEMENT_3D ( 'NONE', #22460, #17259, #17867 ) ;
#9405 = B_SPLINE_CURVE_WITH_KNOTS ( 'NONE', 3,
 ( #21040, #30640, #2001, #9066, #18661, #1372 ),
 .UNSPECIFIED., .F., .F.,
 ( 4, 2, 4 ),
 ( 0.000000000000000000, 0.5000000000000000000, 1.000000000000000000 ),
 .UNSPECIFIED. ) ;
#9406 = AXIS2_PLACEMENT_3D ( 'NONE', #18222, #8624, #15882 ) ;
#9407 = CARTESIAN_POINT ( 'NONE',  ( 0.4162902733250000153, -12.33263093849999947, 232.6627648150000027 ) ) ;
#9408 = CARTESIAN_POINT ( 'NONE',  ( 9.738910687886868089, -24.96785170200598358, 202.0000000000000000 ) ) ;
#9409 = CARTESIAN_POINT ( 'NONE',  ( 0.000000000000000000, 0.000000000000000000, 40.00000000000000000 ) ) ;
#9410 = CARTESIAN_POINT ( 'NONE',  ( -2.320012200738846619, 5.013958306206127702, -6.731725184299999221 ) ) ;
#9411 = CARTESIAN_POINT ( 'NONE',  ( 21.16705260759999874, -21.30254494150000255, 229.2404163060000144 ) ) ;
#9412 = ORIENTED_EDGE ( 'NONE', *, *, #7586, .T. ) ;
#9413 = CARTESIAN_POINT ( 'NONE',  ( -24.62906106470000012, -14.34164290000000008, 223.9040321109999923 ) ) ;
#9414 = CARTESIAN_POINT ( 'NONE',  ( 0.7420639427752478978, -6.011517603930927045, -18.97054674910000927 ) ) ;
#9415 = CARTESIAN_POINT ( 'NONE',  ( -1.419173393149999842E-06, -27.80022181310000207, 226.1000014189999945 ) ) ;
#9416 = CARTESIAN_POINT ( 'NONE',  ( 24.50348397774029152, -13.13223627703424690, 6.042507865999996675 ) ) ;
#9417 = FACE_OUTER_BOUND ( 'NONE', #5488, .T. ) ;
#9418 = CARTESIAN_POINT ( 'NONE',  ( 27.50000000000000000, -3.367667472999999580E-15, 193.6055512739999926 ) ) ;
#9419 = CARTESIAN_POINT ( 'NONE',  ( 0.6626488065419183782, -5.424947836070461271, -42.98057807742500103 ) ) ;
#9420 = EDGE_CURVE ( 'NONE', #9747, #24348, #27433, .T. ) ;
#9421 = B_SPLINE_CURVE_WITH_KNOTS ( 'NONE', 3,
 ( #29551, #8292, #10520, #3578, #17585, #17887, #22782, #27346, #29857, #1233, #10834, #7833, #12713, #5791, #27195, #5633, #20420, #30012, #8445, #29707, #17435, #24986, #13023, #18045, #10366, #22633 ),
 .UNSPECIFIED., .F., .F.,
 ( 4, 2, 2, 2, 1, 1, 1, 1, 1, 1, 2, 2, 2, 2, 2, 4 ),
 ( 0.000000000000000000, 0.2499999999999553690, 0.3749999999999330536, 0.4374999999999219513, 0.4687499999999163447, 0.4843749999999137912, 0.4921874999999124034, 0.4960937499999118483, 0.4980468749999114042, 0.4990234374999112377, 0.4995117187499112932, 0.4999999999999112932, 0.6249999999999333866, 0.7499999999999554801, 0.8749999999999776845, 1.000000000000000000 ),
 .UNSPECIFIED. ) ;
#9422 = CARTESIAN_POINT ( 'NONE',  ( 7.505215711137140033, -5.625030866512529037, -27.14390223597047935 ) ) ;
#9423 = CARTESIAN_POINT ( 'NONE',  ( -23.61599683758278800, -12.66993935690586959, 4.280684604083014655 ) ) ;
#9424 = CARTESIAN_POINT ( 'NONE',  ( -24.45473033751197178, -14.63622298155413226, 6.098654221000004760 ) ) ;
#9425 = CARTESIAN_POINT ( 'NONE',  ( -10.99999999969999998, 21.69999999919999212, -70.09999999999999432 ) ) ;
#9426 = ORIENTED_EDGE ( 'NONE', *, *, #2913, .T. ) ;
#9427 = VECTOR ( 'NONE', #1520, 1000.000000000000000 ) ;
#9428 = CARTESIAN_POINT ( 'NONE',  ( -9.999999999909999104, 19.99999999999999645, -2.399999999999999467 ) ) ;
#9429 = PRESENTATION_STYLE_ASSIGNMENT (( #6917 ) ) ;
#9430 = VECTOR ( 'NONE', #22042, 1000.000000000000114 ) ;
#9431 = DIRECTION ( 'NONE',  ( 1.000000000000000000, 0.000000000000000000, 0.000000000000000000 ) ) ;
#9432 = ORIENTED_EDGE ( 'NONE', *, *, #16742, .T. ) ;
#9433 = ADVANCED_FACE ( 'NONE', ( #22882 ), #19900, .F. ) ;
#9434 = CARTESIAN_POINT ( 'NONE',  ( -25.94284618478186744, -6.948772836044545542, 186.7828584126666840 ) ) ;
#9435 = DIRECTION ( 'NONE',  ( 1.000000000000000000, 0.000000000000000000, 0.000000000000000000 ) ) ;
#9436 = VERTEX_POINT ( 'NONE', #10918 ) ;
#9437 = ORIENTED_EDGE ( 'NONE', *, *, #8997, .F. ) ;
#9438 = EDGE_CURVE ( 'NONE', #15475, #22567, #15976, .T. ) ;
#9439 = DIRECTION ( 'NONE',  ( 1.000000000000000000, 0.000000000000000000, 0.000000000000000000 ) ) ;
#9440 = ORIENTED_EDGE ( 'NONE', *, *, #11935, .T. ) ;
#9441 = FACE_OUTER_BOUND ( 'NONE', #1374, .T. ) ;
#9442 = EDGE_CURVE ( 'NONE', #1647, #8375, #21677, .T. ) ;
#9443 = ORIENTED_EDGE ( 'NONE', *, *, #28292, .F. ) ;
#9444 = CARTESIAN_POINT ( 'NONE',  ( -10.35000000039999968, -130.0000000000000000, -41.24671599790000442 ) ) ;
#9445 = CARTESIAN_POINT ( 'NONE',  ( 7.453090060300409547, -2.907137518772282991, 20.00000000000000000 ) ) ;
#9446 = CARTESIAN_POINT ( 'NONE',  ( 24.49999999589999788, -3.000285566359999846E-15, 140.0000000000000000 ) ) ;
#9447 = CARTESIAN_POINT ( 'NONE',  ( 0.2496999827216928036, 4.399169623874717772, -35.69999999999998863 ) ) ;
#9448 = AXIS2_PLACEMENT_3D ( 'NONE', #12466, #4351, #24439 ) ;
#9449 = EDGE_CURVE ( 'NONE', #8336, #16248, #7068, .T. ) ;
#9450 = CARTESIAN_POINT ( 'NONE',  ( 17.14656078602323319, -7.900182044548062166, -1.000005633855494125E-09 ) ) ;
#9451 = CARTESIAN_POINT ( 'NONE',  ( -3.305579555868532804, -1.864813555827612879, -0.6999999999999992895 ) ) ;
#9452 = DIRECTION ( 'NONE',  ( 1.000000000000000000, 0.000000000000000000, 0.000000000000000000 ) ) ;
#9453 = CARTESIAN_POINT ( 'NONE',  ( -17.99591469510000152, 19.96082041680000074, 229.9999991770000065 ) ) ;
#9454 = AXIS2_PLACEMENT_3D ( 'NONE', #14490, #4731, #16676 ) ;
#9455 = CARTESIAN_POINT ( 'NONE',  ( -4.598206294437411579, -3.044638162784917945, -7.889929326000002519 ) ) ;
#9456 = CARTESIAN_POINT ( 'NONE',  ( 4.807767551039155762, 1.738376938488521040, -25.57499766020000109 ) ) ;
#9457 = CARTESIAN_POINT ( 'NONE',  ( -0.01829671460840276778, -3.547951512854698564, 0.000000000000000000 ) ) ;
#9459 = ADVANCED_FACE ( 'NONE', ( #6656 ), #6942, .F. ) ;
#9458 = VECTOR ( 'NONE', #17610, 1000.000000000000000 ) ;
#9460 = CARTESIAN_POINT ( 'NONE',  ( 23.63672937736964030, -12.63153181622180554, 225.6766013745815940 ) ) ;
#9461 = DIRECTION ( 'NONE',  ( 0.000000000000000000, 0.000000000000000000, 1.000000000000000000 ) ) ;
#9462 = CARTESIAN_POINT ( 'NONE',  ( -17.13980697764020178, 12.06576768890603013, -0.6999999999999785283 ) ) ;
#9463 = CARTESIAN_POINT ( 'NONE',  ( 4.262818619062177738, -0.7545854518158021662, -8.771482634699998115 ) ) ;
#9464 = B_SPLINE_CURVE_WITH_KNOTS ( 'NONE', 3,
 ( #7361, #19477, #24051, #26559, #5000, #21531, #30971, #5310 ),
 .UNSPECIFIED., .F., .F.,
 ( 4, 2, 2, 4 ),
 ( 0.000000000000000000, 0.2500000000000000000, 0.5000000000000000000, 1.000000000000000000 ),
 .UNSPECIFIED. ) ;
#9465 = PRODUCT_DEFINITION_SHAPE ( 'NONE', 'NONE',  #31132 ) ;
#9466 = B_SPLINE_CURVE_WITH_KNOTS ( 'NONE', 1,
 ( #16727, #26190 ),
 .UNSPECIFIED., .F., .F.,
 ( 2, 2 ),
 ( -2.557302930970000000E-06, 0.7000000000009999335 ),
 .UNSPECIFIED. ) ;
#9467 = CARTESIAN_POINT ( 'NONE',  ( 27.53132593009999951, 1.219166508230000085E-11, 229.7313259299999686 ) ) ;
#9468 = CARTESIAN_POINT ( 'NONE',  ( 1.776356839399999922E-14, 0.000000000000000000, 232.6627637660000119 ) ) ;
#9469 = CARTESIAN_POINT ( 'NONE',  ( -9.993285220779545952, -25.61999708228220740, 93.60555127549999099 ) ) ;
#9470 = ORIENTED_EDGE ( 'NONE', *, *, #19531, .T. ) ;
#9471 = EDGE_CURVE ( 'NONE', #19001, #26338, #30705, .T. ) ;
#9472 = VECTOR ( 'NONE', #8746, 1000.000000000000114 ) ;
#9473 = ORIENTED_EDGE ( 'NONE', *, *, #9801, .F. ) ;
#9474 = DIRECTION ( 'NONE',  ( 0.000000000000000000, -1.000000000000000000, 0.000000000000000000 ) ) ;
#9475 = CARTESIAN_POINT ( 'NONE',  ( 4.129834804004070214, 5.047645050185102455, -20.25622222230000347 ) ) ;
#9476 = ORIENTED_EDGE ( 'NONE', *, *, #19917, .F. ) ;
#9477 = CARTESIAN_POINT ( 'NONE',  ( 25.22036945370000183, -13.27344566769999901, 225.2083619149999834 ) ) ;
#9478 = CARTESIAN_POINT ( 'NONE',  ( 22.97726876109999949, 16.89265187250000011, 222.9999999789999947 ) ) ;
#9479 = ORIENTED_EDGE ( 'NONE', *, *, #15863, .F. ) ;
#9480 = CIRCLE ( 'NONE', #21547, 0.9999999999999991118 ) ;
#9481 = VERTEX_POINT ( 'NONE', #1487 ) ;
#9482 = EDGE_LOOP ( 'NONE', ( #25356, #19932, #27849, #29752 ) ) ;
#9483 = SURFACE_STYLE_USAGE ( .BOTH. , #14211 ) ;
#9484 = ORIENTED_EDGE ( 'NONE', *, *, #8642, .T. ) ;
#9485 = CARTESIAN_POINT ( 'NONE',  ( 26.84464184930000030, -3.287411897459999980E-15, 37.43750406050000379 ) ) ;
#9486 = TOROIDAL_SURFACE ( 'NONE', #6469, 18.16530045470000232, 1.699999999999999956 ) ;
#9487 = CARTESIAN_POINT ( 'NONE',  ( 28.50000000000000000, -5.921189464669998951E-16, 222.0000000000000000 ) ) ;
#9488 = CARTESIAN_POINT ( 'NONE',  ( 0.000000000000000000, 0.000000000000000000, 192.0603150150000147 ) ) ;
#9489 = VERTEX_POINT ( 'NONE', #28375 ) ;
#9490 = DIRECTION ( 'NONE',  ( 0.9595496299847263710, -0.2815395311429191305, 0.000000000000000000 ) ) ;
#9491 = DIRECTION ( 'NONE',  ( 0.000000000000000000, 0.3420201433259318358, -0.9396926207858125046 ) ) ;
#9492 = CARTESIAN_POINT ( 'NONE',  ( -12.74904032510000107, -25.66466679760000247, 222.0000000000000000 ) ) ;
#9493 = CARTESIAN_POINT ( 'NONE',  ( 1.089891362629999971, -28.47934442809999922, 225.3101849020000031 ) ) ;
#9494 = VERTEX_POINT ( 'NONE', #6350 ) ;
#9495 = CARTESIAN_POINT ( 'NONE',  ( -20.05890038391583730, 19.99998511269691193, 0.2505997993269546975 ) ) ;
#9496 = CIRCLE ( 'NONE', #12013, 2.100000000000000089 ) ;
#9497 = B_SPLINE_SURFACE_WITH_KNOTS ( 'NONE', 5, 1, ( 
 ( #23783, #16376 ),
 ( #18731, #21420 ),
 ( #4271, #4109 ),
 ( #21258, #2067 ),
 ( #11658, #20947 ),
 ( #19048, #30857 ),
 ( #9291, #28490 ),
 ( #20790, #31010 ),
 ( #13868, #6781 ),
 ( #23475, #6930 ),
 ( #16529, #30551 ),
 ( #25678, #26140 ),
 ( #8980, #4573 ),
 ( #23313, #14178 ),
 ( #1909, #28646 ) ),
 .UNSPECIFIED., .F., .F., .F.,
 ( 6, 3, 3, 3, 6 ),
 ( 2, 2 ),
 ( 0.000000000000000000, 0.5238999882350000581, 1.047799976470000116, 1.571699964700000063, 1.746333294120000046 ),
 ( -0.7000000000009999335, 2.555897717360000054E-06 ),
 .UNSPECIFIED. ) ;
#9498 = CARTESIAN_POINT ( 'NONE',  ( 5.232234863148874204, 1.547035423556993639, -16.54190840230001669 ) ) ;
#9499 = DIRECTION ( 'NONE',  ( 0.000000000000000000, 0.000000000000000000, -1.000000000000000000 ) ) ;
#9500 = EDGE_CURVE ( 'NONE', #30761, #23469, #23359, .T. ) ;
#9501 = CARTESIAN_POINT ( 'NONE',  ( 0.9007122719980839021, -27.48548889903062431, 5.632980212606629955 ) ) ;
#9502 = EDGE_LOOP ( 'NONE', ( #12697, #13548, #2550, #16189 ) ) ;
#9503 = DIRECTION ( 'NONE',  ( -0.9316362575375349842, 0.3633921898465292122, -0.000000000000000000 ) ) ;
#9504 = FACE_OUTER_BOUND ( 'NONE', #21447, .T. ) ;
#9505 = CARTESIAN_POINT ( 'NONE',  ( 26.80000000000000071, -3.552713678799999608E-15, 93.21714158839999698 ) ) ;
#9506 = EDGE_CURVE ( 'NONE', #24116, #13582, #20674, .T. ) ;
#9507 = DIRECTION ( 'NONE',  ( 1.000000000000000000, 5.998481157687279274E-24, -2.257150022441830001E-12 ) ) ;
#9508 = ADVANCED_FACE ( 'NONE', ( #16413 ), #30270, .T. ) ;
#9509 = DIRECTION ( 'NONE',  ( -0.000000000000000000, -0.000000000000000000, -1.000000000000000000 ) ) ;
#9510 = CIRCLE ( 'NONE', #5477, 4.276011752367109509 ) ;
#9511 = DIRECTION ( 'NONE',  ( 0.000000000000000000, 0.000000000000000000, 1.000000000000000000 ) ) ;
#9513 = EDGE_CURVE ( 'NONE', #1593, #11462, #3403, .T. ) ;
#9512 = CARTESIAN_POINT ( 'NONE',  ( 10.69999999999999929, -127.2537437101000108, -34.36317024011000143 ) ) ;
#9514 = VERTEX_POINT ( 'NONE', #16103 ) ;
#9515 = CARTESIAN_POINT ( 'NONE',  ( -10.00000000052381743, -27.78524365307784549, -31.32191803000652186 ) ) ;
#9516 = CARTESIAN_POINT ( 'NONE',  ( 249981.0602220003202, -207625.5434020000102, -380034.9847440001322 ) ) ;
#9517 =( BOUNDED_CURVE ( )  B_SPLINE_CURVE ( 5, ( #20378, #6372, #25260, #29969, #8562, #15498, #22904, #11408, #23063, #27608, #13610, #21010, #1659, #5891, #27766, #13294, #1344, #13763, #15649, #16124, #18162, #8398, #4014, #3692, #6053, #6210, #25102, #15819, #30614, #1507, #25426, #11251, #9040, #20860, #3535, #11099, #20693, #8721, #23385, #18329, #25735, #30458, #1186, #13131, #8879, #18482, #28081, #4171, #1819, #27450, #22740, #10782, #9188, #21472, #18636, #13927, #6997, #26194, #14085, #26045, #4483, #2286, #25894, #4941, #31069, #4628, #6835, #23535, #28399, #21631, #30918, #28847, #21780, #2122, #23687 ),
 .UNSPECIFIED., .F., .T. ) 
 B_SPLINE_CURVE_WITH_KNOTS ( ( 6, 3, 3, 3, 3, 3, 3, 3, 3, 3, 3, 3, 3, 3, 3, 3, 3, 3, 3, 3, 3, 3, 3, 3, 6 ),
 ( 8.127326494040000071, 11.49596029219999949, 23.35952330949999833, 35.23214498380000492, 46.71570041140000029, 58.48118637179999979, 70.16173614769999745, 81.99711437660000968, 93.33986353700001359, 104.8204913790000035, 116.3828353250000021, 128.2105526469999859, 137.7231253239999944, 147.2120576640000138, 156.6774103699999898, 168.4624398839999913, 180.2684855139999911, 192.1268167670000082, 203.5147100690000173, 215.0810220189999882, 226.8492753339999979, 238.4740513719999910, 250.2932425120000062, 262.1023078380000015, 271.0195818650000206 ),
 .UNSPECIFIED. ) 
 CURVE ( )  GEOMETRIC_REPRESENTATION_ITEM ( )  RATIONAL_B_SPLINE_CURVE ( ( 0.2500000000000000000, 0.2500000000000000000, 0.2500000000000000000, 0.2500000000000000000, 0.2500000000000000000, 0.2500000000000000000, 0.2500000000000000000, 0.2500000000000000000, 0.2500000000000000000, 0.2500000000000000000, 0.2500000000000000000, 0.2500000000000000000, 0.2500000000000000000, 0.2500000000000000000, 0.2500000000000000000, 0.2500000000000000000, 0.2500000000000000000, 0.2500000000000000000, 0.2500000000000000000, 0.2500000000000000000, 0.2500000000000000000, 0.2500000000000000000, 0.2500000000000000000, 0.2500000000000000000, 0.2500000000000000000, 0.2500000000000000000, 0.2500000000000000000, 0.2500000000000000000, 0.2500000000000000000, 0.2500000000000000000, 0.2500000000000000000, 0.2500000000000000000, 0.2500000000000000000, 0.2500000000000000000, 0.2500000000000000000, 0.2500000000000000000, 0.2500000000000000000, 0.2500000000000000000, 0.2500000000000000000, 0.2500000000000000000, 0.2500000000000000000, 0.2500000000000000000, 0.2500000000000000000, 0.2500000000000000000, 0.2500000000000000000, 0.2500000000000000000, 0.2500000000000000000, 0.2500000000000000000, 0.2500000000000000000, 0.2500000000000000000, 0.2500000000000000000, 0.2500000000000000000, 0.2500000000000000000, 0.2500000000000000000, 0.2500000000000000000, 0.2500000000000000000, 0.2500000000000000000, 0.2500000000000000000, 0.2500000000000000000, 0.2500000000000000000, 0.2500000000000000000, 0.2500000000000000000, 0.2500000000000000000, 0.2500000000000000000, 0.2500000000000000000, 0.2500000000000000000, 0.2500000000000000000, 0.2500000000000000000, 0.2500000000000000000, 0.2500000000000000000, 0.2500000000000000000, 0.2500000000000000000, 0.2500000000000000000, 0.2500000000000000000, 0.2500000000000000000 ) ) 
 REPRESENTATION_ITEM ( '' )  );
#9518 = CARTESIAN_POINT ( 'NONE',  ( -26.87967798701711786, 4.135222155429991275, 0.000000000000000000 ) ) ;
#9519 = CARTESIAN_POINT ( 'NONE',  ( -7.861312627708494816, 4.070676187742483521, -39.46457060538356387 ) ) ;
#9520 = VERTEX_POINT ( 'NONE', #2714 ) ;
#9521 = CARTESIAN_POINT ( 'NONE',  ( -3.458129700889219116, 0.5397582531354577773, -88.52261276322501260 ) ) ;
#9522 = FILL_AREA_STYLE ('',( #19429 ) ) ;
#9523 = EDGE_LOOP ( 'NONE', ( #22714, #27501, #6366, #6233 ) ) ;
#9524 = DIRECTION ( 'NONE',  ( 0.000000000000000000, 0.000000000000000000, 1.000000000000000000 ) ) ;
#9525 = CARTESIAN_POINT ( 'NONE',  ( 23.78314118259453380, 14.39461387841678608, 6.098654095000016540 ) ) ;
#9526 = VERTEX_POINT ( 'NONE', #19240 ) ;
#9527 = CARTESIAN_POINT ( 'NONE',  ( -4.637531673247329955, -1.216599033067103264, -25.98406121680000425 ) ) ;
#9528 = DIRECTION ( 'NONE',  ( 0.000000000000000000, 1.000000000000000000, 0.000000000000000000 ) ) ;
#9529 = CIRCLE ( 'NONE', #20085, 27.23548387100000312 ) ;
#9530 = VECTOR ( 'NONE', #28723, 1000.000000000000000 ) ;
#9531 = B_SPLINE_CURVE_WITH_KNOTS ( 'NONE', 3,
 ( #8538, #8693, #18301, #6347, #21714, #7237, #12105, #5335, #26588, #22174 ),
 .UNSPECIFIED., .F., .F.,
 ( 4, 2, 2, 2, 4 ),
 ( 0.000000000000000000, 0.2500000000000000000, 0.5000000000000000000, 0.7500000000000000000, 1.000000000000000000 ),
 .UNSPECIFIED. ) ;
#9532 = CARTESIAN_POINT ( 'NONE',  ( -4.368432077694425431, -0.2718166108138866943, -44.56408784452499106 ) ) ;
#9533 = DIRECTION ( 'NONE',  ( -0.8086898285215826654, 0.000000000000000000, 0.5882352941176968164 ) ) ;
#9534 = FILL_AREA_STYLE ('',( #19439 ) ) ;
#9535 = CARTESIAN_POINT ( 'NONE',  ( 24.43762869010000216, -14.66515636309999948, 223.9972528570000065 ) ) ;
#9536 = CLOSED_SHELL ( 'NONE', ( #11922, #13086, #20326, #21579, #28663, #12544, #27756, #8827, #20360, #7326, #5192, #1986, #21551, #18954, #7797, #15699, #4836, #8231, #16394, #16321, #11428, #16379, #20542, #787, #14379, #20026, #24147, #10812, #4709, #2817, #18229, #21027, #17201, #15987, #22522, #28514, #13872, #29048, #11336, #5654, #22101, #30746 ) ) ;
#9537 = CARTESIAN_POINT ( 'NONE',  ( 3.455337460958629148, 1.015179960318480346, 230.7778176299132156 ) ) ;
#9538 = CARTESIAN_POINT ( 'NONE',  ( 12.84364015881248733, 20.99999999989936228, -69.49900052785271498 ) ) ;
#9539 = DIRECTION ( 'NONE',  ( 0.7757560252248331123, 0.3849708941249066485, 0.5000000000040377701 ) ) ;
#9540 = ORIENTED_EDGE ( 'NONE', *, *, #8341, .F. ) ;
#9541 = CYLINDRICAL_SURFACE ( 'NONE', #20533, 2.999999999999999556 ) ;
#9542 = LINE ( 'NONE', #16153, #13266 ) ;
#9543 = CARTESIAN_POINT ( 'NONE',  ( -12.28060600210000075, -0.5788309733769999577, 232.6627643349999914 ) ) ;
#9544 = CARTESIAN_POINT ( 'NONE',  ( -4.175165894169885483, -119.7166638525666826, -63.39999999999999858 ) ) ;
#9545 = CARTESIAN_POINT ( 'NONE',  ( 19.80526555972147307, 19.50877392102524155, 3.000000000000002665 ) ) ;
#9546 = CARTESIAN_POINT ( 'NONE',  ( -5.023648568049999596, -17.12171681569999748, 230.7531949689999919 ) ) ;
#9547 = FACE_OUTER_BOUND ( 'NONE', #19408, .T. ) ;
#9548 = EDGE_CURVE ( 'NONE', #11502, #22798, #16815, .T. ) ;
#9549 = CARTESIAN_POINT ( 'NONE',  ( -24.97129468253034545, 13.73710443232325495, 3.901342130000013064 ) ) ;
#9550 = LINE ( 'NONE', #14432, #20650 ) ;
#9551 = CARTESIAN_POINT ( 'NONE',  ( -26.79999999999999361, -1.754055898257055324, 93.21714158836665831 ) ) ;
#9552 = LINE ( 'NONE', #21673, #21863 ) ;
#9553 = CARTESIAN_POINT ( 'NONE',  ( 7.097978820185624649, -115.1185614902606744, 21.95989595838153718 ) ) ;
#9554 = ORIENTED_EDGE ( 'NONE', *, *, #15634, .T. ) ;
#9555 = CARTESIAN_POINT ( 'NONE',  ( -1.100000000000000089, -27.47799119300000115, 225.0000000000000000 ) ) ;
#9556 = B_SPLINE_CURVE_WITH_KNOTS ( 'NONE', 5,
 ( #30075, #5382, #14990, #19871, #17491, #4108 ),
 .UNSPECIFIED., .F., .F.,
 ( 6, 6 ),
 ( 3.338999440259999840, 3.575680517940000414 ),
 .UNSPECIFIED. ) ;
#9557 = ORIENTED_EDGE ( 'NONE', *, *, #4842, .F. ) ;
#9558 = CARTESIAN_POINT ( 'NONE',  ( 24.60666743799999878, -12.93650359530000138, 225.1041818340000020 ) ) ;
#9559 = ADVANCED_FACE ( 'NONE', ( #23973 ), #21451, .T. ) ;
#9560 = CARTESIAN_POINT ( 'NONE',  ( -2.158984558600606007, 5.217364672555318883, -57.14652090042499566 ) ) ;
#9561 = ORIENTED_EDGE ( 'NONE', *, *, #1297, .F. ) ;
#9562 = ITEM_DEFINED_TRANSFORMATION ( 'NONE', 'NONE', #29902,  #17722 ) ;
#9563 = ORIENTED_EDGE ( 'NONE', *, *, #24459, .T. ) ;
#9564 = VECTOR ( 'NONE', #16030, 1000.000000000000114 ) ;
#9565 = DIRECTION ( 'NONE',  ( 0.000000000000000000, 1.000000000000000000, 0.000000000000000000 ) ) ;
#9566 = ORIENTED_EDGE ( 'NONE', *, *, #11639, .F. ) ;
#9567 = CARTESIAN_POINT ( 'NONE',  ( 23.40936070919999779, 16.84772962260000284, 229.0000000000000000 ) ) ;
#9568 = ADVANCED_FACE ( 'NONE', ( #2411 ), #14681, .F. ) ;
#9569 = DIRECTION ( 'NONE',  ( 1.000000000000000000, -1.224606353819999582E-16, 0.000000000000000000 ) ) ;
#9570 = CARTESIAN_POINT ( 'NONE',  ( -17.62526623054365871, -8.236462051082252600, 0.000000000000000000 ) ) ;
#9571 = B_SPLINE_CURVE_WITH_KNOTS ( 'NONE', 3,
 ( #23240, #11120, #14107, #25448, #11587, #18357 ),
 .UNSPECIFIED., .F., .F.,
 ( 4, 2, 4 ),
 ( 0.000000000000000000, 0.5000000000000000000, 1.000000000000000000 ),
 .UNSPECIFIED. ) ;
#9572 = CARTESIAN_POINT ( 'NONE',  ( 8.417769050959998722, 8.647000318390000828, 231.9999991140000191 ) ) ;
#9573 = CARTESIAN_POINT ( 'NONE',  ( 27.79539923781684507, 0.5057481689249165857, 1.000000000000000888 ) ) ;
#9574 = DIRECTION ( 'NONE',  ( 3.134067079931429195E-12, 0.3568421334038983650, -0.9341647027306021478 ) ) ;
#9575 = CARTESIAN_POINT ( 'NONE',  ( -1.425537026491585868, 4.583202318768851313, -3.837455258300006555 ) ) ;
#9576 = CARTESIAN_POINT ( 'NONE',  ( 25.19810601000000361, -14.44114490489999980, 230.5592437530000041 ) ) ;
#9577 = VERTEX_POINT ( 'NONE', #26631 ) ;
#9578 = CARTESIAN_POINT ( 'NONE',  ( -9.999999999969999109, -120.5233595632000174, -31.26042064989999858 ) ) ;
#9579 = AXIS2_PLACEMENT_3D ( 'NONE', #14605, #28914, #12227 ) ;
#9580 = CARTESIAN_POINT ( 'NONE',  ( 1.771049722044198971, -6.234229536879996481, -21.29535708919999593 ) ) ;
#9581 = CARTESIAN_POINT ( 'NONE',  ( 0.3874847876386515733, 3.500000000000000000, 230.8270369382009051 ) ) ;
#9582 = CARTESIAN_POINT ( 'NONE',  ( -10.00134423289999930, -25.00000000000000000, -2.314486209600001398 ) ) ;
#9583 = CARTESIAN_POINT ( 'NONE',  ( 1.064429457989999994, 12.07977735470000091, 230.6412452697800006 ) ) ;
#9584 = CARTESIAN_POINT ( 'NONE',  ( 0.000000000000000000, -17.25771824150000100, 225.0000000000000000 ) ) ;
#9585 = CARTESIAN_POINT ( 'NONE',  ( -20.25360395112956269, 20.00000005254026192, 0.6180758210000136810 ) ) ;
#9586 = LINE ( 'NONE', #26269, #23804 ) ;
#9587 = DIRECTION ( 'NONE',  ( 0.000000000000000000, 0.000000000000000000, -1.000000000000000000 ) ) ;
#9588 = DIRECTION ( 'NONE',  ( -0.7071067811865475727, 1.595945597898661921E-12, 0.7071067811865475727 ) ) ;
#9589 = EDGE_CURVE ( 'NONE', #23628, #20876, #4061, .T. ) ;
#9590 = CARTESIAN_POINT ( 'NONE',  ( -26.79999999999999361, 3.901323708532900174E-14, 37.32841481368520675 ) ) ;
#9591 = ORIENTED_EDGE ( 'NONE', *, *, #10857, .F. ) ;
#9592 = CARTESIAN_POINT ( 'NONE',  ( -17.66983789954736750, -8.284439791107988782, 0.000000000000000000 ) ) ;
#9593 = CARTESIAN_POINT ( 'NONE',  ( -380005.9281980000087, -207598.1847299999790, -249768.1509097300004 ) ) ;
#9594 = DIRECTION ( 'NONE',  ( 0.8775825618903718706, -0.4794255386042047262, 0.000000000000000000 ) ) ;
#9595 = ORIENTED_EDGE ( 'NONE', *, *, #27014, .F. ) ;
#9596 = CARTESIAN_POINT ( 'NONE',  ( 24.97129468909112404, -13.73710443560444183, 3.901342130000013064 ) ) ;
#9597 = CARTESIAN_POINT ( 'NONE',  ( -1.760169390438194759, -5.172221906152406845, -47.79520033292500614 ) ) ;
#9598 = ORIENTED_EDGE ( 'NONE', *, *, #1596, .T. ) ;
#9599 = ORIENTED_EDGE ( 'NONE', *, *, #28493, .F. ) ;
#9600 = AXIS2_PLACEMENT_3D ( 'NONE', #5128, #16623, #2011 ) ;
#9601 = EDGE_LOOP ( 'NONE', ( #3468, #26808, #522, #11651, #7811 ) ) ;
#9602 = CARTESIAN_POINT ( 'NONE',  ( 10.70000000009999930, -23.82317073084000114, -28.39999999989999324 ) ) ;
#9603 = EDGE_LOOP ( 'NONE', ( #20311, #9124, #1361, #9716 ) ) ;
#9604 = CARTESIAN_POINT ( 'NONE',  ( -9.000000000000000000, -130.0000000000000000, -43.39999999999999858 ) ) ;
#9605 = DIRECTION ( 'NONE',  ( 1.000000000000000000, -3.981000000000000101E-12, 1.940999999999999908E-12 ) ) ;
#9606 = EDGE_CURVE ( 'NONE', #4699, #4261, #18327, .T. ) ;
#9607 = DIRECTION ( 'NONE',  ( 0.7071067811870024311, 0.6455034180679679601, -0.2886612846606330662 ) ) ;
#9608 = CARTESIAN_POINT ( 'NONE',  ( 0.7946872764172051573, 4.107354228457116285, -35.69999999999999574 ) ) ;
#9609 = CARTESIAN_POINT ( 'NONE',  ( 18.39548692765703208, 20.00005474883426970, -0.6591334621046254227 ) ) ;
#9610 = CARTESIAN_POINT ( 'NONE',  ( -24.52721838146529620, 14.51532614515499020, 5.760265123000013254 ) ) ;
#9611 = CARTESIAN_POINT ( 'NONE',  ( -16.83342759579999637, -9.000000000000001776, -0.8000000000000020428 ) ) ;
#9612 = CARTESIAN_POINT ( 'NONE',  ( -19.29867024690000221, 19.63492390480000083, 229.6953880050000123 ) ) ;
#9613 = ORIENTED_EDGE ( 'NONE', *, *, #6230, .F. ) ;
#9614 = CARTESIAN_POINT ( 'NONE',  ( -4.184186767956290964, -1.312611723764788296, -10.52323088900000414 ) ) ;
#9615 = CARTESIAN_POINT ( 'NONE',  ( -5.430430790592723156, -2.746024268427175841, -27.36472909260000108 ) ) ;
#9616 = CARTESIAN_POINT ( 'NONE',  ( 3.221827467136498591, 1.415571281914143720, 0.000000000000000000 ) ) ;
#9617 = LINE ( 'NONE', #12744, #2147 ) ;
#9618 = ADVANCED_FACE ( 'NONE', ( #2562 ), #19555, .F. ) ;
#9619 = CARTESIAN_POINT ( 'NONE',  ( 24.47278418934494937, 14.60601539438439822, 6.095965388000001539 ) ) ;
#9620 = CARTESIAN_POINT ( 'NONE',  ( -3.950034095761355335, 2.484763540022569384, -10.44547590280000371 ) ) ;
#9621 = EDGE_CURVE ( 'NONE', #17104, #23118, #12149, .T. ) ;
#9622 = DIRECTION ( 'NONE',  ( 0.000000000000000000, 0.000000000000000000, -1.000000000000000000 ) ) ;
#9623 = CARTESIAN_POINT ( 'NONE',  ( -24.45473033751197178, -14.63622298155413226, 3.901342939999996595 ) ) ;
#9624 = CARTESIAN_POINT ( 'NONE',  ( -1.380865576384323168, -3.499743769985608211, 230.6852868990059164 ) ) ;
#9625 = ORIENTED_EDGE ( 'NONE', *, *, #13427, .F. ) ;
#9626 = EDGE_CURVE ( 'NONE', #23873, #26210, #29180, .T. ) ;
#9627 = FACE_OUTER_BOUND ( 'NONE', #3157, .T. ) ;
#9628 = CARTESIAN_POINT ( 'NONE',  ( 17.00259495291042455, 12.09719844080319895, -4.336808689942018722E-16 ) ) ;
#9629 = B_SPLINE_CURVE_WITH_KNOTS ( 'NONE', 5,
 ( #29920, #27704, #18103, #27554, #12930, #22227, #25199, #1291, #986, #14992, #24589, #5998, #27250, #15593, #681 ),
 .UNSPECIFIED., .F., .F.,
 ( 6, 3, 3, 3, 6 ),
 ( 0.000000000000000000, 0.1000000000034356601, 0.4000000000022904678, 0.7000000000005727196, 1.000000000000000000 ),
 .UNSPECIFIED. ) ;
#9630 = ORIENTED_EDGE ( 'NONE', *, *, #2965, .T. ) ;
#9631 = LINE ( 'NONE', #4455, #27394 ) ;
#9632 = CARTESIAN_POINT ( 'NONE',  ( 13.15526517074354196, 21.70000000000177209, -56.37750224591909642 ) ) ;
#9633 = ORIENTED_EDGE ( 'NONE', *, *, #26033, .T. ) ;
#9634 = EDGE_LOOP ( 'NONE', ( #13942, #14217, #27386, #19190 ) ) ;
#9635 = ORIENTED_EDGE ( 'NONE', *, *, #17759, .T. ) ;
#9636 = ORIENTED_EDGE ( 'NONE', *, *, #8864, .F. ) ;
#9637 = CARTESIAN_POINT ( 'NONE',  ( 0.000000000000000000, 19.99999999999999645, -44.10000000000000142 ) ) ;
#9638 = EDGE_CURVE ( 'NONE', #23803, #23190, #2865, .T. ) ;
#9639 = CARTESIAN_POINT ( 'NONE',  ( -8.699999999655181782, -13.66682223737418944, -36.55330428419230060 ) ) ;
#9640 = FACE_BOUND ( 'NONE', #19323, .T. ) ;
#9641 = ORIENTED_EDGE ( 'NONE', *, *, #9500, .T. ) ;
#9642 = DIRECTION ( 'NONE',  ( -0.0001253086065159677936, 0.000000000000000000, -0.9999999921488764709 ) ) ;
#9643 = VECTOR ( 'NONE', #1693, 1000.000000000000000 ) ;
#9644 = CARTESIAN_POINT ( 'NONE',  ( 6.000000000000000000, -29.27600094726834712, -81.66227801707495360 ) ) ;
#9645 = CARTESIAN_POINT ( 'NONE',  ( -17.27724273263302379, -31.99964310593069072, -30.37245333090922728 ) ) ;
#9646 = DIRECTION ( 'NONE',  ( -0.9831920802501790124, 0.1715636151751586680, 0.06244404920691486172 ) ) ;
#9647 = CARTESIAN_POINT ( 'NONE',  ( 2.926699082014111664, -4.037750131915458063, -0.6999994991842533043 ) ) ;
#9648 = ORIENTED_EDGE ( 'NONE', *, *, #14035, .T. ) ;
#9649 = EDGE_CURVE ( 'NONE', #26486, #14200, #7283, .T. ) ;
#9650 = CARTESIAN_POINT ( 'NONE',  ( -17.91543966611209981, 20.00000000001002221, -0.6999999999999785283 ) ) ;
#9651 = CARTESIAN_POINT ( 'NONE',  ( 0.5300456733980305479, -4.293941145674102344, -17.87054674910000784 ) ) ;
#9652 = CARTESIAN_POINT ( 'NONE',  ( -7.999999999652283478, -16.96959321758620476, -37.81493174591201978 ) ) ;
#9653 = CARTESIAN_POINT ( 'NONE',  ( 7.105427357599999217E-15, 0.000000000000000000, 136.3944487250000179 ) ) ;
#9654 = ORIENTED_EDGE ( 'NONE', *, *, #25278, .T. ) ;
#9655 = CARTESIAN_POINT ( 'NONE',  ( 16.10061776519356869, 10.69263420686418442, -0.6999999999999784173 ) ) ;
#9656 = CARTESIAN_POINT ( 'NONE',  ( 27.54633501930000250, 4.750421692669999807, 222.0000000000000000 ) ) ;
#9657 = CARTESIAN_POINT ( 'NONE',  ( 28.41645191122389846, 4.850979895915015661, 1.000000000000000888 ) ) ;
#9658 = FACE_OUTER_BOUND ( 'NONE', #7664, .T. ) ;
#9659 = CARTESIAN_POINT ( 'NONE',  ( 2.220446049249999755E-16, 2.100000000000000089, 226.6412452697800006 ) ) ;
#9660 = PRESENTATION_LAYER_ASSIGNMENT (  '', '', ( #23328 ) ) ;
#9661 = CARTESIAN_POINT ( 'NONE',  ( 27.79999999999999716, -2.352589991099999975E-11, 229.1414213560000235 ) ) ;
#9662 = CARTESIAN_POINT ( 'NONE',  ( -16.58808965729999940, -7.862989603470000866, 230.6999999999999886 ) ) ;
#9663 = ORIENTED_EDGE ( 'NONE', *, *, #13520, .T. ) ;
#9664 = AXIS2_PLACEMENT_3D ( 'NONE', #1100, #27378, #8633 ) ;
#9665 = CARTESIAN_POINT ( 'NONE',  ( 27.79999999980000069, 4.333901714429999608, 229.0000000000000000 ) ) ;
#9666 = CARTESIAN_POINT ( 'NONE',  ( 27.92857142909999979, -3.420150602509999660E-15, 187.9396849849999853 ) ) ;
#9667 = CARTESIAN_POINT ( 'NONE',  ( -27.88265104574380260, 4.289521473631270787, 1.000000000000000888 ) ) ;
#9668 = CARTESIAN_POINT ( 'NONE',  ( -4.749401372790300613, -1.581986711674698842, -68.10000000002503384 ) ) ;
#9669 = ORIENTED_EDGE ( 'NONE', *, *, #23334, .T. ) ;
#9670 = CARTESIAN_POINT ( 'NONE',  ( 19.31629274950000408, 18.68265037930000005, 230.6999999999999886 ) ) ;
#9671 = ORIENTED_EDGE ( 'NONE', *, *, #15322, .F. ) ;
#9672 = PLANE ( 'NONE',  #28559 ) ;
#9673 = ADVANCED_FACE ( 'NONE', ( #9954 ), #31052, .T. ) ;
#9674 = CIRCLE ( 'NONE', #5646, 18.00000000000000000 ) ;
#9675 = CARTESIAN_POINT ( 'NONE',  ( -3.857468353316018117, 3.836780423039637178, -69.74322600342500778 ) ) ;
#9676 = ORIENTED_EDGE ( 'NONE', *, *, #13956, .F. ) ;
#9677 = CARTESIAN_POINT ( 'NONE',  ( -4.266767049786682087, -2.157590496602210806, -28.90222909260000250 ) ) ;
#9678 = CARTESIAN_POINT ( 'NONE',  ( 0.5184513693225726305, -28.49550581263314086, 6.099998581000020792 ) ) ;
#9679 = ADVANCED_FACE ( 'NONE', ( #29139 ), #15133, .T. ) ;
#9680 = EDGE_CURVE ( 'NONE', #170, #12548, #26968, .T. ) ;
#9681 = CARTESIAN_POINT ( 'NONE',  ( -4.050122923326508584, -2.059172231882750559, -62.36424626872499033 ) ) ;
#9682 = CARTESIAN_POINT ( 'NONE',  ( -24.34131725939277757, -12.79741914669601144, 4.782075047738786999 ) ) ;
#9683 = AXIS2_PLACEMENT_3D ( 'NONE', #12171, #19730, #12479 ) ;
#9684 = SURFACE_STYLE_USAGE ( .BOTH. , #26067 ) ;
#9685 = CARTESIAN_POINT ( 'NONE',  ( 9.999488386939999529, 19.99999999999999645, -42.44046182635000264 ) ) ;
#9686 = UNCERTAINTY_MEASURE_WITH_UNIT (LENGTH_MEASURE( 1.000000000000000082E-05 ), #23356, 'distance_accuracy_value', 'NONE');
#9687 = DIRECTION ( 'NONE',  ( 2.249415931299125355E-12, -0.9431856258987900699, -0.3322662713817151059 ) ) ;
#9688 = DIRECTION ( 'NONE',  ( 0.9595496299847263710, -0.2815395311429191305, 0.000000000000000000 ) ) ;
#9689 = ORIENTED_EDGE ( 'NONE', *, *, #14130, .F. ) ;
#9690 = CARTESIAN_POINT ( 'NONE',  ( 0.000000000000000000, 0.000000000000000000, 140.0000000000000000 ) ) ;
#9691 = CARTESIAN_POINT ( 'NONE',  ( -6.394884621839999216E-14, -26.80000000000000071, 226.0999999999999943 ) ) ;
#9692 = CARTESIAN_POINT ( 'NONE',  ( -12.24209934469999972, 1.548575594009999890, 232.6627643349999914 ) ) ;
#9693 = CARTESIAN_POINT ( 'NONE',  ( -15.73383125209597999, -9.054522205455617367, 0.000000000000000000 ) ) ;
#9694 = DIRECTION ( 'NONE',  ( 0.000000000000000000, -1.000000000000000000, 0.000000000000000000 ) ) ;
#9695 = CARTESIAN_POINT ( 'NONE',  ( -5.747616903875187866, -30.90662447469063778, -80.12742089939932555 ) ) ;
#9697 = B_SPLINE_CURVE_WITH_KNOTS ( 'NONE', 3,
 ( #15485, #3212, #22424, #868 ),
 .UNSPECIFIED., .F., .F.,
 ( 4, 4 ),
 ( 0.000000000000000000, 1.000000000000000000 ),
 .UNSPECIFIED. ) ;
#9696 = CARTESIAN_POINT ( 'NONE',  ( 24.49848005072939827, -13.14029679208924151, 224.3227009702077908 ) ) ;
#9698 = CARTESIAN_POINT ( 'NONE',  ( -1.100000000000000311, -26.77741585740000474, 225.0970590044875621 ) ) ;
#9699 = FACE_OUTER_BOUND ( 'NONE', #11530, .T. ) ;
#9700 = CARTESIAN_POINT ( 'NONE',  ( 2.000000000000000000, 0.2617993877991477425, 227.6412452701696054 ) ) ;
#9701 = B_SPLINE_CURVE_WITH_KNOTS ( 'NONE', 3,
 ( #24332, #585, #20219, #12670, #5291, #22438, #29811, #883, #14734, #5436, #22125, #10166, #22595, #24486, #24945, #5587, #19610, #1035, #17687, #17845, #29665, #7639, #19766, #24639, #14894, #2923, #26841, #7943, #5124, #431, #3072, #22277, #29351, #12516, #7793, #735, #17394, #26997, #10326, #12835, #19920, #10013, #15046, #8094, #29507, #15347, #8247, #17543, #27153, #10478, #10624, #15188, #24792 ),
 .UNSPECIFIED., .F., .F.,
 ( 4, 1, 1, 1, 2, 2, 1, 1, 1, 1, 2, 2, 1, 1, 2, 2, 1, 1, 1, 2, 2, 1, 1, 1, 2, 2, 1, 1, 2, 2, 2, 2, 2, 2, 4 ),
 ( 0.000000000000000000, 0.01562499999999919509, 0.02343749999999868161, 0.02734374999999848038, 0.02929687499999846997, 0.03124999999999845957, 0.04687499999999945877, 0.05468749999999995837, 0.05859375000000026368, 0.06054687500000038858, 0.06152343750000032613, 0.06250000000000026368, 0.07812499999999922284, 0.08593749999999863998, 0.08984374999999845957, 0.09374999999999829303, 0.1093749999999974187, 0.1171874999999970440, 0.1210937499999970163, 0.1230468749999969330, 0.1249999999999968636, 0.1874999999999967248, 0.2187499999999966138, 0.2343749999999964750, 0.2421874999999965306, 0.2499999999999966138, 0.3749999999999971134, 0.4374999999999973355, 0.4687499999999975020, 0.4999999999999976685, 0.5624999999999980016, 0.6249999999999982236, 0.7499999999999987788, 0.8749999999999993339, 1.000000000000000000 ),
 .UNSPECIFIED. ) ;
#9702 = CARTESIAN_POINT ( 'NONE',  ( -6.050735318990731137, -17.25475041001947574, -75.15854509790392513 ) ) ;
#9703 = DIRECTION ( 'NONE',  ( 1.000000000000000000, 0.000000000000000000, 0.000000000000000000 ) ) ;
#9704 = CARTESIAN_POINT ( 'NONE',  ( 24.41841038956698640, 14.69667349781389376, 6.099998581000020792 ) ) ;
#9705 = VECTOR ( 'NONE', #20416, 1000.000000000000114 ) ;
#9706 = ORIENTED_EDGE ( 'NONE', *, *, #17557, .T. ) ;
#9707 = LINE ( 'NONE', #4841, #25841 ) ;
#9708 = VERTEX_POINT ( 'NONE', #5838 ) ;
#9709 = CARTESIAN_POINT ( 'NONE',  ( 1.814857447021396585E-10, -110.9401521129946389, -1.050525799519145487 ) ) ;
#9710 = CARTESIAN_POINT ( 'NONE',  ( -2.948077164825084306, -3.495793300896363753, -59.17407541852499975 ) ) ;
#9711 = VERTEX_POINT ( 'NONE', #24894 ) ;
#9712 = EDGE_CURVE ( 'NONE', #31042, #2824, #16482, .T. ) ;
#9713 = EDGE_LOOP ( 'NONE', ( #5064, #6273, #25106, #4418 ) ) ;
#9714 = CARTESIAN_POINT ( 'NONE',  ( 8.700000000234501485, -26.52350767672318810, -25.41191590392901034 ) ) ;
#9715 = EDGE_CURVE ( 'NONE', #5647, #15181, #22536, .T. ) ;
#9716 = ORIENTED_EDGE ( 'NONE', *, *, #18462, .T. ) ;
#9717 = FILL_AREA_STYLE ('',( #24507 ) ) ;
#9718 = CIRCLE ( 'NONE', #12749, 3.000000000000001332 ) ;
#9719 = CARTESIAN_POINT ( 'NONE',  ( 12.41901213044714680, 20.99999999997343636, -55.86814804320044914 ) ) ;
#9720 = MECHANICAL_DESIGN_GEOMETRIC_PRESENTATION_REPRESENTATION (  '', ( #19275 ), #4203 ) ;
#9721 = CARTESIAN_POINT ( 'NONE',  ( 3.441895620960000013, 11.73074934140000103, 232.6627648150000027 ) ) ;
#9722 = DIRECTION ( 'NONE',  ( -1.000000000000000000, 5.665498452320000818E-16, 0.000000000000000000 ) ) ;
#9723 = CARTESIAN_POINT ( 'NONE',  ( 5.763395275750641922, -2.111988417859953504, -5.836105321700000736 ) ) ;
#9724 = CARTESIAN_POINT ( 'NONE',  ( 4.175165894169885483, -55.00000000000000000, -44.10000000000000142 ) ) ;
#9725 = B_SPLINE_CURVE_WITH_KNOTS ( 'NONE', 3,
 ( #17125, #5164, #7225, #28937, #24528, #12097, #2968, #17278, #26579, #474, #14774, #5019, #19184, #24376 ),
 .UNSPECIFIED., .F., .F.,
 ( 4, 2, 2, 2, 2, 2, 4 ),
 ( 0.000000000000000000, 0.2499999999999525935, 0.3749999999999519273, 0.4374999999999515943, 0.4999999999999513722, 0.7499999999999755751, 1.000000000000000000 ),
 .UNSPECIFIED. ) ;
#9726 = EDGE_LOOP ( 'NONE', ( #9950, #20742, #18604, #17101, #3992, #7519, #3431, #5825 ) ) ;
#9727 = CARTESIAN_POINT ( 'NONE',  ( -0.6393421544539239498, -5.029762131177996309, -44.10000000002499121 ) ) ;
#9728 = CARTESIAN_POINT ( 'NONE',  ( 4.129834804009608007, 5.047645050193429128, -20.85622222230000489 ) ) ;
#9729 = CARTESIAN_POINT ( 'NONE',  ( 0.8585117870366192339, 3.500000000000000000, 230.7766559207250339 ) ) ;
#9730 = DIRECTION ( 'NONE',  ( 1.000000000000000000, 0.000000000000000000, -2.257150022439999944E-12 ) ) ;
#9731 = CARTESIAN_POINT ( 'NONE',  ( -24.60699806910000120, -12.93667933180000063, 225.0000014190000002 ) ) ;
#9732 = CARTESIAN_POINT ( 'NONE',  ( 27.63177371719999798, -3.383804566139999704E-15, 192.6394760450000092 ) ) ;
#9733 = CARTESIAN_POINT ( 'NONE',  ( -17.83930458829795640, 19.99999999999961631, 0.000000000000000000 ) ) ;
#9734 = CARTESIAN_POINT ( 'NONE',  ( 10.69999999999827622, -26.63513617188653626, -25.40000000000000213 ) ) ;
#9735 = CARTESIAN_POINT ( 'NONE',  ( 8.000000000829070146, -18.03083188300961481, -34.06405199645556792 ) ) ;
#9736 = CARTESIAN_POINT ( 'NONE',  ( 13.99999999979999821, 21.69999999929999390, -58.51619795559999915 ) ) ;
#9737 = VECTOR ( 'NONE', #582, 1000.000000000000000 ) ;
#9738 = VECTOR ( 'NONE', #8771, 1000.000000000000000 ) ;
#9740 = EDGE_CURVE ( 'NONE', #4471, #6349, #19442, .T. ) ;
#9739 = CIRCLE ( 'NONE', #27327, 1.700000000000000178 ) ;
#9741 = DIRECTION ( 'NONE',  ( 0.000000000000000000, -1.000000000000000000, 0.000000000000000000 ) ) ;
#9742 = EDGE_LOOP ( 'NONE', ( #30921, #10005, #10185, #4213 ) ) ;
#9743 = VECTOR ( 'NONE', #19929, 1000.000000000000000 ) ;
#9744 = VECTOR ( 'NONE', #25158, 1000.000000000000000 ) ;
#9745 = CARTESIAN_POINT ( 'NONE',  ( 1.844957972340690588, -5.198917526286033208, -31.25632401680000783 ) ) ;
#9746 = CARTESIAN_POINT ( 'NONE',  ( 1.346291201779999946, -3.434453875705480108, -72.25672407562892374 ) ) ;
#9747 = VERTEX_POINT ( 'NONE', #7882 ) ;
#9748 = CARTESIAN_POINT ( 'NONE',  ( 24.83827472153076599, -12.48687851163286133, 4.999998581000003384 ) ) ;
#9749 = CARTESIAN_POINT ( 'NONE',  ( 4.531630834892032667, -0.6723478992683162847, -46.13818262062499542 ) ) ;
#9750 = ORIENTED_EDGE ( 'NONE', *, *, #11880, .F. ) ;
#9751 = ORIENTED_EDGE ( 'NONE', *, *, #8593, .F. ) ;
#9752 = DIRECTION ( 'NONE',  ( 1.000000000000000000, 0.000000000000000000, 0.000000000000000000 ) ) ;
#9753 = B_SPLINE_SURFACE_WITH_KNOTS ( 'NONE', 5, 1, ( 
 ( #6550, #13952 ),
 ( #8908, #23565 ),
 ( #27956, #2000 ),
 ( #28580, #7020 ),
 ( #1532, #11590 ),
 ( #6396, #18509 ),
 ( #4192, #28420 ),
 ( #25762, #21038 ),
 ( #16147, #30639 ),
 ( #4039, #3883 ),
 ( #15996, #21186 ),
 ( #28111, #4511 ),
 ( #13474, #30486 ),
 ( #13637, #13794 ),
 ( #1839, #1683 ) ),
 .UNSPECIFIED., .F., .F., .F.,
 ( 6, 3, 3, 3, 6 ),
 ( 2, 2 ),
 ( 0.000000000000000000, 0.5239017171269999551, 1.047803434249999999, 1.571705151379999998, 1.746339057089999924 ),
 ( -0.7000000000009999335, 2.556331299420000144E-06 ),
 .UNSPECIFIED. ) ;
#9754 = ORIENTED_EDGE ( 'NONE', *, *, #17382, .F. ) ;
#9755 = CARTESIAN_POINT ( 'NONE',  ( 8.699999999994835420, -111.9817663798902885, 5.760339591779549018 ) ) ;
#9756 = ORIENTED_EDGE ( 'NONE', *, *, #19824, .T. ) ;
#9757 = CARTESIAN_POINT ( 'NONE',  ( -27.79539923781770483, -0.5057481688778011630, 1.000000000000000888 ) ) ;
#9758 = CARTESIAN_POINT ( 'NONE',  ( 2.407487872917116967, 2.830108685495575926, 227.7614631413372308 ) ) ;
#9759 = CARTESIAN_POINT ( 'NONE',  ( 10.69999999999999929, -27.00000000000000000, -28.40000000000000213 ) ) ;
#9760 = CARTESIAN_POINT ( 'NONE',  ( 0.2104509476007864199, 4.444330529862462242, -35.69999999999998863 ) ) ;
#9761 = B_SPLINE_CURVE_WITH_KNOTS ( 'NONE', 4,
 ( #17910, #15557, #25167, #11324, #18395 ),
 .UNSPECIFIED., .F., .F.,
 ( 5, 5 ),
 ( -0.9817477042469999748, 0.9817477042469999748 ),
 .UNSPECIFIED. ) ;
#9762 = CARTESIAN_POINT ( 'NONE',  ( 20.22062173471788071, 19.99992278450133298, 0.4812210343388954037 ) ) ;
#9763 = CARTESIAN_POINT ( 'NONE',  ( -23.88992818679365371, 14.21747995069046588, 5.680829343999993952 ) ) ;
#9764 = DIRECTION ( 'NONE',  ( -0.8775825618903718706, 0.4794255386042047262, 0.000000000000000000 ) ) ;
#9765 = AXIS2_PLACEMENT_3D ( 'NONE', #26964, #15009, #7456 ) ;
#9766 = CARTESIAN_POINT ( 'NONE',  ( -23.62948527985757963, -14.64611956755585709, 224.3223991483396560 ) ) ;
#9767 = CONICAL_SURFACE ( 'NONE', #17283, 1.656072167390155281, 0.3728633601815770082 ) ;
#9768 = ORIENTED_EDGE ( 'NONE', *, *, #20716, .T. ) ;
#9769 = VECTOR ( 'NONE', #20978, 1000.000000000000114 ) ;
#9770 = AXIS2_PLACEMENT_3D ( 'NONE', #7145, #4796, #7304 ) ;
#9771 = CARTESIAN_POINT ( 'NONE',  ( 0.2392016894930265591, 6.101552847015987879, -8.537690181100003883 ) ) ;
#9772 = CARTESIAN_POINT ( 'NONE',  ( -6.085238278930475531, -0.01014600953121863602, -28.16856466009999593 ) ) ;
#9773 = AXIS2_PLACEMENT_3D ( 'NONE', #30325, #15852, #8432 ) ;
#9774 = CARTESIAN_POINT ( 'NONE',  ( 1.776356839399999804E-15, -5.329070518200000398E-15, 224.6412452697800290 ) ) ;
#9775 = B_SPLINE_CURVE_WITH_KNOTS ( 'NONE', 3,
 ( #11238, #23206, #24935, #25413 ),
 .UNSPECIFIED., .F., .F.,
 ( 4, 4 ),
 ( -0.08350576075630000705, 0.08350576075630000705 ),
 .UNSPECIFIED. ) ;
#9776 = CARTESIAN_POINT ( 'NONE',  ( -16.85343921394901301, 12.09981795542885585, -0.6999999989999727834 ) ) ;
#9777 = B_SPLINE_CURVE_WITH_KNOTS ( 'NONE', 3,
 ( #27400, #5685, #19870, #15442, #10572, #17788 ),
 .UNSPECIFIED., .F., .F.,
 ( 4, 2, 4 ),
 ( 0.000000000000000000, 0.5000000000000000000, 1.000000000000000000 ),
 .UNSPECIFIED. ) ;
#9778 = CARTESIAN_POINT ( 'NONE',  ( 20.30396079673062815, 19.99999999994985700, 0.8743359189999910797 ) ) ;
#9779 = CARTESIAN_POINT ( 'NONE',  ( -25.46368746804859740, 12.80129684245613575, 4.999998581000003384 ) ) ;
#9780 = CARTESIAN_POINT ( 'NONE',  ( 7.379546049855187029, -26.49401563815924376, 21.93856359977218418 ) ) ;
#9781 = CARTESIAN_POINT ( 'NONE',  ( 4.630235822890134578, 0.3309221515414850767, -14.64454535870000207 ) ) ;
#9782 = ADVANCED_FACE ( 'NONE', ( #529 ), #28260, .F. ) ;
#9783 = CARTESIAN_POINT ( 'NONE',  ( 0.6090474298383116158, -27.79358669172298946, 6.095948809000023338 ) ) ;
#9784 = CARTESIAN_POINT ( 'NONE',  ( 8.000000000235820252, -29.73863906515999389, -27.17531388883937993 ) ) ;
#9785 = CARTESIAN_POINT ( 'NONE',  ( -0.1113126277073503700, 2.989789856892466346, -42.27519293827315749 ) ) ;
#9786 = ORIENTED_EDGE ( 'NONE', *, *, #7319, .T. ) ;
#9787 =( GEOMETRIC_REPRESENTATION_CONTEXT ( 3 ) GLOBAL_UNCERTAINTY_ASSIGNED_CONTEXT ( ( #16610 ) ) GLOBAL_UNIT_ASSIGNED_CONTEXT ( ( #5103, #24153, #14872 ) ) REPRESENTATION_CONTEXT ( 'NONE', 'WORKASPACE' ) );
#9788 = ADVANCED_FACE ( 'NONE', ( #13546 ), #1755, .F. ) ;
#9789 = CARTESIAN_POINT ( 'NONE',  ( 16.47468026047738121, 11.86718987800275471, -4.336808689942017736E-16 ) ) ;
#9790 = ORIENTED_EDGE ( 'NONE', *, *, #12733, .T. ) ;
#9791 = B_SPLINE_SURFACE_WITH_KNOTS ( 'NONE', 5, 1, ( 
 ( #24448, #2883 ),
 ( #28844, #29306 ),
 ( #26959, #9656 ),
 ( #5545, #14696 ),
 ( #7751, #7302 ),
 ( #16890, #12020 ),
 ( #29005, #29155 ),
 ( #17047, #24139 ),
 ( #4937, #10283 ) ),
 .UNSPECIFIED., .F., .F., .F.,
 ( 6, 3, 6 ),
 ( 2, 2 ),
 ( 0.000000000000000000, 12.04143823630000121, 16.88247121709999732 ),
 ( -3.785313009420000493E-15, 0.7017044499210000064 ),
 .UNSPECIFIED. ) ;
#9792 = CARTESIAN_POINT ( 'NONE',  ( 24.73445225629999911, -14.15837998019999944, 226.0959682270000144 ) ) ;
#9793 = CARTESIAN_POINT ( 'NONE',  ( 24.21906834310036771, 15.02342240524378703, 3.957526369000014199 ) ) ;
#9794 = AXIS2_PLACEMENT_3D ( 'NONE', #1110, #29899, #8325 ) ;
#9795 = ORIENTED_EDGE ( 'NONE', *, *, #27996, .T. ) ;
#9796 = VERTEX_POINT ( 'NONE', #1599 ) ;
#9797 = VERTEX_POINT ( 'NONE', #11186 ) ;
#9798 = EDGE_LOOP ( 'NONE', ( #400, #28977, #21067, #20511 ) ) ;
#9799 = DIRECTION ( 'NONE',  ( -8.579942312181285869E-13, -0.9431856258987900699, -0.3322662713817151059 ) ) ;
#9800 = CARTESIAN_POINT ( 'NONE',  ( -21.16705332919999805, 21.30254446269999846, 229.0000000000000000 ) ) ;
#9801 = EDGE_CURVE ( 'NONE', #27907, #3989, #30309, .T. ) ;
#9802 = CARTESIAN_POINT ( 'NONE',  ( 18.03376228215428156, -8.308107856198580166, -4.336808689942017736E-16 ) ) ;
#9803 = ORIENTED_EDGE ( 'NONE', *, *, #29891, .F. ) ;
#9804 = CARTESIAN_POINT ( 'NONE',  ( -25.44662322720214576, 12.83524168061546966, 5.310645680000003921 ) ) ;
#9805 = DIRECTION ( 'NONE',  ( 1.000000000000000000, 0.000000000000000000, 0.000000000000000000 ) ) ;
#9806 = CARTESIAN_POINT ( 'NONE',  ( -13.12132034329999897, 20.99999999990000887, -69.22132034359999864 ) ) ;
#9807 = AXIS2_PLACEMENT_3D ( 'NONE', #27144, #3525, #22428 ) ;
#9808 = MECHANICAL_DESIGN_GEOMETRIC_PRESENTATION_REPRESENTATION (  '', ( #12814 ), #8782 ) ;
#9809 = CARTESIAN_POINT ( 'NONE',  ( 7.638687372266933728, -0.9159326020094504806, -37.03243899219256008 ) ) ;
#9810 = ORIENTED_EDGE ( 'NONE', *, *, #22721, .F. ) ;
#9811 = CARTESIAN_POINT ( 'NONE',  ( -17.83929479963776288, 19.99998902616253105, -0.6999999999999784173 ) ) ;
#9812 = CARTESIAN_POINT ( 'NONE',  ( 5.320018516182488000, -2.211191048809329374, -17.87122516810000405 ) ) ;
#9813 = CARTESIAN_POINT ( 'NONE',  ( -1.110223024630000146E-16, 0.000000000000000000, -43.39999999999999858 ) ) ;
#9814 = CARTESIAN_POINT ( 'NONE',  ( 27.50000000000000000, -3.367667472999999580E-15, 115.0000000010000036 ) ) ;
#9815 = CARTESIAN_POINT ( 'NONE',  ( 3.760007715734311251, -19.71206033701148996, -27.86495495698533986 ) ) ;
#9816 = DIRECTION ( 'NONE',  ( 1.000000000000000000, -0.000000000000000000, -2.257150022439999944E-12 ) ) ;
#9817 = AXIS2_PLACEMENT_3D ( 'NONE', #10708, #16055, #22671 ) ;
#9818 = CARTESIAN_POINT ( 'NONE',  ( 22.78981481966842182, -14.10205219082176065, 5.737227008641060166 ) ) ;
#9819 = CARTESIAN_POINT ( 'NONE',  ( 1.065814103639999922E-14, 0.000000000000000000, 36.78285841159999592 ) ) ;
#9820 = CARTESIAN_POINT ( 'NONE',  ( 3.040504021322313122, 1.733590290792417887, -0.6999999999999784173 ) ) ;
#9821 = EDGE_CURVE ( 'NONE', #27542, #17245, #25022, .T. ) ;
#9822 = DIRECTION ( 'NONE',  ( 1.000000000000000000, -1.224606353819999829E-16, 0.000000000000000000 ) ) ;
#9823 = DIRECTION ( 'NONE',  ( -0.9880370573969197157, 0.1542166437529879364, 0.000000000000000000 ) ) ;
#9824 = VERTEX_POINT ( 'NONE', #25982 ) ;
#9825 = CARTESIAN_POINT ( 'NONE',  ( -12.30489359501477864, -24.40455160664326684, -24.12498013687346443 ) ) ;
#9826 = ADVANCED_FACE ( 'NONE', ( #20944, #20787 ), #6462, .T. ) ;
#9827 = DIRECTION ( 'NONE',  ( 0.1542166437529880196, 0.9880370573969197157, 0.000000000000000000 ) ) ;
#9828 = CARTESIAN_POINT ( 'NONE',  ( -4.873443905621923200, -0.09218704096741060783, -68.10000000002501963 ) ) ;
#9829 = AXIS2_PLACEMENT_3D ( 'NONE', #7085, #14338, #9439 ) ;
#9830 = ORIENTED_EDGE ( 'NONE', *, *, #24259, .T. ) ;
#9831 = CARTESIAN_POINT ( 'NONE',  ( 3.542914729026319876, 0.003443490030938245461, -88.52261276241732446 ) ) ;
#9832 =( NAMED_UNIT ( * ) PLANE_ANGLE_UNIT ( ) SI_UNIT ( $, .RADIAN. ) );
#9833 = VERTEX_POINT ( 'NONE', #8657 ) ;
#9834 = DIRECTION ( 'NONE',  ( 0.3633921898465273803, -0.9316362575375355393, 0.000000000000000000 ) ) ;
#9835 = CARTESIAN_POINT ( 'NONE',  ( -0.8291470764733243071, -4.443337602648614215, -68.30745670422500382 ) ) ;
#9836 = EDGE_CURVE ( 'NONE', #23146, #26338, #13705, .T. ) ;
#9837 = ORIENTED_EDGE ( 'NONE', *, *, #1167, .F. ) ;
#9838 = CARTESIAN_POINT ( 'NONE',  ( 3.790912472548403578, -2.108217834232220422, -26.93037294500000201 ) ) ;
#9839 = CARTESIAN_POINT ( 'NONE',  ( 24.49999999470000134, -3.000285566199999922E-15, 39.99999999930000172 ) ) ;
#9840 = EDGE_CURVE ( 'NONE', #22953, #15258, #11501, .T. ) ;
#9841 = CARTESIAN_POINT ( 'NONE',  ( -1.460566089872938900, -4.291843709425553044, -46.99520033292500187 ) ) ;
#9842 = PLANE ( 'NONE',  #27114 ) ;
#9843 = CARTESIAN_POINT ( 'NONE',  ( -7.999999999664561656, -9.529422221863875109, -35.87488938007345496 ) ) ;
#9844 = EDGE_CURVE ( 'NONE', #26590, #30960, #13980, .T. ) ;
#9845 = CARTESIAN_POINT ( 'NONE',  ( 8.700000000301640668, -14.95611408989196711, -40.37595097046296644 ) ) ;
#9846 = CARTESIAN_POINT ( 'NONE',  ( 11.49999999979999998, 20.99999999990000887, -70.09999999999999432 ) ) ;
#9847 = ORIENTED_EDGE ( 'NONE', *, *, #2240, .F. ) ;
#9848 = CARTESIAN_POINT ( 'NONE',  ( 14.84842474946407620, -32.00026250641055015, -28.62408860391630583 ) ) ;
#9849 = CARTESIAN_POINT ( 'NONE',  ( -24.36724936496760918, -13.38201651699120021, 5.104178996000019453 ) ) ;
#9850 = CARTESIAN_POINT ( 'NONE',  ( -23.39354070939840824, -15.01969650306709170, 5.760134161999996394 ) ) ;
#9851 = CARTESIAN_POINT ( 'NONE',  ( -27.79999999999999716, -2.360757793890000105E-11, 229.0000000000000000 ) ) ;
#9852 = CARTESIAN_POINT ( 'NONE',  ( 23.88690489929999927, -14.22221811490000043, 223.9575292099999899 ) ) ;
#9853 = CARTESIAN_POINT ( 'NONE',  ( 10.69999999998290008, -127.6903210698857549, -34.82346581440141620 ) ) ;
#9854 = DIRECTION ( 'NONE',  ( 0.000000000000000000, 0.000000000000000000, -1.000000000000000000 ) ) ;
#9855 = ADVANCED_FACE ( 'NONE', ( #10883 ), #4145, .T. ) ;
#9856 = CARTESIAN_POINT ( 'NONE',  ( -19.89993772616713841, -20.76973888581983019, -0.6577119969999878357 ) ) ;
#9857 = LINE ( 'NONE', #10168, #22810 ) ;
#9858 = CARTESIAN_POINT ( 'NONE',  ( 28.68577476838161644, -9.950727360109466346, 8.000000000000007105 ) ) ;
#9859 = CARTESIAN_POINT ( 'NONE',  ( 10.00000000000000000, -15.86465192213301556, -74.65259062561435144 ) ) ;
#9860 = ADVANCED_FACE ( 'NONE', ( #9441 ), #24087, .F. ) ;
#9861 = DIRECTION ( 'NONE',  ( 0.9316362575375356503, 0.3633921898465274913, 0.000000000000000000 ) ) ;
#9862 = CARTESIAN_POINT ( 'NONE',  ( 8.700000000244115128, -26.99999999999395328, -28.39999999994493862 ) ) ;
#9863 = CARTESIAN_POINT ( 'NONE',  ( 22.63992238019999803, -14.34133587289999845, 225.0000000000000000 ) ) ;
#9864 = ORIENTED_EDGE ( 'NONE', *, *, #17117, .F. ) ;
#9865 = EDGE_CURVE ( 'NONE', #16870, #28488, #5555, .T. ) ;
#9866 = CARTESIAN_POINT ( 'NONE',  ( -12.36097874953984466, 21.69999999999976836, -55.83956240900247536 ) ) ;
#9867 = CARTESIAN_POINT ( 'NONE',  ( -24.69967241520000201, -14.21967358789999913, 223.9000014189999774 ) ) ;
#9868 = VERTEX_POINT ( 'NONE', #9755 ) ;
#9869 = CARTESIAN_POINT ( 'NONE',  ( 24.26025373720000289, -13.57556515269999942, 226.0424756639999941 ) ) ;
#9870 = CARTESIAN_POINT ( 'NONE',  ( -1.650988191866312516, 3.989749455477759721, -57.54652090042499424 ) ) ;
#9871 = VERTEX_POINT ( 'NONE', #2221 ) ;
#9872 = ITEM_DEFINED_TRANSFORMATION ( 'NONE', 'NONE', #25903,  #17722 ) ;
#9873 = EDGE_LOOP ( 'NONE', ( #26169, #22381, #30435, #17975, #24972 ) ) ;
#9874 = CARTESIAN_POINT ( 'NONE',  ( 10.45000000009999930, -24.07317073171000033, -28.39999999989999679 ) ) ;
#9875 = ORIENTED_EDGE ( 'NONE', *, *, #4098, .F. ) ;
#9876 = ORIENTED_EDGE ( 'NONE', *, *, #10187, .T. ) ;
#9877 = CARTESIAN_POINT ( 'NONE',  ( 22.97596755210000197, 15.65128466780000061, 222.0000000000000000 ) ) ;
#9878 = CARTESIAN_POINT ( 'NONE',  ( -23.79228473957821777, 14.38012949749760416, 4.689353541000001790 ) ) ;
#9879 = CARTESIAN_POINT ( 'NONE',  ( -27.87609112763809449, 3.928995115440388375, 5.200000000000009948 ) ) ;
#9880 = B_SPLINE_SURFACE_WITH_KNOTS ( 'NONE', 5, 1, ( 
 ( #11594, #4357 ),
 ( #7337, #26529 ),
 ( #6860, #6707 ),
 ( #26385, #19139 ),
 ( #2314, #14581 ),
 ( #9371, #2156 ) ),
 .UNSPECIFIED., .F., .F., .F.,
 ( 6, 6 ),
 ( 2, 2 ),
 ( 0.000000000000000000, 7.118175366610000054 ),
 ( -0.7000000000080000007, 0.0003774914509440000041 ),
 .UNSPECIFIED. ) ;
#9881 = CARTESIAN_POINT ( 'NONE',  ( 7.637033006139999358, 9.343723945229999828, 231.9999991140000191 ) ) ;
#9882 = FACE_OUTER_BOUND ( 'NONE', #21612, .T. ) ;
#9883 = CARTESIAN_POINT ( 'NONE',  ( 0.2392016894930265591, 6.101552847015987879, -7.937690181100006903 ) ) ;
#9884 = FACE_OUTER_BOUND ( 'NONE', #24572, .T. ) ;
#9885 = ORIENTED_EDGE ( 'NONE', *, *, #9449, .F. ) ;
#9886 = CARTESIAN_POINT ( 'NONE',  ( 1.017907904351449844, -4.876997505310738390, -44.10000000002499831 ) ) ;
#9887 = CARTESIAN_POINT ( 'NONE',  ( 15.49562240950000103, -7.676231176589999983, 5.000000000000000000 ) ) ;
#9888 = CARTESIAN_POINT ( 'NONE',  ( -3.316315296248301792, 4.409923538414076027, -20.63064294429999990 ) ) ;
#9889 = LINE ( 'NONE', #148, #1608 ) ;
#9890 = CARTESIAN_POINT ( 'NONE',  ( -8.699999999700381181, -24.65270539047089926, -30.30942439802224442 ) ) ;
#9891 = ADVANCED_FACE ( 'NONE', ( #17139 ), #5035, .F. ) ;
#9892 = CARTESIAN_POINT ( 'NONE',  ( -2.525646774299999731, 11.92010449670000050, 230.6412452697800006 ) ) ;
#9893 = FACE_OUTER_BOUND ( 'NONE', #7918, .T. ) ;
#9894 = CARTESIAN_POINT ( 'NONE',  ( -1.677440080217387219, -4.586793301645948340, -43.23640794712499513 ) ) ;
#9895 = EDGE_CURVE ( 'NONE', #23549, #19698, #10965, .T. ) ;
#9896 = CARTESIAN_POINT ( 'NONE',  ( 3.760007715734309475, -21.02717377737872795, -30.56133709588283409 ) ) ;
#9897 = EDGE_CURVE ( 'NONE', #25829, #18513, #14340, .T. ) ;
#9898 = CARTESIAN_POINT ( 'NONE',  ( 8.000000000456484628, -17.29968381802795463, -33.37248524067440769 ) ) ;
#9899 = LINE ( 'NONE', #318, #16298 ) ;
#9900 = CARTESIAN_POINT ( 'NONE',  ( -18.50496050079999932, 20.74627092889999957, 229.1414212730000202 ) ) ;
#9901 = EDGE_CURVE ( 'NONE', #7727, #16212, #21524, .T. ) ;
#9902 = CARTESIAN_POINT ( 'NONE',  ( -1.505510951065242020, -9.645525760189025632, -102.7632020892250040 ) ) ;
#9903 = ORIENTED_EDGE ( 'NONE', *, *, #8409, .T. ) ;
#9904 = CARTESIAN_POINT ( 'NONE',  ( 2.499950477468915189, 3.566222500441431187, -29.71106724380000230 ) ) ;
#9905 = CARTESIAN_POINT ( 'NONE',  ( 9.999999999975235809, -125.3357287891403757, -32.69504109670850767 ) ) ;
#9906 = EDGE_LOOP ( 'NONE', ( #16697, #30884, #10641, #24962 ) ) ;
#9907 = CARTESIAN_POINT ( 'NONE',  ( 24.37450210455010335, -13.36961646745188759, 3.904029301000005781 ) ) ;
#9908 = CARTESIAN_POINT ( 'NONE',  ( -6.340437944841875506, 0.6332316896323284539, -48.10737393802499184 ) ) ;
#9909 = VERTEX_POINT ( 'NONE', #11962 ) ;
#9910 = ORIENTED_EDGE ( 'NONE', *, *, #22783, .T. ) ;
#9911 = VECTOR ( 'NONE', #9642, 1000.000000000000114 ) ;
#9912 = DIRECTION ( 'NONE',  ( 1.000000000000000000, 0.000000000000000000, 0.000000000000000000 ) ) ;
#9913 = EDGE_LOOP ( 'NONE', ( #12762, #485, #12185, #16601, #14704, #16447 ) ) ;
#9914 = CIRCLE ( 'NONE', #15954, 4.100000000000000533 ) ;
#9915 = CARTESIAN_POINT ( 'NONE',  ( -7.453090060300250563, -2.907137518772508589, 202.0000000000000000 ) ) ;
#9916 = ADVANCED_BREP_SHAPE_REPRESENTATION ( '', ( #941, #17722 ), #2296 ) ;
#9917 = VERTEX_POINT ( 'NONE', #9602 ) ;
#9918 = CARTESIAN_POINT ( 'NONE',  ( -27.66290831536099759, -7.787312998881454895, 1.000000000000000888 ) ) ;
#9919 = CARTESIAN_POINT ( 'NONE',  ( 2.595403069823767339, 2.504630016939114689, 227.7079405341281699 ) ) ;
#9920 = CARTESIAN_POINT ( 'NONE',  ( 8.699999999531884853, -22.83323352251082738, -39.84673050073825351 ) ) ;
#9921 = CARTESIAN_POINT ( 'NONE',  ( 0.3669718430465309100, 4.315306525164807283, -35.70000000000000995 ) ) ;
#9922 = B_SPLINE_CURVE_WITH_KNOTS ( 'NONE', 5,
 ( #21050, #8600, #3896, #16318, #25929, #22941, #4206, #30168, #6255 ),
 .UNSPECIFIED., .F., .F.,
 ( 6, 3, 6 ),
 ( 0.000000000000000000, 53.20205529499999386, 91.13698440880000362 ),
 .UNSPECIFIED. ) ;
#9923 = CARTESIAN_POINT ( 'NONE',  ( -12.40047914203026380, -30.61031961594332529, -24.71115946178905176 ) ) ;
#9924 = CARTESIAN_POINT ( 'NONE',  ( -24.93720648713954446, 13.79881813474513486, 6.099998581000020792 ) ) ;
#9925 = CARTESIAN_POINT ( 'NONE',  ( -22.92405521513462929, -13.88330634431700972, 5.957452580073338666 ) ) ;
#9926 = CARTESIAN_POINT ( 'NONE',  ( -17.83929479963776288, 19.99998902616253105, -0.6999999999999784173 ) ) ;
#9927 = CARTESIAN_POINT ( 'NONE',  ( 0.1879441846346346090, 4.794077236920960772, -8.875190181100002462 ) ) ;
#9928 = CARTESIAN_POINT ( 'NONE',  ( 5.097421258188004067, 0.5103876169533114737, -28.69366556700000004 ) ) ;
#9929 = CARTESIAN_POINT ( 'NONE',  ( -3.040504021322313122, -1.733590290792417887, 0.000000000000000000 ) ) ;
#9930 = CIRCLE ( 'NONE', #21994, 28.50000000000000000 ) ;
#9931 = CARTESIAN_POINT ( 'NONE',  ( 24.49145441566124148, -14.57548795709913847, 5.680829342999987652 ) ) ;
#9932 = CARTESIAN_POINT ( 'NONE',  ( 17.16657240420000008, 10.97998838177520931, -1.972246272986471594 ) ) ;
#9933 = FILL_AREA_STYLE_COLOUR ( '', #590 ) ;
#9934 = CARTESIAN_POINT ( 'NONE',  ( 6.336630981016743824, -26.76091511895456421, 21.17299964012854119 ) ) ;
#9935 = CARTESIAN_POINT ( 'NONE',  ( 2.992916622598568388, -2.824380467281232487, -18.03565260999999964 ) ) ;
#9936 = VECTOR ( 'NONE', #25271, 1000.000000000000000 ) ;
#9937 = CARTESIAN_POINT ( 'NONE',  ( -4.352394000759999624E-10, -4.352376237189999857E-10, 227.6412452697800006 ) ) ;
#9938 = CARTESIAN_POINT ( 'NONE',  ( -24.61381496313306982, -14.36755986783020056, 3.957524336000023624 ) ) ;
#9939 = CARTESIAN_POINT ( 'NONE',  ( 0.7992118187927096384, -3.499831230572010288, 230.7844944799418272 ) ) ;
#9940 = ORIENTED_EDGE ( 'NONE', *, *, #13004, .F. ) ;
#9941 = CYLINDRICAL_SURFACE ( 'NONE', #14292, 3.000000000000002220 ) ;
#9942 = CARTESIAN_POINT ( 'NONE',  ( -12.59531001298080710, -31.99999999999998579, -26.06220780008972326 ) ) ;
#9943 = VERTEX_POINT ( 'NONE', #6927 ) ;
#9944 = LINE ( 'NONE', #17777, #17335 ) ;
#9945 = LINE ( 'NONE', #24885, #24281 ) ;
#9946 = ORIENTED_EDGE ( 'NONE', *, *, #9283, .F. ) ;
#9947 = CARTESIAN_POINT ( 'NONE',  ( 9.414213562409999625, -15.31419272936388687, -74.45223986426802298 ) ) ;
#9948 = VERTEX_POINT ( 'NONE', #26137 ) ;
#9949 = B_SPLINE_SURFACE_WITH_KNOTS ( 'NONE', 5, 1, ( 
 ( #17239, #27454 ),
 ( #20079, #24489 ),
 ( #2928, #5896 ),
 ( #29669, #25107 ),
 ( #4336, #25432 ),
 ( #6214, #18167 ),
 ( #8883, #27936 ),
 ( #18488, #15974 ),
 ( #20697, #1349 ),
 ( #15653, #10786 ),
 ( #27770, #20384 ),
 ( #8726, #30135 ),
 ( #15823, #13615 ),
 ( #8566, #28086 ),
 ( #23220, #22744 ) ),
 .UNSPECIFIED., .F., .F., .F.,
 ( 6, 3, 3, 3, 6 ),
 ( 2, 2 ),
 ( 0.000000000000000000, 0.5239055193860000514, 1.047811038770000147, 1.571716558150000109, 1.746351731290000098 ),
 ( -0.7000000000009999335, 2.557300549769999790E-06 ),
 .UNSPECIFIED. ) ;
#9950 = ORIENTED_EDGE ( 'NONE', *, *, #15837, .F. ) ;
#9951 = AXIS2_PLACEMENT_3D ( 'NONE', #16339, #28451, #30668 ) ;
#9952 = APPLICATION_PROTOCOL_DEFINITION ( 'draft international standard', 'automotive_design', 1998, #26848 ) ;
#9953 = ORIENTED_EDGE ( 'NONE', *, *, #8522, .F. ) ;
#9954 = FACE_OUTER_BOUND ( 'NONE', #13613, .T. ) ;
#9955 = VECTOR ( 'NONE', #10147, 1000.000000000000000 ) ;
#9956 = LINE ( 'NONE', #25044, #6107 ) ;
#9957 = EDGE_CURVE ( 'NONE', #1677, #18573, #19201, .T. ) ;
#9958 = DIRECTION ( 'NONE',  ( 0.000000000000000000, 0.000000000000000000, 1.000000000000000000 ) ) ;
#9959 = ORIENTED_EDGE ( 'NONE', *, *, #1666, .F. ) ;
#9960 = DIRECTION ( 'NONE',  ( 0.000000000000000000, 0.000000000000000000, 1.000000000000000000 ) ) ;
#9961 = AXIS2_PLACEMENT_3D ( 'NONE', #10757, #3667, #29482 ) ;
#9962 = CARTESIAN_POINT ( 'NONE',  ( 16.20123158609999692, -8.472631907500000281, -0.7999999992999995424 ) ) ;
#9963 = CIRCLE ( 'NONE', #24029, 26.80000000000000071 ) ;
#9964 = CARTESIAN_POINT ( 'NONE',  ( 0.000000000000000000, 0.000000000000000000, 41.66046017469999896 ) ) ;
#9965 = LINE ( 'NONE', #7293, #5910 ) ;
#9966 = ORIENTED_EDGE ( 'NONE', *, *, #1620, .F. ) ;
#9967 = EDGE_CURVE ( 'NONE', #10105, #15932, #23185, .T. ) ;
#9968 = CARTESIAN_POINT ( 'NONE',  ( -4.598830142556993295, 1.338852748371190282, -15.36693125759999923 ) ) ;
#9969 = CARTESIAN_POINT ( 'NONE',  ( -27.79999999999999716, -2.360778239559999931E-11, 229.0000000000000000 ) ) ;
#9970 = DIRECTION ( 'NONE',  ( -0.7071067811865475727, 0.7071067811865475727, 0.000000000000000000 ) ) ;
#9971 = CARTESIAN_POINT ( 'NONE',  ( 4.494667250129237068, -18.71248644572223796, -28.35247971844670190 ) ) ;
#9972 = CARTESIAN_POINT ( 'NONE',  ( 11.78484171507088085, 21.69999999994148965, -70.02227941812002143 ) ) ;
#9973 = LINE ( 'NONE', #23993, #25364 ) ;
#9974 = AXIS2_PLACEMENT_3D ( 'NONE', #21342, #23711, #25915 ) ;
#9975 = DIRECTION ( 'NONE',  ( 0.8090169943751909232, 0.5877852522921378498, 0.000000000000000000 ) ) ;
#9976 = CARTESIAN_POINT ( 'NONE',  ( 27.92857142909999979, -3.420150602509999660E-15, 37.93968498519999599 ) ) ;
#9977 = CARTESIAN_POINT ( 'NONE',  ( 24.06257814289999786, 13.36313762839999875, 230.0000000000000000 ) ) ;
#9978 = DIRECTION ( 'NONE',  ( 0.000000000000000000, -1.000000000000000000, 0.000000000000000000 ) ) ;
#9979 = B_SPLINE_CURVE_WITH_KNOTS ( 'NONE', 5,
 ( #11878, #9519, #14402, #4491, #19116, #2747, #14093, #26659, #12342 ),
 .UNSPECIFIED., .F., .F.,
 ( 6, 3, 6 ),
 ( 0.000000000000000000, 2.405120303439999940, 3.339306056729999916 ),
 .UNSPECIFIED. ) ;
#9980 = ORIENTED_EDGE ( 'NONE', *, *, #186, .F. ) ;
#9981 = CARTESIAN_POINT ( 'NONE',  ( 0.9406167415608388538, 5.909121140422558760, -54.41500058692499664 ) ) ;
#9982 = DIRECTION ( 'NONE',  ( -1.000000000000000000, 1.380859481889999837E-13, -9.437625531729999712E-14 ) ) ;
#9983 = DIRECTION ( 'NONE',  ( 0.000000000000000000, 0.000000000000000000, 1.000000000000000000 ) ) ;
#9984 = AXIS2_PLACEMENT_3D ( 'NONE', #19017, #28620, #29075 ) ;
#9985 = CARTESIAN_POINT ( 'NONE',  ( -4.398480579787159783, -2.501424955541164508, -68.10000000002500542 ) ) ;
#9986 = ADVANCED_FACE ( 'NONE', ( #30147 ), #12422, .F. ) ;
#9987 = EDGE_LOOP ( 'NONE', ( #4495, #22096, #12662, #19433 ) ) ;
#9988 = CARTESIAN_POINT ( 'NONE',  ( 10.69999999997181028, -24.37874960104799626, -29.91132621206058317 ) ) ;
#9989 = ORIENTED_EDGE ( 'NONE', *, *, #23655, .T. ) ;
#9990 = CARTESIAN_POINT ( 'NONE',  ( 3.233792851425277171, 2.806794219454205930, -38.84813418134861251 ) ) ;
#9991 = CARTESIAN_POINT ( 'NONE',  ( -4.185763533044374540, 4.163314928055855901, -69.42322600472500937 ) ) ;
#9992 = ORIENTED_EDGE ( 'NONE', *, *, #30762, .T. ) ;
#9993 = CARTESIAN_POINT ( 'NONE',  ( -4.121720561938956529, -3.673096573571036139, -25.84101932450001016 ) ) ;
#9994 = FACE_OUTER_BOUND ( 'NONE', #27441, .T. ) ;
#9995 = VECTOR ( 'NONE', #25095, 1000.000000000000000 ) ;
#9996 = CARTESIAN_POINT ( 'NONE',  ( -3.948109860491266776, 2.321589337205137937, -44.84354844312500177 ) ) ;
#9997 = CARTESIAN_POINT ( 'NONE',  ( 8.700000000238844677, -25.09064271401819113, -26.05287923382458004 ) ) ;
#9998 = CARTESIAN_POINT ( 'NONE',  ( 0.9598841921113454578, -27.48329941562163370, 224.4438356452711503 ) ) ;
#9999 = EDGE_CURVE ( 'NONE', #2499, #15963, #12312, .T. ) ;
#10000 = CARTESIAN_POINT ( 'NONE',  ( -7.999999999640660775, -13.05987697124905367, -39.51663027436784148 ) ) ;
#10001 = UNCERTAINTY_MEASURE_WITH_UNIT (LENGTH_MEASURE( 1.000000000000000082E-05 ), #15439, 'distance_accuracy_value', 'NONE');
#10002 = DIRECTION ( 'NONE',  ( 1.000000000000000000, 0.000000000000000000, 0.000000000000000000 ) ) ;
#10003 = AXIS2_PLACEMENT_3D ( 'NONE', #20731, #18036, #18369 ) ;
#10004 = CARTESIAN_POINT ( 'NONE',  ( 10.69999999999999929, -36.62914859500000375, -26.86371135770000151 ) ) ;
#10005 = ORIENTED_EDGE ( 'NONE', *, *, #31002, .T. ) ;
#10006 = CARTESIAN_POINT ( 'NONE',  ( 3.427383197809986903, 1.063472793664595129, 227.6973195743642862 ) ) ;
#10007 = CARTESIAN_POINT ( 'NONE',  ( 23.73992238018677625, -12.43607998452291419, 224.9035646525462937 ) ) ;
#10008 = CARTESIAN_POINT ( 'NONE',  ( -10.69999999930000101, -30.49251257979999963, -21.04205368470000082 ) ) ;
#10009 = FACE_OUTER_BOUND ( 'NONE', #1524, .T. ) ;
#10010 = B_SPLINE_CURVE_WITH_KNOTS ( 'NONE', 1,
 ( #30327, #5195 ),
 .UNSPECIFIED., .F., .F.,
 ( 2, 2 ),
 ( -2.393070191420000080E-05, 0.7036780443879999680 ),
 .UNSPECIFIED. ) ;
#10011 = DIRECTION ( 'NONE',  ( 1.000000000000000000, 0.000000000000000000, 0.000000000000000000 ) ) ;
#10012 = CYLINDRICAL_SURFACE ( 'NONE', #16534, 3.000000000000001776 ) ;
#10013 = CARTESIAN_POINT ( 'NONE',  ( 0.9747465533911489066, -3.736773033513550946, -0.6999999999999991784 ) ) ;
#10014 = CARTESIAN_POINT ( 'NONE',  ( -27.55801272791059731, -0.5014288284350322256, -0.5592437529999827461 ) ) ;
#10015 = DIRECTION ( 'NONE',  ( -0.000000000000000000, 1.000000000000000000, -2.255973188440000244E-12 ) ) ;
#10016 = EDGE_CURVE ( 'NONE', #23190, #15903, #13464, .T. ) ;
#10017 = SURFACE_SIDE_STYLE ('',( #12519 ) ) ;
#10018 = CARTESIAN_POINT ( 'NONE',  ( 28.50000000000000000, -5.921189464669998951E-16, 222.0000000000000000 ) ) ;
#10019 = VECTOR ( 'NONE', #7299, 1000.000000000000000 ) ;
#10020 = EDGE_CURVE ( 'NONE', #2003, #14789, #12686, .T. ) ;
#10021 = CARTESIAN_POINT ( 'NONE',  ( -24.14619884835838093, -13.16136950043478748, 5.880491002298545489 ) ) ;
#10022 = DIRECTION ( 'NONE',  ( 0.000000000000000000, 0.000000000000000000, -1.000000000000000000 ) ) ;
#10023 = VERTEX_POINT ( 'NONE', #2142 ) ;
#10024 = CARTESIAN_POINT ( 'NONE',  ( -11.08346179031915568, -28.41490585489482967, 86.39444872449999480 ) ) ;
#10025 =( NAMED_UNIT ( * ) SI_UNIT ( $, .STERADIAN. ) SOLID_ANGLE_UNIT ( ) );
#10026 = VECTOR ( 'NONE', #21492, 1000.000000000000000 ) ;
#10027 = CARTESIAN_POINT ( 'NONE',  ( 0.000000000000000000, 20.70710678120000381, -44.39289321881399530 ) ) ;
#10028 = CARTESIAN_POINT ( 'NONE',  ( -5.463799992266447525, -1.435916617982112342, -56.93102360502499693 ) ) ;
#10029 = ORIENTED_EDGE ( 'NONE', *, *, #9375, .T. ) ;
#10030 = ITEM_DEFINED_TRANSFORMATION ( 'NONE', 'NONE', #2780,  #17722 ) ;
#10031 = EDGE_LOOP ( 'NONE', ( #24386, #15326, #16087, #22796 ) ) ;
#10032 = B_SPLINE_CURVE_WITH_KNOTS ( 'NONE', 3,
 ( #27176, #22618, #1059, #10502, #29690, #24969, #20241, #18189, #8275, #17869, #15520, #25126, #13156, #20404, #30786, #9211, #8751, #18972, #28261, #9367 ),
 .UNSPECIFIED., .F., .F.,
 ( 4, 1, 1, 1, 2, 2, 2, 1, 1, 1, 2, 2, 4 ),
 ( 0.000000000000000000, 0.1250000000000018596, 0.1875000000000018874, 0.2187500000000019151, 0.2343750000000011935, 0.2500000000000004441, 0.4999999999999968914, 0.6249999999999951150, 0.6874999999999942268, 0.7187499999999937828, 0.7343749999999943379, 0.7499999999999948930, 1.000000000000000000 ),
 .UNSPECIFIED. ) ;
#10034 = EDGE_CURVE ( 'NONE', #18767, #22309, #15995, .T. ) ;
#10033 = CARTESIAN_POINT ( 'NONE',  ( -8.881784197000000993E-16, 3.378317624991660661, -69.77707803651591689 ) ) ;
#10035 = EDGE_LOOP ( 'NONE', ( #24630, #290, #20740, #6204 ) ) ;
#10036 = VERTEX_POINT ( 'NONE', #28415 ) ;
#10037 = SURFACE_STYLE_USAGE ( .BOTH. , #28753 ) ;
#10038 = CARTESIAN_POINT ( 'NONE',  ( -24.49145440958036701, 14.57548795270903774, 4.319167817000008291 ) ) ;
#10039 = LINE ( 'NONE', #2799, #26025 ) ;
#10040 = CARTESIAN_POINT ( 'NONE',  ( 7.334768408830000475, -9.866585358490000957, 232.6627648150000027 ) ) ;
#10041 = CARTESIAN_POINT ( 'NONE',  ( 0.000000000000000000, 0.000000000000000000, 140.0000000000000000 ) ) ;
#10042 = CARTESIAN_POINT ( 'NONE',  ( 5.967946066639521874, -1.056419632483374116, -8.171482634700002023 ) ) ;
#10043 = CARTESIAN_POINT ( 'NONE',  ( 28.04325408089999883, -7.346495424229999571, 230.2432540810000319 ) ) ;
#10044 = VERTEX_POINT ( 'NONE', #11731 ) ;
#10045 = CARTESIAN_POINT ( 'NONE',  ( 2.559859836303097325, -3.484879554911406441, -44.10000000002499121 ) ) ;
#10046 = FACE_OUTER_BOUND ( 'NONE', #30019, .T. ) ;
#10047 = EDGE_CURVE ( 'NONE', #11948, #16822, #31075, .T. ) ;
#10048 = CARTESIAN_POINT ( 'NONE',  ( 4.354753084053725409, 0.1085053810021691101, -20.67661200060000226 ) ) ;
#10049 = CARTESIAN_POINT ( 'NONE',  ( -12.44385388530932701, -25.85073127557643247, -33.50965282259626576 ) ) ;
#10050 = VECTOR ( 'NONE', #16454, 1000.000000000000227 ) ;
#10051 = CARTESIAN_POINT ( 'NONE',  ( 0.000000000000000000, 0.000000000000000000, 90.00000000000000000 ) ) ;
#10052 = B_SPLINE_SURFACE_WITH_KNOTS ( 'NONE', 5, 1, ( 
 ( #18485, #30132 ),
 ( #3536, #27767 ),
 ( #29970, #10625 ),
 ( #6528, #10783 ),
 ( #20379, #29812 ),
 ( #22905, #18330 ),
 ( #6054, #23065 ),
 ( #25261, #3693 ),
 ( #15820, #13296 ),
 ( #1345, #27933 ),
 ( #3858, #1508 ),
 ( #11100, #6374 ) ),
 .UNSPECIFIED., .F., .F., .F.,
 ( 6, 3, 3, 6 ),
 ( 2, 2 ),
 ( 0.000000000000000000, 0.5717440563379999618, 1.143488112680000057, 1.429360140840000071 ),
 ( -0.7000000000009999335, 0.002002273473629999963 ),
 .UNSPECIFIED. ) ;
#10053 = CARTESIAN_POINT ( 'NONE',  ( -23.77307140041805411, 14.41181874028064591, 4.999998581000003384 ) ) ;
#10054 = CARTESIAN_POINT ( 'NONE',  ( -15.76765990766156733, 11.30637938232363204, -0.6999999999999785283 ) ) ;
#10055 = CARTESIAN_POINT ( 'NONE',  ( 5.925978784015399903, -0.8792241758803844842, -45.65818262062499855 ) ) ;
#10056 = CARTESIAN_POINT ( 'NONE',  ( -7.999999999949641172, -113.1810333093661995, 6.475256412746450252 ) ) ;
#10057 = CARTESIAN_POINT ( 'NONE',  ( -15.96623771770940969, 11.69189214367815843, -4.336808689942017736E-16 ) ) ;
#10058 = CARTESIAN_POINT ( 'NONE',  ( 8.699999999970108533, -117.2796036033498268, 12.53378553140980323 ) ) ;
#10059 = CARTESIAN_POINT ( 'NONE',  ( -26.28018753080000280, 9.189075756099999381, 229.9172022029999880 ) ) ;
#10060 = LINE ( 'NONE', #21556, #16282 ) ;
#10061 = VERTEX_POINT ( 'NONE', #1993 ) ;
#10062 = CARTESIAN_POINT ( 'NONE',  ( 3.473119624653126181, -3.299750202710006963, -30.98876389020000133 ) ) ;
#10063 = VERTEX_POINT ( 'NONE', #21178 ) ;
#10064 = CARTESIAN_POINT ( 'NONE',  ( -10.00000000026539126, -35.47767383571155619, -24.90806880955480551 ) ) ;
#10065 = CARTESIAN_POINT ( 'NONE',  ( -0.5163256777700186984, 4.538631023554798638, -48.26410749632499630 ) ) ;
#10066 = EDGE_LOOP ( 'NONE', ( #22420, #15236, #28543, #22759 ) ) ;
#10067 = ORIENTED_EDGE ( 'NONE', *, *, #8927, .T. ) ;
#10068 = CIRCLE ( 'NONE', #15573, 5.000000000000000000 ) ;
#10069 = DIRECTION ( 'NONE',  ( 0.000000000000000000, 0.000000000000000000, 1.000000000000000000 ) ) ;
#10070 = B_SPLINE_CURVE_WITH_KNOTS ( 'NONE', 3,
 ( #723, #27293, #1178, #10468 ),
 .UNSPECIFIED., .F., .F.,
 ( 4, 4 ),
 ( 0.000000000000000000, 1.000000000000000000 ),
 .UNSPECIFIED. ) ;
#10071 = VERTEX_POINT ( 'NONE', #21335 ) ;
#10072 = CARTESIAN_POINT ( 'NONE',  ( 20.05931974663578288, 19.99997412885312542, 229.7488604916501913 ) ) ;
#10073 = EDGE_CURVE ( 'NONE', #1536, #4103, #4185, .T. ) ;
#10074 = EDGE_LOOP ( 'NONE', ( #10414, #16705, #10845, #17438, #448, #18215 ) ) ;
#10075 = CARTESIAN_POINT ( 'NONE',  ( -10.79767709090000061, -24.52928868880000124, -0.9448358073000027169 ) ) ;
#10076 = LINE ( 'NONE', #12115, #15269 ) ;
#10077 = CARTESIAN_POINT ( 'NONE',  ( 9.999999999966270536, -29.52728889296171744, -26.74669651331937104 ) ) ;
#10078 = CARTESIAN_POINT ( 'NONE',  ( 0.4552590567128736998, 4.266916551624608367, -35.70000000000000284 ) ) ;
#10079 = EDGE_CURVE ( 'NONE', #3666, #4458, #9360, .T. ) ;
#10080 = EDGE_CURVE ( 'NONE', #20395, #15903, #6389, .T. ) ;
#10081 = FACE_OUTER_BOUND ( 'NONE', #4457, .T. ) ;
#10082 = DIRECTION ( 'NONE',  ( -0.9316362575375349842, 0.3633921898465292122, -0.000000000000000000 ) ) ;
#10083 = CARTESIAN_POINT ( 'NONE',  ( 2.223383862040885450, -3.430296892840217993, -0.1659393883000001568 ) ) ;
#10084 = CARTESIAN_POINT ( 'NONE',  ( -27.54391552379999908, 3.373045395960000230E-15, 42.95625301639999805 ) ) ;
#10085 = B_SPLINE_CURVE_WITH_KNOTS ( 'NONE', 5,
 ( #3051, #10603, #8379, #27281, #6030, #5413, #17976, #20198, #5721, #24927, #29791, #27589, #17825, #13108, #25079 ),
 .UNSPECIFIED., .F., .F.,
 ( 6, 3, 3, 3, 6 ),
 ( 0.000000000000000000, 0.3000000000011452950, 0.6000000000034357850, 0.9000000000022905233, 1.000000000000000000 ),
 .UNSPECIFIED. ) ;
#10086 = CARTESIAN_POINT ( 'NONE',  ( 3.619519562537647062, 2.908736503316577515, -8.854586407999997633 ) ) ;
#10087 = CARTESIAN_POINT ( 'NONE',  ( -4.607598934103576127, 1.311847319348407481, -30.36408078970000801 ) ) ;
#10088 = CARTESIAN_POINT ( 'NONE',  ( -6.992667155225802844, -16.10181445525363841, -74.73891072835350258 ) ) ;
#10089 = CARTESIAN_POINT ( 'NONE',  ( 24.09407739349263622, -13.86899051603569255, 6.002806299999996043 ) ) ;
#10090 = CARTESIAN_POINT ( 'NONE',  ( 8.000000000000000000, -15.86465192213301556, -74.65259062561435144 ) ) ;
#10091 = CARTESIAN_POINT ( 'NONE',  ( 5.999999999999999112, -30.20957738316099395, -79.87371650620046637 ) ) ;
#10092 = CARTESIAN_POINT ( 'NONE',  ( -24.37165444408190851, 14.77472139917419369, 4.999998581000003384 ) ) ;
#10093 = CARTESIAN_POINT ( 'NONE',  ( -1.932773295258156887, 4.259541830411037289, -31.72635571290000200 ) ) ;
#10094 = CARTESIAN_POINT ( 'NONE',  ( 1.495522319900055574, -27.76012052182101542, 5.506490228000010312 ) ) ;
#10095 = LINE ( 'NONE', #3005, #9219 ) ;
#10096 = CARTESIAN_POINT ( 'NONE',  ( -1.833239707743530955, -3.500000000000507594, 230.5777212759286670 ) ) ;
#10097 = EDGE_LOOP ( 'NONE', ( #671, #15822, #22743, #26627, #27824 ) ) ;
#10098 = CARTESIAN_POINT ( 'NONE',  ( 18.26639035967037827, -8.979988381807324060, -0.6999999999999784173 ) ) ;
#10099 = CARTESIAN_POINT ( 'NONE',  ( -12.35698168758728777, -32.00000000000000711, -27.45509309272506826 ) ) ;
#10100 = ORIENTED_EDGE ( 'NONE', *, *, #23764, .F. ) ;
#10101 = B_SPLINE_CURVE_WITH_KNOTS ( 'NONE', 3,
 ( #4624, #11865, #31064, #21625, #1968, #23991 ),
 .UNSPECIFIED., .F., .F.,
 ( 4, 2, 4 ),
 ( 0.000000000000000000, 0.5000000000000000000, 1.000000000000000000 ),
 .UNSPECIFIED. ) ;
#10102 = B_SPLINE_CURVE_WITH_KNOTS ( 'NONE', 5,
 ( #25384, #1469, #22864, #15154, #6016, #15614, #3650, #22702, #27117, #1308, #10738, #17511 ),
 .UNSPECIFIED., .F., .F.,
 ( 6, 3, 3, 6 ),
 ( 0.000000000000000000, 2.408321944279999904, 4.816680746389999435, 4.935551041960000163 ),
 .UNSPECIFIED. ) ;
#10103 = CARTESIAN_POINT ( 'NONE',  ( 0.5496038886516223521, 2.045530029741057021, 226.6412452697799722 ) ) ;
#10104 = CARTESIAN_POINT ( 'NONE',  ( -8.699999999694114194, -28.22468611108677194, -31.13863906519358693 ) ) ;
#10105 = VERTEX_POINT ( 'NONE', #18651 ) ;
#10106 = CARTESIAN_POINT ( 'NONE',  ( -4.679595096517847885, 0.7234518752358163329, -44.10000000002499121 ) ) ;
#10107 = ORIENTED_EDGE ( 'NONE', *, *, #19213, .F. ) ;
#10108 = ORIENTED_EDGE ( 'NONE', *, *, #16660, .F. ) ;
#10109 = FILL_AREA_STYLE ('',( #526 ) ) ;
#10110 = ORIENTED_EDGE ( 'NONE', *, *, #26962, .F. ) ;
#10111 = CARTESIAN_POINT ( 'NONE',  ( 27.04041630560000087, 3.053900541549999745E-14, 230.6999999999999886 ) ) ;
#10112 = CARTESIAN_POINT ( 'NONE',  ( 8.700000000247854359, -24.42167197180108573, -29.98317312617670538 ) ) ;
#10113 = B_SPLINE_CURVE_WITH_KNOTS ( 'NONE', 5,
 ( #23706, #25444, #13944, #3877, #28253, #25754, #20712, #6542, #13466, #16140, #1994, #1833, #6696, #16296, #23558 ),
 .UNSPECIFIED., .F., .F.,
 ( 6, 3, 3, 3, 6 ),
 ( 0.000000000000000000, 0.2500000000035760284, 0.4999999999999331091, 0.7500000000052684523, 1.000000000000000000 ),
 .UNSPECIFIED. ) ;
#10114 = CARTESIAN_POINT ( 'NONE',  ( 16.40303402075260308, 10.20816091466531716, -0.6999999999999784173 ) ) ;
#10115 = ORIENTED_EDGE ( 'NONE', *, *, #4712, .T. ) ;
#10116 = CARTESIAN_POINT ( 'NONE',  ( -25.16696685493285202, 13.37570800105521585, 6.002806401000010617 ) ) ;
#10117 = CARTESIAN_POINT ( 'NONE',  ( -14.60916135985672071, 28.04296594682689658, 8.000000000000007105 ) ) ;
#10118 = EDGE_CURVE ( 'NONE', #11243, #24111, #18502, .T. ) ;
#10119 = CARTESIAN_POINT ( 'NONE',  ( -3.072394438959999974, -1.678456730820000020, 227.6468472915199754 ) ) ;
#10120 = CARTESIAN_POINT ( 'NONE',  ( 4.175165894169885483, -119.7166638525666826, -43.39999999999999858 ) ) ;
#10121 = ORIENTED_EDGE ( 'NONE', *, *, #25043, .F. ) ;
#10122 = CARTESIAN_POINT ( 'NONE',  ( -12.94794535325927676, 25.03405588289514938, -59.76667836462032568 ) ) ;
#10123 = CARTESIAN_POINT ( 'NONE',  ( -3.117834729128555971, -4.866792379758847709, -18.10544088820000042 ) ) ;
#10124 = CARTESIAN_POINT ( 'NONE',  ( -26.62724484483129572, -3.508068424019920695, 193.2171415880000325 ) ) ;
#10125 = CARTESIAN_POINT ( 'NONE',  ( -8.699999999708559528, -29.94314889530440738, -29.10209438447943953 ) ) ;
#10126 = B_SPLINE_CURVE_WITH_KNOTS ( 'NONE', 3,
 ( #7114, #23656, #11682, #13733, #21282, #9005 ),
 .UNSPECIFIED., .F., .F.,
 ( 4, 2, 4 ),
 ( 0.000000000000000000, 0.4999999999999986677, 1.000000000000000000 ),
 .UNSPECIFIED. ) ;
#10127 = CARTESIAN_POINT ( 'NONE',  ( 3.853224190864724896, -19.62827330940682202, -27.90582062084719439 ) ) ;
#10128 = CARTESIAN_POINT ( 'NONE',  ( 0.5746121234323043891, -27.79431838510023667, 3.901346086000012647 ) ) ;
#10129 = CARTESIAN_POINT ( 'NONE',  ( -24.82552935800767457, 12.51236512602968887, 4.712680001979744127 ) ) ;
#10130 = DIRECTION ( 'NONE',  ( -0.000000000000000000, -0.000000000000000000, -1.000000000000000000 ) ) ;
#10131 = DIRECTION ( 'NONE',  ( -1.000000000000000000, 0.000000000000000000, 0.000000000000000000 ) ) ;
#10132 = CARTESIAN_POINT ( 'NONE',  ( 21.31445244760000080, 17.08994352740000267, 230.0000000000000000 ) ) ;
#10133 = CARTESIAN_POINT ( 'NONE',  ( -13.99999999969999820, 21.69999999929999390, -67.09999999999999432 ) ) ;
#10134 = ORIENTED_EDGE ( 'NONE', *, *, #29615, .T. ) ;
#10135 = CARTESIAN_POINT ( 'NONE',  ( 2.776548632478545553, -3.583402058917904753, -52.50430438132499233 ) ) ;
#10136 = CARTESIAN_POINT ( 'NONE',  ( -28.49528339128749366, -0.5184828350247674411, 1.000000000000000888 ) ) ;
#10137 = CARTESIAN_POINT ( 'NONE',  ( -24.18086174036168856, 13.20182724809068553, 0.000000000000000000 ) ) ;
#10138 = CARTESIAN_POINT ( 'NONE',  ( -4.438363504809300863, 1.105440681516749235, -68.10000000002499121 ) ) ;
#10139 = ORIENTED_EDGE ( 'NONE', *, *, #11548, .T. ) ;
#10140 = ADVANCED_FACE ( 'NONE', ( #14257, #23402 ), #11426, .T. ) ;
#10141 = CARTESIAN_POINT ( 'NONE',  ( 3.056341819332166310, -2.413956206206734123, -96.46963879144223597 ) ) ;
#10142 = B_SPLINE_SURFACE_WITH_KNOTS ( 'NONE', 5, 1, ( 
 ( #14185, #28339 ),
 ( #25991, #26295 ),
 ( #26146, #9136 ),
 ( #23788, #28795 ),
 ( #16686, #8987 ),
 ( #31016, #7097 ),
 ( #30559, #4740 ),
 ( #18740, #9612 ),
 ( #16383, #21584 ),
 ( #21427, #2073 ),
 ( #6787, #16226 ),
 ( #11512, #25840 ),
 ( #14034, #6626 ),
 ( #28497, #9453 ),
 ( #18587, #11664 ) ),
 .UNSPECIFIED., .F., .F., .F.,
 ( 6, 3, 3, 3, 6 ),
 ( 2, 2 ),
 ( 0.000000000000000000, 0.5777958940569999369, 1.155591788109999962, 2.022285629200000212, 2.888979470280000239 ),
 ( -1.118726812310000082E-05, 0.7031447686210000603 ),
 .UNSPECIFIED. ) ;
#10143 = CIRCLE ( 'NONE', #3588, 12.03781779390000040 ) ;
#10144 = VERTEX_POINT ( 'NONE', #27948 ) ;
#10145 = CARTESIAN_POINT ( 'NONE',  ( 24.12437077020566534, 15.17512415148409133, 5.965434402546257786 ) ) ;
#10146 = AXIS2_PLACEMENT_3D ( 'NONE', #3168, #7884, #5840 ) ;
#10147 = DIRECTION ( 'NONE',  ( 1.000000000000000000, -0.000000000000000000, 0.000000000000000000 ) ) ;
#10148 = VECTOR ( 'NONE', #21684, 1000.000000000000114 ) ;
#10149 = ORIENTED_EDGE ( 'NONE', *, *, #22380, .T. ) ;
#10150 = CARTESIAN_POINT ( 'NONE',  ( -3.253989917302559043, -2.899813084402115049, -24.84101932450000305 ) ) ;
#10151 = CARTESIAN_POINT ( 'NONE',  ( -9.738910687886855655, -24.96785170200598714, 186.7828584120000244 ) ) ;
#10152 = CARTESIAN_POINT ( 'NONE',  ( -28.58473218748631339, 4.397531023511127124, 1.000000000000000888 ) ) ;
#10153 = CARTESIAN_POINT ( 'NONE',  ( 7.638687372266931952, -2.231046042376699567, -39.72882113109005076 ) ) ;
#10154 = DIRECTION ( 'NONE',  ( -0.8660254037843289066, -0.5000000000001899592, 0.000000000000000000 ) ) ;
#10155 = CARTESIAN_POINT ( 'NONE',  ( -3.389121577680000108, -11.55088360999999963, 224.6412452697800290 ) ) ;
#10156 = CARTESIAN_POINT ( 'NONE',  ( -7.999999999683791607, -15.80258142959463363, -33.02070610725625954 ) ) ;
#10157 = CARTESIAN_POINT ( 'NONE',  ( -0.1258946531760308241, -17.01754440315029271, -109.8342699011357126 ) ) ;
#10158 = CIRCLE ( 'NONE', #24239, 2.000000000000000000 ) ;
#10159 = ORIENTED_EDGE ( 'NONE', *, *, #16817, .T. ) ;
#10160 = CARTESIAN_POINT ( 'NONE',  ( 14.69473318574048015, -31.99965463203811211, -26.74399720207908260 ) ) ;
#10161 = CARTESIAN_POINT ( 'NONE',  ( 8.700000000288625301, -16.67085403793054255, -37.94852427682175744 ) ) ;
#10162 = CARTESIAN_POINT ( 'NONE',  ( -23.29312071521372118, -15.17488101142239643, 5.506989586000016423 ) ) ;
#10163 = CARTESIAN_POINT ( 'NONE',  ( 0.8697582157755545662, -3.930924299790361509, -38.89973510835485371 ) ) ;
#10164 = CARTESIAN_POINT ( 'NONE',  ( 9.999999999962405184, -25.59333594965072223, -25.74355301541976360 ) ) ;
#10165 = DIRECTION ( 'NONE',  ( 1.000000000000000000, 0.000000000000000000, 0.000000000000000000 ) ) ;
#10166 = CARTESIAN_POINT ( 'NONE',  ( 3.380431529615641750, -2.586477721823119857, -0.6999999999999992895 ) ) ;
#10167 = CARTESIAN_POINT ( 'NONE',  ( 14.40197535836999876, -32.00000000000000000, -25.51324865394999719 ) ) ;
#10168 = CARTESIAN_POINT ( 'NONE',  ( -10.32522729140000095, -24.86557399950000047, -1.399999999999998579 ) ) ;
#10169 = CARTESIAN_POINT ( 'NONE',  ( 17.16657240420000008, 10.97998838177520931, 0.05106179917585291356 ) ) ;
#10170 = CARTESIAN_POINT ( 'NONE',  ( 3.552713678799999608E-15, -3.552713678799999608E-15, 136.7828584120000244 ) ) ;
#10171 = EDGE_CURVE ( 'NONE', #16061, #7420, #19051, .T. ) ;
#10173 = CARTESIAN_POINT ( 'NONE',  ( -20.77057278543777485, -16.95162108973866921, 93.21714158846111786 ) ) ;
#10172 = APPLICATION_CONTEXT ( 'automotive_design' ) ;
#10174 = CARTESIAN_POINT ( 'NONE',  ( -0.5944614571882205212, -27.79380703160649446, 4.999998581000003384 ) ) ;
#10175 = ORIENTED_EDGE ( 'NONE', *, *, #25212, .F. ) ;
#10176 = ADVANCED_FACE ( 'NONE', ( #16295 ), #14102, .F. ) ;
#10177 = CARTESIAN_POINT ( 'NONE',  ( 11.69999999989999928, -24.11120071670000087, -1.399999999999998579 ) ) ;
#10178 =( NAMED_UNIT ( * ) SI_UNIT ( $, .STERADIAN. ) SOLID_ANGLE_UNIT ( ) );
#10179 = CARTESIAN_POINT ( 'NONE',  ( 24.73445225629999911, -14.15837998019999944, 226.0959682270000144 ) ) ;
#10180 = B_SPLINE_CURVE_WITH_KNOTS ( 'NONE', 5,
 ( #279, #9858, #19456, #26688, #29049, #7494, #14738, #12370, #23726 ),
 .UNSPECIFIED., .F., .F.,
 ( 6, 3, 6 ),
 ( 0.000000000000000000, 55.31395627320000585, 94.75474476520000167 ),
 .UNSPECIFIED. ) ;
#10181 = CARTESIAN_POINT ( 'NONE',  ( -1.494970809075166329, -6.161113191638062148, -62.42311227092500303 ) ) ;
#10182 = ORIENTED_EDGE ( 'NONE', *, *, #5246, .F. ) ;
#10183 = ORIENTED_EDGE ( 'NONE', *, *, #8533, .F. ) ;
#10184 = CARTESIAN_POINT ( 'NONE',  ( -17.04621913067799710, -22.00000000000000000, -31.28675134614999820 ) ) ;
#10185 = ORIENTED_EDGE ( 'NONE', *, *, #1225, .F. ) ;
#10186 = ORIENTED_EDGE ( 'NONE', *, *, #24494, .T. ) ;
#10187 = EDGE_CURVE ( 'NONE', #14604, #22866, #8560, .T. ) ;
#10188 = FACE_BOUND ( 'NONE', #1456, .T. ) ;
#10189 = CARTESIAN_POINT ( 'NONE',  ( -24.92013865347427171, 13.82966157970119525, 3.899998581000013509 ) ) ;
#10190 = CARTESIAN_POINT ( 'NONE',  ( -28.49530731802708416, -0.5184832703812605192, 8.000000000000007105 ) ) ;
#10191 = ADVANCED_FACE ( 'NONE', ( #6695 ), #30775, .T. ) ;
#10192 = B_SPLINE_CURVE_WITH_KNOTS ( 'NONE', 5,
 ( #12388, #138, #2492, #7050, #9567, #16640 ),
 .UNSPECIFIED., .F., .F.,
 ( 6, 6 ),
 ( 0.000000000000000000, 21.97608269730000075 ),
 .UNSPECIFIED. ) ;
#10193 = CARTESIAN_POINT ( 'NONE',  ( 4.917756447549999521, 10.96637803540000000, 231.9999991140000191 ) ) ;
#10194 = DIRECTION ( 'NONE',  ( 1.000000000000000000, 0.000000000000000000, 0.000000000000000000 ) ) ;
#10195 = CARTESIAN_POINT ( 'NONE',  ( -3.099128499470596321, -3.102542665468454253, -9.813991631000003935 ) ) ;
#10196 = CARTESIAN_POINT ( 'NONE',  ( 4.096142159599999388, 4.096142159599999388, 226.6412452697800006 ) ) ;
#10197 = ORIENTED_EDGE ( 'NONE', *, *, #1046, .F. ) ;
#10198 = CARTESIAN_POINT ( 'NONE',  ( 2.733853777285388365, -3.446019709399517517, -44.10000000002499121 ) ) ;
#10199 = DIRECTION ( 'NONE',  ( 0.000000000000000000, 0.000000000000000000, -1.000000000000000000 ) ) ;
#10200 = PRODUCT_RELATED_PRODUCT_CATEGORY ( 'part', '', ( #3799 ) ) ;
#10201 = CARTESIAN_POINT ( 'NONE',  ( 0.1332961122732720383, -6.531058726825651028, -25.01888333259999442 ) ) ;
#10202 = CARTESIAN_POINT ( 'NONE',  ( -12.38103409318511083, -23.51166759135386641, -32.15925398282187331 ) ) ;
#10203 = CARTESIAN_POINT ( 'NONE',  ( -16.14153545196241524, 10.13281012202415177, -4.336808689942017736E-16 ) ) ;
#10204 = VECTOR ( 'NONE', #29469, 1000.000000000000000 ) ;
#10205 = CARTESIAN_POINT ( 'NONE',  ( -24.34663841809999951, -12.78636765230000094, 5.000000000000000000 ) ) ;
#10206 = CARTESIAN_POINT ( 'NONE',  ( -2.884696998040799709, 4.705809124755043982, -44.25531229042500314 ) ) ;
#10207 = CARTESIAN_POINT ( 'NONE',  ( -10.69999999999999929, -126.5194192958999935, -33.65254911369999746 ) ) ;
#10208 = CARTESIAN_POINT ( 'NONE',  ( -26.80000000069999899, 3.281945028329999726E-15, 143.2171415869999862 ) ) ;
#10209 = CARTESIAN_POINT ( 'NONE',  ( -18.94791452757604944, 20.00033874320078908, 230.5288124007003887 ) ) ;
#10210 = EDGE_CURVE ( 'NONE', #1959, #25501, #11914, .T. ) ;
#10211 = DIRECTION ( 'NONE',  ( 0.000000000000000000, 0.000000000000000000, 1.000000000000000000 ) ) ;
#10212 = CARTESIAN_POINT ( 'NONE',  ( 24.29812717141672707, -12.87956648207215515, 225.4905541419588815 ) ) ;
#10213 = ORIENTED_EDGE ( 'NONE', *, *, #26629, .T. ) ;
#10214 = CARTESIAN_POINT ( 'NONE',  ( -5.864216825201565619, 1.669623860961706674, -31.90158078969999877 ) ) ;
#10215 = ORIENTED_EDGE ( 'NONE', *, *, #13092, .F. ) ;
#10216 = AXIS2_PLACEMENT_3D ( 'NONE', #15267, #963, #10554 ) ;
#10217 = CARTESIAN_POINT ( 'NONE',  ( 25.32653163311281830, -13.07087917458821202, 4.239730452999995514 ) ) ;
#10218 = CARTESIAN_POINT ( 'NONE',  ( -1.572917327626556228, -4.621985533170462901, -47.74520033292501608 ) ) ;
#10219 = VERTEX_POINT ( 'NONE', #26823 ) ;
#10220 = EDGE_CURVE ( 'NONE', #30960, #24425, #18440, .T. ) ;
#10221 = AXIS2_PLACEMENT_3D ( 'NONE', #807, #15416, #1264 ) ;
#10222 = ORIENTED_EDGE ( 'NONE', *, *, #5597, .T. ) ;
#10223 = APPLICATION_PROTOCOL_DEFINITION ( 'draft international standard', 'automotive_design', 1998, #19223 ) ;
#10224 = AXIS2_PLACEMENT_3D ( 'NONE', #8032, #5676, #5215 ) ;
#10225 = ORIENTED_EDGE ( 'NONE', *, *, #1388, .F. ) ;
#10226 = ORIENTED_EDGE ( 'NONE', *, *, #10992, .T. ) ;
#10227 = VECTOR ( 'NONE', #14577, 1000.000000000000000 ) ;
#10228 = ADVANCED_FACE ( 'NONE', ( #29331 ), #26518, .F. ) ;
#10229 = CARTESIAN_POINT ( 'NONE',  ( 24.68173674080000168, -14.25001227039999918, 226.1000014189999945 ) ) ;
#10230 = CARTESIAN_POINT ( 'NONE',  ( -5.510824522656250224, -9.335491771010991258, -36.26375142553751374 ) ) ;
#10231 = CARTESIAN_POINT ( 'NONE',  ( 9.999999999899998215, -2.500000000000002220, -2.399999999999999467 ) ) ;
#10232 = LINE ( 'NONE', #19832, #31027 ) ;
#10233 = LINE ( 'NONE', #29726, #2540 ) ;
#10234 = EDGE_CURVE ( 'NONE', #1598, #10318, #717, .T. ) ;
#10235 = CARTESIAN_POINT ( 'NONE',  ( -4.082901699294640530, 2.312515566788601262, -0.6999999999999991784 ) ) ;
#10236 = LINE ( 'NONE', #10387, #7214 ) ;
#10237 = LINE ( 'NONE', #17458, #17019 ) ;
#10238 = CARTESIAN_POINT ( 'NONE',  ( 4.880902371519058036, -3.592936783560450653, -9.572776792900008047 ) ) ;
#10239 = CARTESIAN_POINT ( 'NONE',  ( 2.022420680230021972, -3.847796821814266632, -33.20721934060000535 ) ) ;
#10240 = CARTESIAN_POINT ( 'NONE',  ( 1.099998490678698593, -27.77839035186433136, 225.0734570122248215 ) ) ;
#10241 = CARTESIAN_POINT ( 'NONE',  ( 23.88992819277635959, -14.21747995518237317, 5.680829342999987652 ) ) ;
#10242 = CARTESIAN_POINT ( 'NONE',  ( 23.85408961476034051, 14.27673465474052072, 6.098654221000004760 ) ) ;
#10243 = CIRCLE ( 'NONE', #18265, 4.000000004070001225 ) ;
#10244 = CARTESIAN_POINT ( 'NONE',  ( -27.56257419730000180, -2.940926349879999851E-14, 230.5592437530000041 ) ) ;
#10245 = CARTESIAN_POINT ( 'NONE',  ( 0.09521150875770739708, -4.665041947735808492, -24.41888333260000365 ) ) ;
#10246 = CIRCLE ( 'NONE', #8195, 3.200000000000000178 ) ;
#10247 = AXIS2_PLACEMENT_3D ( 'NONE', #30999, #6028, #20672 ) ;
#10248 = CARTESIAN_POINT ( 'NONE',  ( 0.7459188900473354700, -27.79046661982714639, 6.079790450999988494 ) ) ;
#10249 = CARTESIAN_POINT ( 'NONE',  ( -24.36130770023227043, -13.39283555866521525, 4.791638085000021974 ) ) ;
#10250 = CARTESIAN_POINT ( 'NONE',  ( -7.003284688416608894, -8.398564518084793207, -36.72072137990513596 ) ) ;
#10251 = EDGE_CURVE ( 'NONE', #23079, #13180, #19594, .T. ) ;
#10252 = ORIENTED_EDGE ( 'NONE', *, *, #25988, .T. ) ;
#10253 = B_SPLINE_CURVE_WITH_KNOTS ( 'NONE', 3,
 ( #29612, #5536, #24591, #17640, #24742, #5844, #20323, #29921, #15446, #10424, #5690, #22685 ),
 .UNSPECIFIED., .F., .F.,
 ( 4, 2, 2, 2, 2, 4 ),
 ( 0.000000000000000000, 0.2500000000000002776, 0.5000000000000005551, 0.6250000000000001110, 0.7499999999999996669, 1.000000000000000000 ),
 .UNSPECIFIED. ) ;
#10254 = EDGE_CURVE ( 'NONE', #4699, #6773, #6381, .T. ) ;
#10255 = CARTESIAN_POINT ( 'NONE',  ( 1.645560275461343203, -28.45273235261698019, 4.999998581000003384 ) ) ;
#10256 = CARTESIAN_POINT ( 'NONE',  ( -12.48017473518110521, -32.00000000000000000, -26.57817950442041166 ) ) ;
#10257 = VERTEX_POINT ( 'NONE', #29174 ) ;
#10258 = DIRECTION ( 'NONE',  ( 0.000000000000000000, 0.3420201433259318358, -0.9396926207858125046 ) ) ;
#10259 = DIRECTION ( 'NONE',  ( 0.000000000000000000, 0.000000000000000000, -1.000000000000000000 ) ) ;
#10260 = VERTEX_POINT ( 'NONE', #19125 ) ;
#10261 = CARTESIAN_POINT ( 'NONE',  ( 7.636616881710000193, 9.305349148710000406, 230.6412452697800006 ) ) ;
#10262 = ORIENTED_EDGE ( 'NONE', *, *, #24670, .F. ) ;
#10263 = ADVANCED_FACE ( 'NONE', ( #2758 ), #5268, .F. ) ;
#10264 = VERTEX_POINT ( 'NONE', #19435 ) ;
#10265 = ORIENTED_EDGE ( 'NONE', *, *, #28555, .F. ) ;
#10266 = CARTESIAN_POINT ( 'NONE',  ( 28.50000000000000000, 3.195004098709999527E-14, 229.2404163060000144 ) ) ;
#10267 = LINE ( 'NONE', #20167, #25210 ) ;
#10268 = DIRECTION ( 'NONE',  ( 0.3633921898465276024, -0.9316362575375355393, -6.071532165918824830E-14 ) ) ;
#10269 = AXIS2_PLACEMENT_3D ( 'NONE', #30579, #18758, #2250 ) ;
#10270 = ORIENTED_EDGE ( 'NONE', *, *, #25225, .F. ) ;
#10271 = CARTESIAN_POINT ( 'NONE',  ( -24.98823330661245379, 13.70626928206978690, 6.095967861000000987 ) ) ;
#10272 = AXIS2_PLACEMENT_3D ( 'NONE', #18785, #6832, #8718 ) ;
#10273 = AXIS2_PLACEMENT_3D ( 'NONE', #15696, #5946, #15237 ) ;
#10274 = FACE_OUTER_BOUND ( 'NONE', #3680, .T. ) ;
#10275 = CYLINDRICAL_SURFACE ( 'NONE', #13019, 10.00000000000000533 ) ;
#10276 = DIRECTION ( 'NONE',  ( 0.000000000000000000, 0.000000000000000000, -1.000000000000000000 ) ) ;
#10277 = FACE_OUTER_BOUND ( 'NONE', #20005, .T. ) ;
#10278 = CARTESIAN_POINT ( 'NONE',  ( 3.736517203680826515, 4.566916950137848374, -19.25622222229999991 ) ) ;
#10279 = CARTESIAN_POINT ( 'NONE',  ( -0.8892886897209191233, -28.48641921395686794, 224.3203319190939737 ) ) ;
#10280 = CARTESIAN_POINT ( 'NONE',  ( 0.000000000000000000, 4.811145170119999648, -67.12721591429999535 ) ) ;
#10281 = STYLED_ITEM ( 'NONE', ( #23396 ), #2064 ) ;
#10282 = CARTESIAN_POINT ( 'NONE',  ( 23.32129337744305886, -14.57293380325871723, 225.5561643542927470 ) ) ;
#10283 = CARTESIAN_POINT ( 'NONE',  ( 22.97596219000000062, 15.65128142029999836, 222.0000000000000000 ) ) ;
#10284 = TOROIDAL_SURFACE ( 'NONE', #27599, 24.50000000000000000, 3.200000000000000178 ) ;
#10285 = CARTESIAN_POINT ( 'NONE',  ( 8.999999999770000869, 20.80003289834280977, -44.48586295459759299 ) ) ;
#10286 = DIRECTION ( 'NONE',  ( -0.000000000000000000, -0.000000000000000000, 1.000000000000000000 ) ) ;
#10287 = CARTESIAN_POINT ( 'NONE',  ( 25.98110156819999972, 9.099016333859999861, 230.0000000000000000 ) ) ;
#10288 = CARTESIAN_POINT ( 'NONE',  ( -7.999999999713793386, -30.00976070822369834, -28.70911656063094597 ) ) ;
#10289 = EDGE_CURVE ( 'NONE', #1493, #11656, #9385, .T. ) ;
#10290 = CIRCLE ( 'NONE', #5251, 26.80000000000000071 ) ;
#10291 = ORIENTED_EDGE ( 'NONE', *, *, #15967, .F. ) ;
#10292 = CARTESIAN_POINT ( 'NONE',  ( 3.357378826396556271, -2.722208303779470651, -55.40923804942499942 ) ) ;
#10293 = CARTESIAN_POINT ( 'NONE',  ( -0.1113126277073495929, 2.989789856717120387, -42.27519293863267791 ) ) ;
#10294 = VECTOR ( 'NONE', #22247, 1000.000000000000114 ) ;
#10295 = CIRCLE ( 'NONE', #8243, 4.439999999999999503 ) ;
#10296 = EDGE_CURVE ( 'NONE', #21919, #9128, #24013, .T. ) ;
#10297 = CARTESIAN_POINT ( 'NONE',  ( -2.041049994039236815, 3.920024695840365503, -39.39109296326683562 ) ) ;
#10298 = CARTESIAN_POINT ( 'NONE',  ( -4.451258330096496074, 1.095504858435497386, -68.10000000002500542 ) ) ;
#10299 = ADVANCED_FACE ( 'NONE', ( #7168 ), #16754, .F. ) ;
#10300 = ORIENTED_EDGE ( 'NONE', *, *, #20209, .F. ) ;
#10301 = CARTESIAN_POINT ( 'NONE',  ( -2.127246859535990353, 2.914123423714512384, -88.52261276242110455 ) ) ;
#10302 = EDGE_LOOP ( 'NONE', ( #29864, #13920, #3878, #9340, #21212, #25702, #6647 ) ) ;
#10303 = DIRECTION ( 'NONE',  ( 1.000000000000000000, 0.000000000000000000, 0.000000000000000000 ) ) ;
#10304 = PRESENTATION_LAYER_ASSIGNMENT (  '', '', ( #6275 ) ) ;
#10305 = DIRECTION ( 'NONE',  ( 4.428977494234582379E-12, 0.8987940462991651502, -0.4383711467890810676 ) ) ;
#10306 = ORIENTED_EDGE ( 'NONE', *, *, #17676, .F. ) ;
#10307 = CARTESIAN_POINT ( 'NONE',  ( 6.385918709370476343, 0.1527399656023400998, -63.58686508972500917 ) ) ;
#10308 = CARTESIAN_POINT ( 'NONE',  ( -22.52168649520000088, -19.90806591850000018, 229.9751242030000071 ) ) ;
#10309 = CARTESIAN_POINT ( 'NONE',  ( -27.57306739230703130, 9.318986405453829391, 0.5017677510000262409 ) ) ;
#10310 = LINE ( 'NONE', #14574, #11533 ) ;
#10311 =( LENGTH_UNIT ( ) NAMED_UNIT ( * ) SI_UNIT ( .MILLI., .METRE. ) );
#10312 = CARTESIAN_POINT ( 'NONE',  ( -15.79905445585067270, 10.59899472511377816, -1.400000000000001910 ) ) ;
#10313 = ORIENTED_EDGE ( 'NONE', *, *, #8956, .F. ) ;
#10314 = UNCERTAINTY_MEASURE_WITH_UNIT (LENGTH_MEASURE( 1.000000000000000082E-05 ), #12528, 'distance_accuracy_value', 'NONE');
#10315 = DIRECTION ( 'NONE',  ( 0.9002473904559572526, -0.4353787270609801308, 0.000000000000000000 ) ) ;
#10316 = B_SPLINE_CURVE_WITH_KNOTS ( 'NONE', 3,
 ( #23926, #9590, #4716, #7074 ),
 .UNSPECIFIED., .F., .F.,
 ( 4, 4 ),
 ( 0.000000000000000000, 1.000000000000000000 ),
 .UNSPECIFIED. ) ;
#10317 = CARTESIAN_POINT ( 'NONE',  ( 19.80538212960000166, 19.50875458629999670, 229.0000000010000178 ) ) ;
#10318 = VERTEX_POINT ( 'NONE', #10151 ) ;
#10319 = CARTESIAN_POINT ( 'NONE',  ( 14.40197535836999876, -32.00000000000000000, -31.28675134584999640 ) ) ;
#10320 = CARTESIAN_POINT ( 'NONE',  ( 23.68723484229111875, -12.53725850769392380, 224.5052107121046276 ) ) ;
#10321 = ADVANCED_FACE ( 'NONE', ( #9994 ), #15027, .F. ) ;
#10322 = CARTESIAN_POINT ( 'NONE',  ( -24.38199545545641911, -14.75707035126829147, 6.098654095000016540 ) ) ;
#10323 = CARTESIAN_POINT ( 'NONE',  ( 0.8618564855135213421, -0.4187060996060523732, -98.10259367259374130 ) ) ;
#10324 = CARTESIAN_POINT ( 'NONE',  ( -11.76276068685807985, -2.846903954059027519, 232.0000000000047748 ) ) ;
#10325 = CARTESIAN_POINT ( 'NONE',  ( -6.496986506900674918, -26.00150201275824102, 208.5476012337068425 ) ) ;
#10326 = CARTESIAN_POINT ( 'NONE',  ( 1.343267674844191406, -3.656436453084884519, -0.6999999999999991784 ) ) ;
#10327 = CARTESIAN_POINT ( 'NONE',  ( -28.45300238704230367, -0.5177135156027806717, 0.5017677510000262409 ) ) ;
#10328 = CARTESIAN_POINT ( 'NONE',  ( 8.999999999540001738, 19.99999999999999645, -44.09999999970998630 ) ) ;
#10329 = VECTOR ( 'NONE', #18435, 1000.000000000000000 ) ;
#10330 =( GEOMETRIC_REPRESENTATION_CONTEXT ( 3 ) GLOBAL_UNCERTAINTY_ASSIGNED_CONTEXT ( ( #15338 ) ) GLOBAL_UNIT_ASSIGNED_CONTEXT ( ( #16215, #9125, #18575 ) ) REPRESENTATION_CONTEXT ( 'NONE', 'WORKASPACE' ) );
#10331 = CARTESIAN_POINT ( 'NONE',  ( 11.20000000009999930, -29.50000000000000000, -24.06987298045999779 ) ) ;
#10332 = FACE_OUTER_BOUND ( 'NONE', #13220, .T. ) ;
#10333 = CARTESIAN_POINT ( 'NONE',  ( -5.393907605749490131, -26.25263145716210644, 20.79431568259033369 ) ) ;
#10334 = CARTESIAN_POINT ( 'NONE',  ( -1.060716232127552727, -3.772072411421167892, -68.10000000002499121 ) ) ;
#10335 = ORIENTED_EDGE ( 'NONE', *, *, #4405, .F. ) ;
#10336 = FACE_OUTER_BOUND ( 'NONE', #1562, .T. ) ;
#10337 = DIRECTION ( 'NONE',  ( 0.000000000000000000, 0.000000000000000000, 1.000000000000000000 ) ) ;
#10338 = CARTESIAN_POINT ( 'NONE',  ( 1.672654430053971852, 5.259243695923226269, -61.26492395752499931 ) ) ;
#10339 = VERTEX_POINT ( 'NONE', #26979 ) ;
#10340 = EDGE_LOOP ( 'NONE', ( #12282, #16269, #30055, #3663, #18140, #7822 ) ) ;
#10341 = CARTESIAN_POINT ( 'NONE',  ( 8.700000000288207858, -19.62571037376041261, -40.87651877822478497 ) ) ;
#10342 = ORIENTED_EDGE ( 'NONE', *, *, #10016, .F. ) ;
#10343 = ORIENTED_EDGE ( 'NONE', *, *, #6615, .T. ) ;
#10344 = EDGE_CURVE ( 'NONE', #16882, #6775, #14433, .T. ) ;
#10345 = CARTESIAN_POINT ( 'NONE',  ( 9.999999999979143794, -28.51085694194899389, -31.02135916461767096 ) ) ;
#10346 = CARTESIAN_POINT ( 'NONE',  ( -14.09657507470000226, -28.30410041510000241, 229.0000000000000000 ) ) ;
#10347 = DIRECTION ( 'NONE',  ( 1.000000000000000000, 0.000000000000000000, 0.000000000000000000 ) ) ;
#10348 = ADVANCED_FACE ( 'NONE', ( #17217 ), #25481, .F. ) ;
#10349 = CARTESIAN_POINT ( 'NONE',  ( -6.982632971260604116, 4.357143524085962838, -42.94209588230350505 ) ) ;
#10350 = CARTESIAN_POINT ( 'NONE',  ( -12.75378086759999796, -27.00000000000000355, -34.17350269210000135 ) ) ;
#10351 = LINE ( 'NONE', #29537, #31109 ) ;
#10352 = ORIENTED_EDGE ( 'NONE', *, *, #1838, .F. ) ;
#10353 = CARTESIAN_POINT ( 'NONE',  ( 2.499815048740641199, -3.503498767398317337, -44.10000000002499121 ) ) ;
#10354 = CARTESIAN_POINT ( 'NONE',  ( -8.699999999662093586, -15.94902145834643115, -35.53273252493492862 ) ) ;
#10355 = EDGE_CURVE ( 'NONE', #28202, #15917, #22961, .T. ) ;
#10356 = B_SPLINE_CURVE_WITH_KNOTS ( 'NONE', 3,
 ( #26484, #19564, #378, #7443 ),
 .UNSPECIFIED., .F., .F.,
 ( 4, 4 ),
 ( 0.000000000000000000, 1.000000000000000000 ),
 .UNSPECIFIED. ) ;
#10357 = CARTESIAN_POINT ( 'NONE',  ( -4.873044981369978323, 1.499374375125315684, -23.26039663399999924 ) ) ;
#10358 = CARTESIAN_POINT ( 'NONE',  ( -12.39443769393808559, -23.42635292539874214, -32.11001460377168115 ) ) ;
#10359 = CARTESIAN_POINT ( 'NONE',  ( -10.69999999999999929, -130.0000000000000000, -41.24671599790000442 ) ) ;
#10360 = CARTESIAN_POINT ( 'NONE',  ( 9.999999999969999109, -29.12127062269999911, -30.52127062070000107 ) ) ;
#10361 = CARTESIAN_POINT ( 'NONE',  ( -23.52636877871646348, -14.81113159432834081, 225.2882641545094486 ) ) ;
#10362 = CARTESIAN_POINT ( 'NONE',  ( 2.729852257651755210, -4.492922384981882011, -45.81669147672499776 ) ) ;
#10363 = CARTESIAN_POINT ( 'NONE',  ( -27.69999999930000101, 3.392159599999999562E-15, 40.00000000000000000 ) ) ;
#10364 = PLANE ( 'NONE',  #27308 ) ;
#10365 = DIRECTION ( 'NONE',  ( 0.000000000000000000, 0.000000000000000000, -1.000000000000000000 ) ) ;
#10366 = CARTESIAN_POINT ( 'NONE',  ( -19.36389667587700458, -18.53702679572192835, 43.21714158842222986 ) ) ;
#10367 = EDGE_CURVE ( 'NONE', #18124, #17421, #14881, .T. ) ;
#10368 = CARTESIAN_POINT ( 'NONE',  ( -2.100000000000000089, -6.661338147749999512E-16, 226.6412452697800006 ) ) ;
#10369 = ORIENTED_EDGE ( 'NONE', *, *, #13450, .F. ) ;
#10370 = B_SPLINE_CURVE_WITH_KNOTS ( 'NONE', 1,
 ( #21239, #4708 ),
 .UNSPECIFIED., .F., .F.,
 ( 2, 2 ),
 ( -2.557300549769999790E-06, 0.7000000000009999335 ),
 .UNSPECIFIED. ) ;
#10371 = CARTESIAN_POINT ( 'NONE',  ( -2.126050624815288614, 4.685496013473724020, -32.66385571289999490 ) ) ;
#10372 = VERTEX_POINT ( 'NONE', #8076 ) ;
#10373 = EDGE_CURVE ( 'NONE', #28151, #22644, #18253, .T. ) ;
#10374 = CARTESIAN_POINT ( 'NONE',  ( 3.458129700889219116, -0.5397582531354573332, -85.94068374672499999 ) ) ;
#10375 = CARTESIAN_POINT ( 'NONE',  ( -5.473571180597741836, 3.247285761689575168, -50.83267869292499341 ) ) ;
#10376 = EDGE_LOOP ( 'NONE', ( #22640, #23210, #15874, #7781 ) ) ;
#10377 = ORIENTED_EDGE ( 'NONE', *, *, #10080, .F. ) ;
#10378 = DIRECTION ( 'NONE',  ( 0.8660254037843286845, -0.5000000000001905143, 1.975314357840033118E-16 ) ) ;
#10379 = ORIENTED_EDGE ( 'NONE', *, *, #8961, .T. ) ;
#10380 = ORIENTED_EDGE ( 'NONE', *, *, #29638, .F. ) ;
#10381 = DIRECTION ( 'NONE',  ( 0.000000000000000000, 0.9396926207858125046, 0.3420201433259318358 ) ) ;
#10382 = CARTESIAN_POINT ( 'NONE',  ( -17.59696597919420213, 10.20816091468181774, -0.6999999999999784173 ) ) ;
#10383 = DIRECTION ( 'NONE',  ( 1.485828368566968728E-12, 0.9128796883888956604, -0.4082287037029520560 ) ) ;
#10384 = CARTESIAN_POINT ( 'NONE',  ( 3.114464126964767932, 4.033014307823163946, -35.69999999999999574 ) ) ;
#10385 = CARTESIAN_POINT ( 'NONE',  ( -12.60902638016457544, -27.45788211093552889, -22.89113855904373906 ) ) ;
#10386 = CARTESIAN_POINT ( 'NONE',  ( -3.808450222011727782, 1.763428524318019219, -0.6999999999999992895 ) ) ;
#10387 = CARTESIAN_POINT ( 'NONE',  ( -18.95046173579999760, -18.95046173579999760, 115.0000000000000000 ) ) ;
#10388 = LINE ( 'NONE', #21730, #14515 ) ;
#10389 = FACE_OUTER_BOUND ( 'NONE', #7541, .T. ) ;
#10390 = ADVANCED_FACE ( 'NONE', ( #10607 ), #10458, .T. ) ;
#10391 = CARTESIAN_POINT ( 'NONE',  ( 0.7763070146520680836, 4.277613328189620923, -14.02400681850000197 ) ) ;
#10392 = CARTESIAN_POINT ( 'NONE',  ( 2.635706879431563898, 5.544231365240147369, -31.55113063599999990 ) ) ;
#10393 = CARTESIAN_POINT ( 'NONE',  ( 0.5493986535500280377, -27.79508000654526967, 225.9641420709400279 ) ) ;
#10394 = DIRECTION ( 'NONE',  ( -1.000000000000000000, 0.000000000000000000, 0.000000000000000000 ) ) ;
#10395 = CARTESIAN_POINT ( 'NONE',  ( 7.105427357599999217E-15, 8.881784197000000993E-16, 224.6412452697800290 ) ) ;
#10396 = CARTESIAN_POINT ( 'NONE',  ( 24.06826093661917554, -20.50742065831276051, 8.000000000000007105 ) ) ;
#10397 = CARTESIAN_POINT ( 'NONE',  ( -28.45771199730000234, -1.783000543380000178E-14, 229.4982322489999831 ) ) ;
#10398 = DIRECTION ( 'NONE',  ( 0.3633921898465276024, -0.9316362575375355393, 0.000000000000000000 ) ) ;
#10399 = CARTESIAN_POINT ( 'NONE',  ( 9.999999999964241937, -24.59985587209093083, -26.55753809894806494 ) ) ;
#10400 = DIRECTION ( 'NONE',  ( 0.000000000000000000, 0.000000000000000000, 1.000000000000000000 ) ) ;
#10401 = CARTESIAN_POINT ( 'NONE',  ( 1.127732790480000080, -28.47784299079999926, 225.0000014190000002 ) ) ;
#10402 = EDGE_LOOP ( 'NONE', ( #19086, #14949, #19237, #13148 ) ) ;
#10403 = EDGE_CURVE ( 'NONE', #6537, #17588, #17831, .T. ) ;
#10404 = AXIS2_PLACEMENT_3D ( 'NONE', #11270, #20877, #30473 ) ;
#10405 = ADVANCED_FACE ( 'NONE', ( #27747 ), #10760, .T. ) ;
#10406 = DIRECTION ( 'NONE',  ( 0.000000000000000000, -0.3420201433259318913, 0.9396926207858126157 ) ) ;
#10407 = CARTESIAN_POINT ( 'NONE',  ( 10.92440694870000151, 19.99999999999999645, -0.8628532294999990970 ) ) ;
#10408 = EDGE_LOOP ( 'NONE', ( #10817, #4594, #10801, #11312 ) ) ;
#10409 = DIRECTION ( 'NONE',  ( 1.000000000000000000, 0.000000000000000000, 0.000000000000000000 ) ) ;
#10410 = CARTESIAN_POINT ( 'NONE',  ( 7.929582511818026092, -115.3684672989803630, 21.40105740852224159 ) ) ;
#10411 = ORIENTED_EDGE ( 'NONE', *, *, #14851, .F. ) ;
#10412 = CARTESIAN_POINT ( 'NONE',  ( 23.81866167241657806, 14.33570040768432996, 3.899998581000013509 ) ) ;
#10413 = ORIENTED_EDGE ( 'NONE', *, *, #30113, .F. ) ;
#10414 = ORIENTED_EDGE ( 'NONE', *, *, #25796, .F. ) ;
#10415 = ADVANCED_FACE ( 'NONE', ( #3210 ), #30531, .T. ) ;
#10416 = SURFACE_STYLE_FILL_AREA ( #27241 ) ;
#10417 = VERTEX_POINT ( 'NONE', #18464 ) ;
#10418 = DIRECTION ( 'NONE',  ( 0.000000000000000000, 0.000000000000000000, 1.000000000000000000 ) ) ;
#10419 = CARTESIAN_POINT ( 'NONE',  ( 8.700000000248305554, -25.92947359976189503, -31.20249410819006286 ) ) ;
#10420 = LINE ( 'NONE', #29757, #6191 ) ;
#10421 = CARTESIAN_POINT ( 'NONE',  ( 8.700000000248305554, -25.92947359976189503, -31.20249410819006286 ) ) ;
#10422 = DIRECTION ( 'NONE',  ( 0.000000000000000000, 0.000000000000000000, -1.000000000000000000 ) ) ;
#10423 = PRODUCT_DEFINITION_SHAPE ( 'NONE', 'NONE',  #31125 ) ;
#10424 = CARTESIAN_POINT ( 'NONE',  ( -24.35329726287045915, -13.40752173053085983, 5.289304314274809293 ) ) ;
#10425 = EDGE_CURVE ( 'NONE', #9871, #12600, #28529, .T. ) ;
#10426 = CARTESIAN_POINT ( 'NONE',  ( 4.684462318791906554, -27.09927246286415325, 209.5983106348512877 ) ) ;
#10427 = CARTESIAN_POINT ( 'NONE',  ( 23.50666810109999716, -14.84174128299999929, 225.0000014190000002 ) ) ;
#10428 = VERTEX_POINT ( 'NONE', #6659 ) ;
#10429 = CARTESIAN_POINT ( 'NONE',  ( 3.950106903291103588, 1.853988655799144958, -2.479170051700008148 ) ) ;
#10430 = CARTESIAN_POINT ( 'NONE',  ( 4.129834804009608007, 5.047645050193429128, -20.25622222230000347 ) ) ;
#10431 = CARTESIAN_POINT ( 'NONE',  ( -25.43121960300666373, -8.635379644106540908, 193.2171415880000040 ) ) ;
#10432 = AXIS2_PLACEMENT_3D ( 'NONE', #2801, #7366, #9574 ) ;
#10433 = LINE ( 'NONE', #15605, #1451 ) ;
#10434 = CARTESIAN_POINT ( 'NONE',  ( 23.81569860410000317, -13.75000000000000000, 226.0999999999999943 ) ) ;
#10435 = CARTESIAN_POINT ( 'NONE',  ( -25.05382009470000071, 13.89803701039999950, 230.2432540810000319 ) ) ;
#10436 = CARTESIAN_POINT ( 'NONE',  ( -23.26185891368683301, -14.66761890392226242, 224.7132485884542064 ) ) ;
#10437 = EDGE_CURVE ( 'NONE', #5736, #15510, #9229, .T. ) ;
#10438 = CARTESIAN_POINT ( 'NONE',  ( -1.335589246056437140, 3.267430459342669735, -0.6999999999999783062 ) ) ;
#10439 = CARTESIAN_POINT ( 'NONE',  ( 27.53132592989999949, 4.649109393739999874, 229.7313259299999686 ) ) ;
#10440 = CARTESIAN_POINT ( 'NONE',  ( 23.24663841807413434, -14.69162354064478215, 224.9035402886169095 ) ) ;
#10441 = ORIENTED_EDGE ( 'NONE', *, *, #30400, .F. ) ;
#10442 = CARTESIAN_POINT ( 'NONE',  ( -0.9606962270921419744, -4.447130805931738706, -55.53033560642500532 ) ) ;
#10443 = DIRECTION ( 'NONE',  ( 1.000000000000000000, 0.000000000000000000, 0.000000000000000000 ) ) ;
#10444 = CARTESIAN_POINT ( 'NONE',  ( -3.117834729128555971, -4.866792379758847709, -18.70544088820000184 ) ) ;
#10445 = CARTESIAN_POINT ( 'NONE',  ( -22.97593529893700648, 15.65128280014837081, 8.000000000000007105 ) ) ;
#10446 = CARTESIAN_POINT ( 'NONE',  ( -4.291194574663122374, 1.061632286161843020, -68.10000000002500542 ) ) ;
#10447 = EDGE_LOOP ( 'NONE', ( #7176, #14850, #9432, #14639 ) ) ;
#10448 = VERTEX_POINT ( 'NONE', #30593 ) ;
#10449 = AXIS2_PLACEMENT_3D ( 'NONE', #675, #15286, #7732 ) ;
#10450 = CARTESIAN_POINT ( 'NONE',  ( -1.670339710860670568, -0.1901198163082873371, -97.93793859254537892 ) ) ;
#10451 = SURFACE_SIDE_STYLE ('',( #15325 ) ) ;
#10452 = ORIENTED_EDGE ( 'NONE', *, *, #579, .T. ) ;
#10453 = CARTESIAN_POINT ( 'NONE',  ( -24.93720648713954446, 13.79881813474513486, 3.899998581000013509 ) ) ;
#10454 = VECTOR ( 'NONE', #21577, 1000.000000000000000 ) ;
#10455 = DIRECTION ( 'NONE',  ( 0.000000000000000000, -1.000000000000000000, 0.000000000000000000 ) ) ;
#10456 = ORIENTED_EDGE ( 'NONE', *, *, #5209, .T. ) ;
#10457 = CARTESIAN_POINT ( 'NONE',  ( 3.415065912822992988, 4.318092861595879128, -62.83768011632499650 ) ) ;
#10458 = PLANE ( 'NONE',  #381 ) ;
#10459 = MANIFOLD_SOLID_BREP ( 'PartBody', #29636 ) ;
#10460 = CARTESIAN_POINT ( 'NONE',  ( -24.50110440319828342, 13.37667737394870748, -0.6577119969999878357 ) ) ;
#10461 = ADVANCED_FACE ( 'NONE', ( #11854 ), #4313, .T. ) ;
#10462 = CARTESIAN_POINT ( 'NONE',  ( -28.50002393070000295, -2.434994504239999635, 222.0000000000000000 ) ) ;
#10463 = LINE ( 'NONE', #5574, #19951 ) ;
#10464 = CARTESIAN_POINT ( 'NONE',  ( -7.999999999628359504, -14.95611408987656965, -40.37595097054163773 ) ) ;
#10465 = CIRCLE ( 'NONE', #28046, 1.926829268289999231 ) ;
#10466 = ORIENTED_EDGE ( 'NONE', *, *, #22013, .T. ) ;
#10467 = EDGE_CURVE ( 'NONE', #5252, #3651, #26333, .T. ) ;
#10468 = CARTESIAN_POINT ( 'NONE',  ( 13.67718073920000066, 21.70000000000000284, -57.16242423349999768 ) ) ;
#10469 = ADVANCED_FACE ( 'NONE', ( #4781 ), #23824, .F. ) ;
#10470 = EDGE_CURVE ( 'NONE', #20819, #20463, #24975, .T. ) ;
#10471 = DIRECTION ( 'NONE',  ( 1.000000000000000000, 0.000000000000000000, 0.000000000000000000 ) ) ;
#10472 = ORIENTED_EDGE ( 'NONE', *, *, #2315, .T. ) ;
#10473 = CARTESIAN_POINT ( 'NONE',  ( 3.484101657956257370, 0.9653352590934711763, 227.7128614111574052 ) ) ;
#10474 = CARTESIAN_POINT ( 'NONE',  ( -22.63992238019999803, -14.34133587289999845, 5.000000000000000000 ) ) ;
#10475 = CARTESIAN_POINT ( 'NONE',  ( -24.40022624598054435, -14.72688605908970239, 6.099998581000020792 ) ) ;
#10476 = CARTESIAN_POINT ( 'NONE',  ( -24.36725163762957536, -13.38201776503690432, 4.926540930971143872 ) ) ;
#10477 = CARTESIAN_POINT ( 'NONE',  ( -23.24667624907491259, -14.69156368041574723, 4.854326830129346071 ) ) ;
#10478 = CARTESIAN_POINT ( 'NONE',  ( -1.111489881331200413, -3.601265787235460536, -0.6999999999999994005 ) ) ;
#10479 = VECTOR ( 'NONE', #13479, 1000.000000000000114 ) ;
#10480 = CARTESIAN_POINT ( 'NONE',  ( -26.66783967069105898, -7.507193849635574345, -0.6999999999999784173 ) ) ;
#10481 = DIRECTION ( 'NONE',  ( 0.000000000000000000, 0.3420201433259318358, -0.9396926207858125046 ) ) ;
#10482 = ORIENTED_EDGE ( 'NONE', *, *, #23096, .F. ) ;
#10483 =( LENGTH_UNIT ( ) NAMED_UNIT ( * ) SI_UNIT ( .MILLI., .METRE. ) );
#10484 = DIRECTION ( 'NONE',  ( 0.000000000000000000, 0.000000000000000000, -1.000000000000000000 ) ) ;
#10485 = CARTESIAN_POINT ( 'NONE',  ( -26.84464184930000030, 3.287411897469999975E-15, 87.43750406049998958 ) ) ;
#10486 = CARTESIAN_POINT ( 'NONE',  ( 0.4200715327254807008, -3.971614891497597277, -68.10000000002499121 ) ) ;
#10487 = ORIENTED_EDGE ( 'NONE', *, *, #10355, .F. ) ;
#10488 = DIRECTION ( 'NONE',  ( -1.224606353819999829E-16, -1.000000000000000000, 0.000000000000000000 ) ) ;
#10489 = B_SPLINE_CURVE_WITH_KNOTS ( 'NONE', 3,
 ( #26301, #14191, #4437, #11362, #9460, #20960, #7105, #30566, #16690, #28190 ),
 .UNSPECIFIED., .F., .F.,
 ( 4, 2, 2, 2, 4 ),
 ( 0.000000000000000000, 0.2500000000000000000, 0.5000000000000000000, 0.7500000000000000000, 1.000000000000000000 ),
 .UNSPECIFIED. ) ;
#10490 = CARTESIAN_POINT ( 'NONE',  ( -8.000000000050000892, -13.30122639390952877, -75.84793558053411289 ) ) ;
#10491 = CARTESIAN_POINT ( 'NONE',  ( 9.499999999998065547, -18.19953924290990344, -36.00725302081955448 ) ) ;
#10492 = CARTESIAN_POINT ( 'NONE',  ( -1.377718196578040954, -5.677888627607300620, -62.74311227092501753 ) ) ;
#10493 = ORIENTED_EDGE ( 'NONE', *, *, #16998, .F. ) ;
#10494 = EDGE_LOOP ( 'NONE', ( #19908, #23815, #3942, #29074 ) ) ;
#10496 = CARTESIAN_POINT ( 'NONE',  ( 8.000000000281882961, -22.83323352251018079, -39.84673050074155753 ) ) ;
#10495 = CONICAL_SURFACE ( 'NONE', #2970, 3.491271820449999286, 1.047197551199999799 ) ;
#10497 = ORIENTED_EDGE ( 'NONE', *, *, #1586, .F. ) ;
#10498 = ORIENTED_EDGE ( 'NONE', *, *, #25956, .F. ) ;
#10499 = CARTESIAN_POINT ( 'NONE',  ( -10.96000317937597757, 21.69999999997520845, -55.08353444139804367 ) ) ;
#10500 = CARTESIAN_POINT ( 'NONE',  ( -12.29999999969999891, -30.00000000000000000, -28.40000000020000215 ) ) ;
#10501 = CARTESIAN_POINT ( 'NONE',  ( -9.999999999969999109, -29.12127062080000073, -30.52127062269999769 ) ) ;
#10502 = CARTESIAN_POINT ( 'NONE',  ( -17.31926949172594377, -26.03170168038248633, -33.61445539661270487 ) ) ;
#10503 = CARTESIAN_POINT ( 'NONE',  ( 8.700000000270996736, -18.23122067931645773, -34.51216076560373125 ) ) ;
#10504 = EDGE_CURVE ( 'NONE', #3911, #3826, #7591, .T. ) ;
#10505 = CARTESIAN_POINT ( 'NONE',  ( -1.087696845100000198, -27.77899371300000197, 224.7918862260000026 ) ) ;
#10506 = ORIENTED_EDGE ( 'NONE', *, *, #19533, .F. ) ;
#10507 = CARTESIAN_POINT ( 'NONE',  ( 2.876144609715792111, -3.506551327605733182, -44.10000000002499121 ) ) ;
#10508 = CARTESIAN_POINT ( 'NONE',  ( 24.96253706050071131, 13.75225324050492581, 4.689458287000014991 ) ) ;
#10509 = AXIS2_PLACEMENT_3D ( 'NONE', #18512, #28114, #16460 ) ;
#10510 = CARTESIAN_POINT ( 'NONE',  ( -2.496099253731141943, 5.577352528212363048, -23.33780126170000102 ) ) ;
#10511 = CARTESIAN_POINT ( 'NONE',  ( -28.50000000000000000, 3.490128108389999698E-15, 190.0000000000000000 ) ) ;
#10512 = CARTESIAN_POINT ( 'NONE',  ( 12.12499541220000054, 20.99999999999999645, -55.73512219869999740 ) ) ;
#10513 = CARTESIAN_POINT ( 'NONE',  ( 23.25788685383077592, -13.43083806724684948, 86.78285841136666079 ) ) ;
#10514 = CARTESIAN_POINT ( 'NONE',  ( 8.700000000273361067, -18.09728189817007404, -34.21264730247137464 ) ) ;
#10515 = CARTESIAN_POINT ( 'NONE',  ( -3.362912017748242999, 4.936852587875802278, -48.05391720692499291 ) ) ;
#10516 = AXIS2_PLACEMENT_3D ( 'NONE', #18427, #6470, #16072 ) ;
#10517 = CARTESIAN_POINT ( 'NONE',  ( -17.72973609203700462, 11.65373091001462669, -1.400000000000002132 ) ) ;
#10518 = CARTESIAN_POINT ( 'NONE',  ( 4.679341198149911563, -26.38945575071662830, 209.5097050137637211 ) ) ;
#10519 = CARTESIAN_POINT ( 'NONE',  ( -18.02784043102035483, 19.99990957752277509, 230.6954974467259376 ) ) ;
#10520 = CARTESIAN_POINT ( 'NONE',  ( -26.62724484483073439, -3.508068424025491794, 43.21714158835001030 ) ) ;
#10521 = VECTOR ( 'NONE', #28832, 1000.000000000000000 ) ;
#10522 = B_SPLINE_CURVE_WITH_KNOTS ( 'NONE', 3,
 ( #28477, #4564, #23772, #18012, #24958, #15507, #25593, #1201, #25438, #17856, #22751, #27619, #29979, #6066, #10795, #20392, #29678, #5905, #22916, #8413, #15982, #13624, #4026, #3389, #20706, #897 ),
 .UNSPECIFIED., .F., .F.,
 ( 4, 2, 2, 1, 1, 2, 2, 2, 2, 2, 1, 1, 2, 2, 4 ),
 ( 0.000000000000000000, 0.1250000000000019984, 0.1875000000000023870, 0.2187500000000025813, 0.2343750000000010547, 0.2421875000000009992, 0.2500000000000009437, 0.4999999999999972244, 0.6249999999999953371, 0.6874999999999943379, 0.7187499999999937828, 0.7343749999999954481, 0.7421874999999953371, 0.7499999999999952260, 1.000000000000000000 ),
 .UNSPECIFIED. ) ;
#10523 = CARTESIAN_POINT ( 'NONE',  ( 7.297190580108170899, -25.78810378223603195, 22.11652997304829427 ) ) ;
#10524 = ORIENTED_EDGE ( 'NONE', *, *, #14963, .F. ) ;
#10525 = CARTESIAN_POINT ( 'NONE',  ( -4.976668802704899086, 3.592974922927941073, -35.06696136360000793 ) ) ;
#10526 = EDGE_LOOP ( 'NONE', ( #2669, #20274, #15308, #17708, #8144, #23682, #16629, #20660 ) ) ;
#10527 = CARTESIAN_POINT ( 'NONE',  ( 0.000000000000000000, 0.000000000000000000, -44.00000000000000000 ) ) ;
#10528 = CARTESIAN_POINT ( 'NONE',  ( -0.9881560945370695404, 5.823346091562972227, -51.73792092402499776 ) ) ;
#10529 = VERTEX_POINT ( 'NONE', #4924 ) ;
#10530 = EDGE_CURVE ( 'NONE', #20819, #21014, #5874, .T. ) ;
#10531 = ORIENTED_EDGE ( 'NONE', *, *, #26909, .F. ) ;
#10532 = DIRECTION ( 'NONE',  ( -0.8660254037843290176, -0.5000000000001898481, -2.222961732812015412E-16 ) ) ;
#10533 = EDGE_LOOP ( 'NONE', ( #6020, #4459, #937, #14260 ) ) ;
#10534 = ORIENTED_EDGE ( 'NONE', *, *, #10220, .F. ) ;
#10535 = CARTESIAN_POINT ( 'NONE',  ( 24.92639507930385889, 13.81781707913292934, 4.493023686000019445 ) ) ;
#10536 = CARTESIAN_POINT ( 'NONE',  ( -0.5944614084144663746, -27.79380475670850359, 5.146930914275719360 ) ) ;
#10537 = CARTESIAN_POINT ( 'NONE',  ( 3.944225552621728692, 3.331202856656692468, -35.69999999999999574 ) ) ;
#10538 = VECTOR ( 'NONE', #4189, 1000.000000000000114 ) ;
#10539 = CIRCLE ( 'NONE', #28127, 4.276011752367109509 ) ;
#10540 = DIRECTION ( 'NONE',  ( -0.9880370573969197157, 0.1542166437529879364, 0.000000000000000000 ) ) ;
#10541 = CARTESIAN_POINT ( 'NONE',  ( 2.131628207279999844E-14, -5.329070518200000398E-15, 86.78285841159998881 ) ) ;
#10542 = CARTESIAN_POINT ( 'NONE',  ( -3.930544418528015616, 0.9096215242735280482, -0.6999999999999994005 ) ) ;
#10543 = CARTESIAN_POINT ( 'NONE',  ( -13.00000000000000000, 22.40709319595134730, -62.85117013414870257 ) ) ;
#10544 = CARTESIAN_POINT ( 'NONE',  ( 10.69999999997381757, -28.84240556167032921, -30.80012576576890027 ) ) ;
#10545 = DIRECTION ( 'NONE',  ( 0.000000000000000000, 1.000000000000000000, 0.000000000000000000 ) ) ;
#10546 = CARTESIAN_POINT ( 'NONE',  ( -2.929853409778804263, 3.622264489389750874, -13.60352819869999763 ) ) ;
#10547 = CARTESIAN_POINT ( 'NONE',  ( 3.503437880484509659, 2.636891074944046398, -32.36032172559999509 ) ) ;
#10548 = CLOSED_SHELL ( 'NONE', ( #30068, #6474, #371, #28541, #9891, #21421, #18484, #24036, #29673, #18128, #3284, #23948, #26632, #11529, #27790, #22620, #8255, #25460, #9559, #19833, #30796, #28487, #18915, #9327, #22918, #9143, #14247, #23266, #13454, #10820, #20664, #24112, #11737, #16128, #21622, #19009, #1575, #22860, #5418, #3428, #4328, #22025, #27322, #13118, #5444, #21959, #11040, #29435, #1404, #14989, #23433, #2967, #3967, #8930, #20726, #7683, #4668, #5357, #24928, #4442, #26348, #15412, #15200, #615, #8374, #6507, #27723, #8848, #7861 ) ) ;
#10549 = EDGE_CURVE ( 'NONE', #5834, #27894, #14533, .T. ) ;
#10550 = CARTESIAN_POINT ( 'NONE',  ( 4.874695217780000256, -3.326860129179999959, 226.6412452697800006 ) ) ;
#10551 = CARTESIAN_POINT ( 'NONE',  ( 17.83931306984926835, 20.00000000000176570, 0.000000000000000000 ) ) ;
#10552 = CARTESIAN_POINT ( 'NONE',  ( -7.861312627757861549, -7.262254661959269164, -37.27493672744613207 ) ) ;
#10553 = CARTESIAN_POINT ( 'NONE',  ( 27.79539923781684507, 0.5057481689249130330, 1.000000000000000888 ) ) ;
#10554 = DIRECTION ( 'NONE',  ( -0.000000000000000000, 1.000000000000000000, -2.257145581549999994E-12 ) ) ;
#10555 = FACE_OUTER_BOUND ( 'NONE', #30425, .T. ) ;
#10556 = FACE_OUTER_BOUND ( 'NONE', #6643, .T. ) ;
#10557 = LINE ( 'NONE', #20151, #21338 ) ;
#10558 = ORIENTED_EDGE ( 'NONE', *, *, #6513, .F. ) ;
#10559 = LINE ( 'NONE', #29745, #30374 ) ;
#10560 = DIRECTION ( 'NONE',  ( 0.3633921898465289901, 0.9316362575375348731, -8.673617379884029161E-15 ) ) ;
#10561 = EDGE_LOOP ( 'NONE', ( #297, #21177, #15841, #6612 ) ) ;
#10562 = CARTESIAN_POINT ( 'NONE',  ( 0.000000000000000000, 20.99999999999999645, -44.10000000017154065 ) ) ;
#10563 = DIRECTION ( 'NONE',  ( 1.000000000000000000, 0.000000000000000000, 0.000000000000000000 ) ) ;
#10564 = ORIENTED_EDGE ( 'NONE', *, *, #17527, .T. ) ;
#10565 = CARTESIAN_POINT ( 'NONE',  ( -4.684462318791891455, -27.09927246286417102, 20.40168936514870168 ) ) ;
#10566 = EDGE_LOOP ( 'NONE', ( #6145, #30696, #8416, #14112, #206, #10879, #30148 ) ) ;
#10567 = ADVANCED_FACE ( 'NONE', ( #28685 ), #375, .F. ) ;
#10568 = VERTEX_POINT ( 'NONE', #16715 ) ;
#10569 =( NAMED_UNIT ( * ) PLANE_ANGLE_UNIT ( ) SI_UNIT ( $, .RADIAN. ) );
#10570 = ORIENTED_EDGE ( 'NONE', *, *, #21058, .T. ) ;
#10571 = CARTESIAN_POINT ( 'NONE',  ( 16.62864107308872264, -9.970561443424061920, -0.000000000000000000 ) ) ;
#10572 = CARTESIAN_POINT ( 'NONE',  ( -17.93062603662948717, -9.163977451850843892, -0.6999999999999784173 ) ) ;
#10573 = CARTESIAN_POINT ( 'NONE',  ( -7.999999999652525950, -17.05009613497038146, -37.77893181949669099 ) ) ;
#10574 = FILL_AREA_STYLE ('',( #984 ) ) ;
#10575 = CARTESIAN_POINT ( 'NONE',  ( -20.30396346370000060, 20.00000000000000000, 227.3999999999999773 ) ) ;
#10576 = CARTESIAN_POINT ( 'NONE',  ( 0.1352650258152492124, -28.50015511220863118, 6.042326290000010758 ) ) ;
#10577 = CARTESIAN_POINT ( 'NONE',  ( -7.439629836182230171, -5.610939228782946486, -27.11239056199590536 ) ) ;
#10578 = CARTESIAN_POINT ( 'NONE',  ( 23.50666810109999716, -14.84174128299999929, 224.8958160969999938 ) ) ;
#10579 = EDGE_CURVE ( 'NONE', #18294, #25078, #29998, .T. ) ;
#10580 = ADVANCED_FACE ( 'NONE', ( #26637 ), #20984, .T. ) ;
#10581 = CARTESIAN_POINT ( 'NONE',  ( 1.699015317690025118, 6.330513620609809600, -2.653410702900004026 ) ) ;
#10582 = CARTESIAN_POINT ( 'NONE',  ( 1.602378319964792297, -5.640493390528545703, -20.29535708920000658 ) ) ;
#10583 = DIRECTION ( 'NONE',  ( 0.000000000000000000, 0.000000000000000000, 1.000000000000000000 ) ) ;
#10584 = CARTESIAN_POINT ( 'NONE',  ( -1.099928585426612759, -27.47799405182390231, 5.145501061710134216 ) ) ;
#10585 = CARTESIAN_POINT ( 'NONE',  ( -1.595582016994381069, -3.092641108896711177, -90.29857220542305640 ) ) ;
#10586 = CARTESIAN_POINT ( 'NONE',  ( -28.35924375240000117, 4.781805056509999652, 229.7625741969999922 ) ) ;
#10587 = CARTESIAN_POINT ( 'NONE',  ( 10.69999999996523243, -41.43508060205707721, -26.99581415663967121 ) ) ;
#10588 = EDGE_CURVE ( 'NONE', #16422, #16790, #17638, .T. ) ;
#10589 = FACE_BOUND ( 'NONE', #27978, .T. ) ;
#10590 = CARTESIAN_POINT ( 'NONE',  ( -9.014669513459999450, -25.43090265169999853, 230.6999999999999886 ) ) ;
#10591 = CARTESIAN_POINT ( 'NONE',  ( 10.89131017139999891, -24.73114799890000270, -1.811764705899998606 ) ) ;
#10592 = VERTEX_POINT ( 'NONE', #12616 ) ;
#10593 = CARTESIAN_POINT ( 'NONE',  ( -3.735326252960651239, -2.773461810559843421, -55.52895058492500624 ) ) ;
#10594 = CARTESIAN_POINT ( 'NONE',  ( -12.75378086759999796, -27.00000000059169736, -22.62649730796000114 ) ) ;
#10595 = CARTESIAN_POINT ( 'NONE',  ( -4.262638389374871828, -3.164596713843205400, -0.8737437981000060194 ) ) ;
#10596 = CARTESIAN_POINT ( 'NONE',  ( -27.79539923781770128, -0.5057481688779147389, 8.000000000000007105 ) ) ;
#10597 = EDGE_CURVE ( 'NONE', #11027, #26158, #8345, .T. ) ;
#10598 = CARTESIAN_POINT ( 'NONE',  ( -4.210742777790425606, 0.6064333458413161404, -68.10000000002500542 ) ) ;
#10599 = VERTEX_POINT ( 'NONE', #20321 ) ;
#10600 = ORIENTED_EDGE ( 'NONE', *, *, #8259, .F. ) ;
#10601 = CARTESIAN_POINT ( 'NONE',  ( -3.513873398455594987, 0.1826188577267222057, -94.01209571138487320 ) ) ;
#10602 = ORIENTED_EDGE ( 'NONE', *, *, #5994, .T. ) ;
#10603 = CARTESIAN_POINT ( 'NONE',  ( -24.37165444408190851, 14.77472139917419369, 4.895781291000017355 ) ) ;
#10604 = DIRECTION ( 'NONE',  ( -0.9316362575375349842, 0.3633921898465292122, -0.000000000000000000 ) ) ;
#10605 = CARTESIAN_POINT ( 'NONE',  ( 3.051761028451055680, 3.858721280585067248, -62.88768011632500077 ) ) ;
#10606 = EDGE_CURVE ( 'NONE', #3709, #6569, #9629, .T. ) ;
#10607 = FACE_OUTER_BOUND ( 'NONE', #4300, .T. ) ;
#10608 = VECTOR ( 'NONE', #1192, 1000.000000000000000 ) ;
#10609 = CARTESIAN_POINT ( 'NONE',  ( -25.54177752991350303, 13.94484553950296934, 0.5017677510000262409 ) ) ;
#10610 = CARTESIAN_POINT ( 'NONE',  ( -27.54633509470000163, -4.750421057000000502, 222.0000000000000000 ) ) ;
#10611 = CARTESIAN_POINT ( 'NONE',  ( -27.92857142909999979, 3.420150602519999655E-15, 192.0603150150000147 ) ) ;
#10612 = PLANE ( 'NONE',  #28561 ) ;
#10613 = EDGE_LOOP ( 'NONE', ( #18923, #9595, #9671, #19163, #16218, #6852, #7657, #19963, #25221, #5424, #6572, #31044, #26745, #3756, #1781, #30099, #28963 ) ) ;
#10614 = PRODUCT_DEFINITION_CONTEXT ( 'detailed design', #28867, 'design' ) ;
#10615 = CARTESIAN_POINT ( 'NONE',  ( 24.39135169767337885, -14.74223403355047068, 4.689353541000001790 ) ) ;
#10616 = EDGE_CURVE ( 'NONE', #23233, #14792, #5689, .T. ) ;
#10617 = DIRECTION ( 'NONE',  ( 2.764840495839172918E-12, 0.9128796883888953273, -0.4082287037029530552 ) ) ;
#10618 = ORIENTED_EDGE ( 'NONE', *, *, #1632, .T. ) ;
#10619 = CARTESIAN_POINT ( 'NONE',  ( -10.69999999999999929, -29.30501631370000482, -26.47986984990000181 ) ) ;
#10620 = CARTESIAN_POINT ( 'NONE',  ( 16.04656078597520974, 10.97998838177520931, -1.452769935612311825 ) ) ;
#10621 = CARTESIAN_POINT ( 'NONE',  ( -23.69119896570000350, -20.94188573499999961, 222.0000000000000000 ) ) ;
#10622 = CARTESIAN_POINT ( 'NONE',  ( 17.83931306984926835, 20.00000000000176570, 0.000000000000000000 ) ) ;
#10623 = CARTESIAN_POINT ( 'NONE',  ( 16.06941601916650342, -9.166288768300725920, 0.000000000000000000 ) ) ;
#10624 = CARTESIAN_POINT ( 'NONE',  ( -1.580768150575516229, -3.412369166365430306, -0.6999999999999994005 ) ) ;
#10625 = CARTESIAN_POINT ( 'NONE',  ( -10.49243769149999927, -24.66097101990000340, -1.192453596599994725 ) ) ;
#10626 = DIRECTION ( 'NONE',  ( 0.9316362575375356503, 0.3633921898465274913, 0.000000000000000000 ) ) ;
#10627 = ORIENTED_EDGE ( 'NONE', *, *, #11105, .T. ) ;
#10628 = FACE_OUTER_BOUND ( 'NONE', #16360, .T. ) ;
#10629 = CARTESIAN_POINT ( 'NONE',  ( -7.999999999681657314, -14.84794678168725568, -33.28653323038288647 ) ) ;
#10630 = VECTOR ( 'NONE', #4440, 1000.000000000000114 ) ;
#10631 = CARTESIAN_POINT ( 'NONE',  ( -25.51870711004141157, -8.199261060474288598, 93.21714158836661568 ) ) ;
#10632 = DIRECTION ( 'NONE',  ( 0.7071067811865475727, -0.7071067811865475727, 0.000000000000000000 ) ) ;
#10633 = ADVANCED_FACE ( 'NONE', ( #24899 ), #354, .F. ) ;
#10634 = B_SPLINE_CURVE_WITH_KNOTS ( 'NONE', 5,
 ( #15751, #28023, #30078, #16223, #20475, #3633, #27705, #23002, #4275, #30403, #1450, #18584 ),
 .UNSPECIFIED., .F., .F.,
 ( 6, 3, 3, 6 ),
 ( 3.339306056729999916, 4.810258468379999819, 6.613963844790000657, 6.678484291160000197 ),
 .UNSPECIFIED. ) ;
#10635 = CARTESIAN_POINT ( 'NONE',  ( 11.48163258689999999, -24.28840541759999994, -1.419991652300001128 ) ) ;
#10636 = EDGE_CURVE ( 'NONE', #17371, #11462, #29759, .T. ) ;
#10637 =( LENGTH_UNIT ( ) NAMED_UNIT ( * ) SI_UNIT ( .MILLI., .METRE. ) );
#10638 = CARTESIAN_POINT ( 'NONE',  ( 0.000000000000000000, 0.000000000000000000, 115.0000000000000000 ) ) ;
#10639 = DIRECTION ( 'NONE',  ( 1.000000000000000000, 0.000000000000000000, 0.000000000000000000 ) ) ;
#10640 = CARTESIAN_POINT ( 'NONE',  ( -1.078772944755383767, 5.890544393200768170, -60.73324387862499663 ) ) ;
#10641 = ORIENTED_EDGE ( 'NONE', *, *, #25615, .T. ) ;
#10642 = CARTESIAN_POINT ( 'NONE',  ( 19.88997495436197482, 20.00029480896879974, 229.9620880754783911 ) ) ;
#10643 = EDGE_LOOP ( 'NONE', ( #9191, #27901, #12767, #3759, #23413, #21149, #10369, #8941, #6341, #5138, #25038, #13599, #7878, #29289, #13434, #11959, #30221, #8036, #27168, #28675, #7358, #24948, #28667, #13028, #23509, #8857, #19786, #22933, #6941, #21923, #24880, #23462, #7116, #31034, #3565, #17450, #16137, #30969, #28567, #2768, #25441, #29516, #1857, #1004 ) ) ;
#10644 = CARTESIAN_POINT ( 'NONE',  ( -4.575152268165027181, -30.31846920187740224, 0.08279701300001329756 ) ) ;
#10645 = ORIENTED_EDGE ( 'NONE', *, *, #3399, .F. ) ;
#10646 = DIRECTION ( 'NONE',  ( -1.000000000000000000, 5.687697958343395332E-16, -6.771501495045879231E-12 ) ) ;
#10647 = CARTESIAN_POINT ( 'NONE',  ( 25.35851007746311581, -13.00862288856444238, 4.319165765000021473 ) ) ;
#10648 = CARTESIAN_POINT ( 'NONE',  ( -19.80535357367646654, 19.50875577052770993, 1.000000000000000888 ) ) ;
#10649 = VECTOR ( 'NONE', #24413, 1000.000000000000000 ) ;
#10650 = FACE_OUTER_BOUND ( 'NONE', #13584, .T. ) ;
#10651 = CARTESIAN_POINT ( 'NONE',  ( 25.32653163311281830, -13.07087917458821202, 5.760266709000011254 ) ) ;
#10652 = CARTESIAN_POINT ( 'NONE',  ( -0.03443693864410000277, -27.80022362959999782, 223.9000014189999774 ) ) ;
#10653 = EDGE_LOOP ( 'NONE', ( #26587, #26440, #2451, #8270 ) ) ;
#10654 = CARTESIAN_POINT ( 'NONE',  ( 2.815684575957060343, -3.695535399317911196, -44.10000000002499121 ) ) ;
#10655 = CARTESIAN_POINT ( 'NONE',  ( 22.97559295455008765, 15.65128684778802715, 8.000000000000007105 ) ) ;
#10656 = CARTESIAN_POINT ( 'NONE',  ( 1.265035515811500089, -4.453021097817299712, -21.79535708920000658 ) ) ;
#10657 = CARTESIAN_POINT ( 'NONE',  ( 23.60764285305539545, -12.68553248495022423, 4.262772992568688579 ) ) ;
#10658 = MANIFOLD_SOLID_BREP ( 'PartBody', #25633 ) ;
#10659 = CARTESIAN_POINT ( 'NONE',  ( 8.000000000000000000, -17.05999687705277879, -77.21601615383784178 ) ) ;
#10660 = CARTESIAN_POINT ( 'NONE',  ( 26.80000000069999899, -3.281945028320000125E-15, 86.78285841090000474 ) ) ;
#10661 = CARTESIAN_POINT ( 'NONE',  ( -23.51084008381386070, -14.83576737699261727, 225.1458431688038218 ) ) ;
#10662 = CARTESIAN_POINT ( 'NONE',  ( 5.461196134307610528, -0.8102654170096962316, -45.33818262062500537 ) ) ;
#10663 = DIRECTION ( 'NONE',  ( -0.000000000000000000, 1.000000000000000000, -2.257145581549999994E-12 ) ) ;
#10664 = DIRECTION ( 'NONE',  ( 3.133604487004501912E-12, 0.3568421334038983650, -0.9341647027306021478 ) ) ;
#10665 = CARTESIAN_POINT ( 'NONE',  ( -18.59970865813222218, 20.00000695728539668, 230.6210579144432984 ) ) ;
#10666 = CARTESIAN_POINT ( 'NONE',  ( -27.79999999980000069, 4.687507935210000198, 229.1414213560000235 ) ) ;
#10667 = VECTOR ( 'NONE', #229, 1000.000000000000114 ) ;
#10668 = CARTESIAN_POINT ( 'NONE',  ( 7.107063564515522458, -25.84129680694968911, 21.94110913170587551 ) ) ;
#10669 = VERTEX_POINT ( 'NONE', #8822 ) ;
#10670 = CARTESIAN_POINT ( 'NONE',  ( 0.07512830594656044747, -4.346272141329931671, -33.41110030499999795 ) ) ;
#10671 = ADVANCED_FACE ( 'NONE', ( #30401 ), #22490, .F. ) ;
#10672 = ORIENTED_EDGE ( 'NONE', *, *, #26962, .T. ) ;
#10673 = CARTESIAN_POINT ( 'NONE',  ( 13.12132034340000075, 21.69999999990000106, -69.22132034359999864 ) ) ;
#10674 = CARTESIAN_POINT ( 'NONE',  ( -3.347225659292417888, -3.617661372292495514, -50.94612412472498875 ) ) ;
#10675 = ORIENTED_EDGE ( 'NONE', *, *, #19830, .F. ) ;
#10676 = VERTEX_POINT ( 'NONE', #21260 ) ;
#10677 = CONTEXT_DEPENDENT_SHAPE_REPRESENTATION ( #5565, #17686 ) ;
#10678 = EDGE_LOOP ( 'NONE', ( #3398, #26715, #25842, #12538, #28913 ) ) ;
#10679 = ORIENTED_EDGE ( 'NONE', *, *, #20847, .T. ) ;
#10680 = CARTESIAN_POINT ( 'NONE',  ( 24.41841038956698640, 14.69667349781389376, 3.899998581000013509 ) ) ;
#10681 = FACE_BOUND ( 'NONE', #7049, .T. ) ;
#10682 = CARTESIAN_POINT ( 'NONE',  ( 2.910383045670000247E-11, 21.70000000000000284, -64.10000000000000853 ) ) ;
#10683 = CARTESIAN_POINT ( 'NONE',  ( -27.71261514784184499, -0.5042418799608719970, 0.5514269430000329208 ) ) ;
#10684 = CARTESIAN_POINT ( 'NONE',  ( -1.087565149828547018, -27.47889317205697779, 4.782085928244144135 ) ) ;
#10685 = CARTESIAN_POINT ( 'NONE',  ( -4.939834082512651214, 0.8134902471039170413, -0.6999999999999992895 ) ) ;
#10686 = CARTESIAN_POINT ( 'NONE',  ( 3.072394438959999974, 1.678456730820000020, 230.8356432492296619 ) ) ;
#10687 = B_SPLINE_CURVE_WITH_KNOTS ( 'NONE', 3,
 ( #28982, #16407, #9632, #26014 ),
 .UNSPECIFIED., .F., .F.,
 ( 4, 4 ),
 ( 0.000000000000000000, 1.000000000000000000 ),
 .UNSPECIFIED. ) ;
#10688 = VECTOR ( 'NONE', #234, 1000.000000000000000 ) ;
#10689 = CARTESIAN_POINT ( 'NONE',  ( 1.601115582524632597, -1.226324675095826988, 230.8412452700000301 ) ) ;
#10690 = CARTESIAN_POINT ( 'NONE',  ( -8.999999999559999964, 21.35000000040000145, -64.10000000000000853 ) ) ;
#10691 = CARTESIAN_POINT ( 'NONE',  ( 1.888485499342153151, 5.773790730162923879, -11.07047964830000453 ) ) ;
#10692 = CARTESIAN_POINT ( 'NONE',  ( 6.379535387291454640, -1.442012952481606991, -32.18377053310000946 ) ) ;
#10693 = B_SPLINE_CURVE_WITH_KNOTS ( 'NONE', 3,
 ( #23429, #9084, #1856, #3903, #21057, #6264, #18679, #6722, #13497, #26091 ),
 .UNSPECIFIED., .F., .F.,
 ( 4, 2, 2, 2, 4 ),
 ( 0.000000000000000000, 0.2500000000000000000, 0.5000000000000000000, 0.7500000000000000000, 1.000000000000000000 ),
 .UNSPECIFIED. ) ;
#10694 = CARTESIAN_POINT ( 'NONE',  ( -4.884981308350000102E-15, -2.100000000000000089, 227.6412452697800006 ) ) ;
#10695 = CARTESIAN_POINT ( 'NONE',  ( -6.000000000000000000, -23.16799891216055940, -79.43914708545641190 ) ) ;
#10696 = LINE ( 'NONE', #657, #13137 ) ;
#10697 = CARTESIAN_POINT ( 'NONE',  ( 0.6138679561251692007, 4.311712124478117580, -29.00600711720001357 ) ) ;
#10698 = EDGE_CURVE ( 'NONE', #23553, #11358, #3891, .T. ) ;
#10699 = DIRECTION ( 'NONE',  ( -0.7071067811865475727, 0.7071067811865475727, 0.000000000000000000 ) ) ;
#10700 = CARTESIAN_POINT ( 'NONE',  ( 0.000000000000000000, 0.000000000000000000, 140.0000000000000000 ) ) ;
#10701 = CARTESIAN_POINT ( 'NONE',  ( 22.62517538422034136, 16.36045799713766158, 1.000000000000000888 ) ) ;
#10702 = ORIENTED_EDGE ( 'NONE', *, *, #12468, .T. ) ;
#10703 = VERTEX_POINT ( 'NONE', #8663 ) ;
#10704 = DIRECTION ( 'NONE',  ( 0.000000000000000000, -1.000000000000000000, 0.000000000000000000 ) ) ;
#10705 = CARTESIAN_POINT ( 'NONE',  ( -5.414213562369999622, -31.28896728272270877, -80.26658230080884948 ) ) ;
#10706 = ORIENTED_EDGE ( 'NONE', *, *, #12169, .T. ) ;
#10707 = VECTOR ( 'NONE', #13215, 1000.000000000000000 ) ;
#10708 = CARTESIAN_POINT ( 'NONE',  ( 8.999999999770000869, 18.79791847199999921, -43.89791847198399921 ) ) ;
#10709 = DIRECTION ( 'NONE',  ( -0.9880370573969196046, 0.1542166437529879086, 0.000000000000000000 ) ) ;
#10711 = ORIENTED_EDGE ( 'NONE', *, *, #28681, .F. ) ;
#10710 = AXIS2_PLACEMENT_3D ( 'NONE', #27342, #10663, #10983 ) ;
#10712 = CARTESIAN_POINT ( 'NONE',  ( -9.000000000229999131, 21.70000000000000284, -60.10000000000000142 ) ) ;
#10713 = VERTEX_POINT ( 'NONE', #28334 ) ;
#10714 = ORIENTED_EDGE ( 'NONE', *, *, #22431, .T. ) ;
#10715 = ORIENTED_EDGE ( 'NONE', *, *, #12031, .T. ) ;
#10716 = CARTESIAN_POINT ( 'NONE',  ( 27.04365979920000029, 9.471113331109998867, 230.2432540810000319 ) ) ;
#10717 = CARTESIAN_POINT ( 'NONE',  ( -17.41454186825435357, -30.51562454719971385, -32.14375470241721899 ) ) ;
#10718 = PLANE ( 'NONE',  #516 ) ;
#10719 = CARTESIAN_POINT ( 'NONE',  ( -23.69119896570000350, -20.94188573499999961, 222.0000000000000000 ) ) ;
#10720 = CARTESIAN_POINT ( 'NONE',  ( -24.97129468253034545, 13.73710443232325495, 6.098655031999994591 ) ) ;
#10721 = CARTESIAN_POINT ( 'NONE',  ( 25.77914806503467560, 15.40383291000323318, 8.000000000000007105 ) ) ;
#10722 = CARTESIAN_POINT ( 'NONE',  ( 9.993285220779439371, -25.61999708228226069, 202.0000000000000000 ) ) ;
#10723 = CARTESIAN_POINT ( 'NONE',  ( -7.999999999674140660, -13.61361098168129224, -34.64062768038885309 ) ) ;
#10724 = AXIS2_PLACEMENT_3D ( 'NONE', #25664, #4255, #4407 ) ;
#10725 = ORIENTED_EDGE ( 'NONE', *, *, #12332, .T. ) ;
#10726 = ADVANCED_FACE ( 'NONE', ( #18425 ), #25680, .T. ) ;
#10727 = CARTESIAN_POINT ( 'NONE',  ( 0.7444716670016126026, -5.443307122690507427, -1.373124048000001984 ) ) ;
#10728 = CARTESIAN_POINT ( 'NONE',  ( -4.663991843195165465, -3.413757688390889555, -18.87254627010000263 ) ) ;
#10729 = AXIS2_PLACEMENT_3D ( 'NONE', #9354, #31081, #28712 ) ;
#10730 = CARTESIAN_POINT ( 'NONE',  ( -25.94284618478184967, -6.948772836044501133, 193.2171415879999756 ) ) ;
#10731 = CARTESIAN_POINT ( 'NONE',  ( -8.699999999701292452, -29.44961367803777463, -30.17582256626712223 ) ) ;
#10732 = CARTESIAN_POINT ( 'NONE',  ( 2.035903620463144659, -3.499342391980986733, -92.40868836340082737 ) ) ;
#10733 = CARTESIAN_POINT ( 'NONE',  ( -28.45771199730000234, -1.047388408700000119E-14, 229.4982322489999831 ) ) ;
#10734 = CARTESIAN_POINT ( 'NONE',  ( 18.13191322300000152, -9.527368092900001528, -0.6999999999999992895 ) ) ;
#10735 = ADVANCED_FACE ( 'NONE', ( #14029 ), #4111, .T. ) ;
#10736 = CARTESIAN_POINT ( 'NONE',  ( 18.95046173579999760, -18.95046173579999760, 86.78285841159998881 ) ) ;
#10737 = CARTESIAN_POINT ( 'NONE',  ( -0.1718244463979999859, -18.28023999129999666, 230.6999999999999886 ) ) ;
#10738 = CARTESIAN_POINT ( 'NONE',  ( 4.638687372223642136, -9.701227635570159435, -32.74756430415913400 ) ) ;
#10739 = ORIENTED_EDGE ( 'NONE', *, *, #11600, .F. ) ;
#10740 = CARTESIAN_POINT ( 'NONE',  ( 5.235465350887244185, -2.882605534178610984, -58.30843849682499780 ) ) ;
#10741 = CARTESIAN_POINT ( 'NONE',  ( -24.34246741826368066, -14.82285105945933346, 6.099998581000011022 ) ) ;
#10742 = EDGE_LOOP ( 'NONE', ( #28366, #17483, #16127, #8172, #13228, #19657, #8485, #8565 ) ) ;
#10743 = CARTESIAN_POINT ( 'NONE',  ( 6.034652528523337445, 2.501332855249893683, -11.49261350020000449 ) ) ;
#10744 = ORIENTED_EDGE ( 'NONE', *, *, #6339, .T. ) ;
#10745 = CARTESIAN_POINT ( 'NONE',  ( 27.06563796000000366, -3.314475221599999482E-15, 138.0597313979999967 ) ) ;
#10746 = CARTESIAN_POINT ( 'NONE',  ( -4.164642846343869387, 0.1855225024005626999, -68.10000000002501963 ) ) ;
#10747 = VECTOR ( 'NONE', #2920, 1000.000000000000000 ) ;
#10748 = VERTEX_POINT ( 'NONE', #18260 ) ;
#10749 = EDGE_CURVE ( 'NONE', #9824, #18576, #22009, .T. ) ;
#10750 = AXIS2_PLACEMENT_3D ( 'NONE', #7345, #12211, #21510 ) ;
#10751 = ORIENTED_EDGE ( 'NONE', *, *, #1046, .T. ) ;
#10752 = VERTEX_POINT ( 'NONE', #8982 ) ;
#10753 = CARTESIAN_POINT ( 'NONE',  ( -26.80000000000000071, 9.769962616700000205E-15, 186.7828584120000244 ) ) ;
#10754 = CIRCLE ( 'NONE', #24329, 2.000000000000000000 ) ;
#10755 = ORIENTED_EDGE ( 'NONE', *, *, #22457, .T. ) ;
#10756 = CONICAL_SURFACE ( 'NONE', #25846, 0.9999999999991018296, 0.7853981633970000820 ) ;
#10757 = CARTESIAN_POINT ( 'NONE',  ( 0.000000000000000000, 0.000000000000000000, 229.6412452697800006 ) ) ;
#10758 = LINE ( 'NONE', #19745, #28576 ) ;
#10759 = CARTESIAN_POINT ( 'NONE',  ( -5.001751348353093540, 2.318407806459778175, -64.97526299432499286 ) ) ;
#10760 = CYLINDRICAL_SURFACE ( 'NONE', #21981, 27.50000000000000000 ) ;
#10761 = CARTESIAN_POINT ( 'NONE',  ( -22.51305616955001909, 17.92067914158993247, 0.2374258030000131470 ) ) ;
#10762 = DIRECTION ( 'NONE',  ( -1.000000000000000000, 0.000000000000000000, -2.257144471330000330E-12 ) ) ;
#10763 = COLOUR_RGB ( '', 0.72549020, 0.75294118, 0.79215686) ;
#10764 = SURFACE_STYLE_FILL_AREA ( #22580 ) ;
#10765 = CARTESIAN_POINT ( 'NONE',  ( -25.32653162617393861, 13.07087917251410403, 4.239730451999990102 ) ) ;
#10766 = ORIENTED_EDGE ( 'NONE', *, *, #4472, .F. ) ;
#10767 = CARTESIAN_POINT ( 'NONE',  ( 4.880902371519058036, -3.592936783560450653, -8.972776792900004850 ) ) ;
#10768 = CARTESIAN_POINT ( 'NONE',  ( 0.9891023320736628266, -26.78175549074274642, 5.486606153706005351 ) ) ;
#10769 = AXIS2_PLACEMENT_3D ( 'NONE', #8521, #8207, #24915 ) ;
#10770 = CARTESIAN_POINT ( 'NONE',  ( 10.88909890409999903, 21.70000000000000284, -56.10000000020000499 ) ) ;
#10771 = ORIENTED_EDGE ( 'NONE', *, *, #3346, .F. ) ;
#10772 = CARTESIAN_POINT ( 'NONE',  ( 9.738910687886868089, -24.96785170200598358, 115.0000000000000000 ) ) ;
#10773 = CARTESIAN_POINT ( 'NONE',  ( -0.1113126286645371027, -3.930924299786448195, -38.89973510835675796 ) ) ;
#10774 = CIRCLE ( 'NONE', #20343, 2.000000000000000000 ) ;
#10775 = CIRCLE ( 'NONE', #15290, 1.100000000390000787 ) ;
#10776 = CARTESIAN_POINT ( 'NONE',  ( 3.441895497200000431, 11.73074891959999988, 232.6627635220000059 ) ) ;
#10777 = EDGE_CURVE ( 'NONE', #3989, #23963, #27292, .T. ) ;
#10778 = AXIS2_PLACEMENT_3D ( 'NONE', #5506, #6083, #7707 ) ;
#10779 = CARTESIAN_POINT ( 'NONE',  ( 26.68292649568609320, 9.659560297578410726, 0.8585786470000078552 ) ) ;
#10780 = AXIS2_PLACEMENT_3D ( 'NONE', #2844, #24563, #14660 ) ;
#10781 = FACE_OUTER_BOUND ( 'NONE', #21928, .T. ) ;
#10782 = CARTESIAN_POINT ( 'NONE',  ( 1.815007998551255941, 5.706838904126064094, -60.46492395752500215 ) ) ;
#10783 = CARTESIAN_POINT ( 'NONE',  ( -10.58956532309999865, -24.61949706369999902, -1.102843534499998945 ) ) ;
#10784 = CARTESIAN_POINT ( 'NONE',  ( 27.50000000000000000, 1.776356839399999804E-15, 86.39444872449999480 ) ) ;
#10785 = VERTEX_POINT ( 'NONE', #24699 ) ;
#10786 = CARTESIAN_POINT ( 'NONE',  ( 24.14205449336675713, -13.78537897189897343, 3.957489350000009676 ) ) ;
#10787 = CARTESIAN_POINT ( 'NONE',  ( 27.79999999990000248, 4.333901782529999025, 223.3999999999999773 ) ) ;
#10788 = B_SPLINE_CURVE_WITH_KNOTS ( 'NONE', 5,
 ( #13289, #29966, #29502, #8395, #7939, #18158 ),
 .UNSPECIFIED., .F., .F.,
 ( 6, 6 ),
 ( 0.000000000000000000, 1.000000000000000000 ),
 .UNSPECIFIED. ) ;
#10789 = CARTESIAN_POINT ( 'NONE',  ( 0.1319790757060198549, -27.80015609199462290, 6.042326290000010758 ) ) ;
#10790 = AXIS2_PLACEMENT_3D ( 'NONE', #7333, #105, #9687 ) ;
#10791 = EDGE_CURVE ( 'NONE', #6120, #3279, #29512, .T. ) ;
#10792 = ADVANCED_FACE ( 'NONE', ( #22499 ), #24860, .F. ) ;
#10793 = DIRECTION ( 'NONE',  ( 0.000000000000000000, -2.256683728769999802E-12, -1.000000000000000000 ) ) ;
#10794 = CARTESIAN_POINT ( 'NONE',  ( -3.416035461607788815, -1.991895463217535633, -44.10000000002499121 ) ) ;
#10795 = CARTESIAN_POINT ( 'NONE',  ( 14.83997978847463450, -24.11413778510890893, -32.50719654782172796 ) ) ;
#10796 = CARTESIAN_POINT ( 'NONE',  ( -10.90985356904797321, -24.71798678610834443, -1.786271532367390114 ) ) ;
#10797 = EDGE_CURVE ( 'NONE', #28713, #8037, #3134, .T. ) ;
#10798 = VECTOR ( 'NONE', #1854, 1000.000000000000000 ) ;
#10799 = CARTESIAN_POINT ( 'NONE',  ( -3.112296099710467168, 3.758517760630106785, -63.39933298492499603 ) ) ;
#10800 = AXIS2_PLACEMENT_3D ( 'NONE', #24838, #7986, #3270 ) ;
#10801 = ORIENTED_EDGE ( 'NONE', *, *, #17586, .T. ) ;
#10802 = CARTESIAN_POINT ( 'NONE',  ( 18.71271765012262378, 20.00001436454239112, 230.5947203350884820 ) ) ;
#10803 = EDGE_CURVE ( 'NONE', #28481, #30214, #29570, .T. ) ;
#10804 = VERTEX_POINT ( 'NONE', #29724 ) ;
#10805 = CARTESIAN_POINT ( 'NONE',  ( 8.700000000292124724, -17.59705092275675042, -40.94388382661216497 ) ) ;
#10806 = EDGE_LOOP ( 'NONE', ( #26405, #12810, #21128, #10675 ) ) ;
#10807 = CARTESIAN_POINT ( 'NONE',  ( -11.81476342111506561, 21.69999999997402540, -55.60962715557913327 ) ) ;
#10808 = CARTESIAN_POINT ( 'NONE',  ( -28.50000000000000000, -5.684341886079999373E-14, 229.0000000000000000 ) ) ;
#10809 = CARTESIAN_POINT ( 'NONE',  ( -3.547887315624706162, 0.01749626818370194140, 0.000000000000000000 ) ) ;
#10810 = AXIS2_PLACEMENT_3D ( 'NONE', #3170, #20013, #8344 ) ;
#10811 = CARTESIAN_POINT ( 'NONE',  ( -28.53958170586710352, 1.916106982190598051, 8.000000000000007105 ) ) ;
#10812 = ADVANCED_FACE ( 'NONE', ( #7699 ), #8004, .T. ) ;
#10813 = CARTESIAN_POINT ( 'NONE',  ( 24.73568148353697183, -12.68911065183860920, 5.680831396999986183 ) ) ;
#10814 = AXIS2_PLACEMENT_3D ( 'NONE', #25884, #6827, #23208 ) ;
#10815 = AXIS2_PLACEMENT_3D ( 'NONE', #29100, #10378, #14944 ) ;
#10816 = CARTESIAN_POINT ( 'NONE',  ( -0.8738876050350000702, -27.78662806160000187, 224.3198333100000070 ) ) ;
#10817 = ORIENTED_EDGE ( 'NONE', *, *, #16638, .T. ) ;
#10818 = DIRECTION ( 'NONE',  ( -0.5193310806158223381, -1.929012505286207873E-12, -0.8545731265997089654 ) ) ;
#10819 = CARTESIAN_POINT ( 'NONE',  ( 3.653275382406360627, -2.426579979385206531, -0.6999999999999992895 ) ) ;
#10820 = ADVANCED_FACE ( 'NONE', ( #26911 ), #8152, .T. ) ;
#10821 = CARTESIAN_POINT ( 'NONE',  ( -2.020725942109999895, 3.500000000090000007, 230.5235986622430175 ) ) ;
#10822 = CARTESIAN_POINT ( 'NONE',  ( -8.000000000000000000, -17.74403716370463968, -75.33663091226621589 ) ) ;
#10823 = B_SPLINE_CURVE_WITH_KNOTS ( 'NONE', 1,
 ( #28974, #22059 ),
 .UNSPECIFIED., .F., .F.,
 ( 2, 2 ),
 ( -2.556023926959999973E-06, 0.7000000000009999335 ),
 .UNSPECIFIED. ) ;
#10824 = DIRECTION ( 'NONE',  ( 0.3633921898465291567, 0.9316362575375349842, -1.850371707708594444E-14 ) ) ;
#10825 = B_SPLINE_CURVE_WITH_KNOTS ( 'NONE', 5,
 ( #15821, #29667, #8564, #13133, #885, #17847 ),
 .UNSPECIFIED., .F., .F.,
 ( 6, 6 ),
 ( -2.300779637600000260, 0.000000000000000000 ),
 .UNSPECIFIED. ) ;
#10826 = SURFACE_STYLE_FILL_AREA ( #12555 ) ;
#10827 = CARTESIAN_POINT ( 'NONE',  ( -17.23443287097794752, 9.965626860168409706, -1.400000000000002132 ) ) ;
#10828 = CARTESIAN_POINT ( 'NONE',  ( 3.874396413951479268, -2.399869827310083803, -49.33324460762499797 ) ) ;
#10829 = ADVANCED_FACE ( 'NONE', ( #1091 ), #17454, .F. ) ;
#10830 = FACE_OUTER_BOUND ( 'NONE', #16023, .T. ) ;
#10831 = PRODUCT ( 'Cradle Body', 'Cradle Body', '', ( #28137 ) ) ;
#10832 = CARTESIAN_POINT ( 'NONE',  ( -0.1392084988525406630, 2.100000000239999665, 226.6412452697800006 ) ) ;
#10833 = PLANE ( 'NONE',  #1257 ) ;
#10834 = CARTESIAN_POINT ( 'NONE',  ( -24.83284505762695815, -10.07844553579556823, 43.21714158839643005 ) ) ;
#10835 = CARTESIAN_POINT ( 'NONE',  ( 24.34663841808528417, -12.78636765232546146, 225.0964597117140045 ) ) ;
#10836 = EDGE_LOOP ( 'NONE', ( #5636, #6229, #11183 ) ) ;
#10837 = CARTESIAN_POINT ( 'NONE',  ( 6.379535387291454640, -1.442012952481606991, -32.78377053309999667 ) ) ;
#10838 = PRODUCT_DEFINITION_FORMATION_WITH_SPECIFIED_SOURCE ( 'ANY', '', #30511, .NOT_KNOWN. ) ;
#10839 = ORIENTED_EDGE ( 'NONE', *, *, #19399, .T. ) ;
#10840 = CARTESIAN_POINT ( 'NONE',  ( 2.114229738758179432E-14, 3.003144111683443606E-13, 231.6412452697749984 ) ) ;
#10841 = CARTESIAN_POINT ( 'NONE',  ( 1.728540313474559387, 5.648005006634932990, -51.46125421262499344 ) ) ;
#10842 = ORIENTED_EDGE ( 'NONE', *, *, #17728, .T. ) ;
#10843 = APPLICATION_PROTOCOL_DEFINITION ( 'draft international standard', 'automotive_design', 1998, #1352 ) ;
#10844 = ORIENTED_EDGE ( 'NONE', *, *, #2854, .F. ) ;
#10845 = ORIENTED_EDGE ( 'NONE', *, *, #29319, .T. ) ;
#10846 = CARTESIAN_POINT ( 'NONE',  ( -17.66508489110463032, -9.721079119778234912, 0.000000000000000000 ) ) ;
#10847 = CARTESIAN_POINT ( 'NONE',  ( 0.000000000000000000, 0.000000000000000000, 90.00000000000000000 ) ) ;
#10848 = CARTESIAN_POINT ( 'NONE',  ( -17.38249745079332698, -28.28848602987763527, -23.37040506449729094 ) ) ;
#10849 = CARTESIAN_POINT ( 'NONE',  ( -7.999999999938637529, -122.9973754718770493, 4.341317972039581363 ) ) ;
#10850 = CARTESIAN_POINT ( 'NONE',  ( -10.00000000070000183, -30.00000000000000000, -28.40000000000000213 ) ) ;
#10851 = EDGE_CURVE ( 'NONE', #24389, #16212, #20164, .T. ) ;
#10852 = CARTESIAN_POINT ( 'NONE',  ( -3.950843061919687038, 0.4864325623484713201, -0.6999999999999994005 ) ) ;
#10853 = CARTESIAN_POINT ( 'NONE',  ( 6.105340317846409626, -0.2107885887935728730, -2.685409721200002320 ) ) ;
#10854 = CARTESIAN_POINT ( 'NONE',  ( 1.226324675095736394, 1.601115582524161862, 230.8412452700000017 ) ) ;
#10855 = CYLINDRICAL_SURFACE ( 'NONE', #24561, 3.000000000000003997 ) ;
#10856 = VERTEX_POINT ( 'NONE', #645 ) ;
#10857 = EDGE_CURVE ( 'NONE', #13261, #2824, #10232, .T. ) ;
#10858 = CARTESIAN_POINT ( 'NONE',  ( -6.108812354267502798, 0.1812703649498176306, -13.18304957890000040 ) ) ;
#10859 = CARTESIAN_POINT ( 'NONE',  ( 0.09516252086846690994, -5.505278045713965618, -32.41110030500000505 ) ) ;
#10860 = EDGE_CURVE ( 'NONE', #17478, #9711, #14454, .T. ) ;
#10861 = ADVANCED_FACE ( 'NONE', ( #6583, #4074, #13988 ), #25947, .F. ) ;
#10862 = LINE ( 'NONE', #22359, #18184 ) ;
#10863 = CYLINDRICAL_SURFACE ( 'NONE', #29367, 2.500000000000000888 ) ;
#10864 = DIRECTION ( 'NONE',  ( 0.000000000000000000, 0.000000000000000000, 1.000000000000000000 ) ) ;
#10865 = CARTESIAN_POINT ( 'NONE',  ( 10.00000000000000000, 20.99999999999999645, -60.10000000019999788 ) ) ;
#10866 = CARTESIAN_POINT ( 'NONE',  ( -3.856237990133467353, 0.3204508335913280881, 227.8575818780809357 ) ) ;
#10867 = B_SPLINE_CURVE_WITH_KNOTS ( 'NONE', 3,
 ( #18175, #17857, #3240, #12995, #20230, #8107, #27777, #29519, #27317, #13307 ),
 .UNSPECIFIED., .F., .F.,
 ( 4, 2, 2, 2, 4 ),
 ( 0.000000000000000000, 0.2499999999999998890, 0.4999999999999998890, 0.7500000000000000000, 1.000000000000000000 ),
 .UNSPECIFIED. ) ;
#10868 = CARTESIAN_POINT ( 'NONE',  ( 18.97091132401531510, 21.26865671844599248, 0.7595836940000044724 ) ) ;
#10869 = FACE_OUTER_BOUND ( 'NONE', #22176, .T. ) ;
#10870 = CARTESIAN_POINT ( 'NONE',  ( 0.4821455017210000138, -28.49635764770000179, 223.9974824469999817 ) ) ;
#10871 = ORIENTED_EDGE ( 'NONE', *, *, #2166, .F. ) ;
#10872 = CARTESIAN_POINT ( 'NONE',  ( 23.78314118259453380, 14.39461387841678608, 6.098654095000016540 ) ) ;
#10873 = CARTESIAN_POINT ( 'NONE',  ( -5.010133801301174472, -31.60104845553905761, -80.38017055838898273 ) ) ;
#10874 = ORIENTED_EDGE ( 'NONE', *, *, #12521, .F. ) ;
#10875 = CARTESIAN_POINT ( 'NONE',  ( -9.000000000000000000, 19.99999999999999645, -44.10000000000000142 ) ) ;
#10876 = DIRECTION ( 'NONE',  ( 2.257150022439999944E-12, 0.000000000000000000, 1.000000000000000000 ) ) ;
#10877 = ORIENTED_EDGE ( 'NONE', *, *, #30437, .T. ) ;
#10878 = CARTESIAN_POINT ( 'NONE',  ( -9.993285220779425160, -25.61999708228226069, 27.99999999999999645 ) ) ;
#10879 = ORIENTED_EDGE ( 'NONE', *, *, #25796, .T. ) ;
#10880 = EDGE_LOOP ( 'NONE', ( #13124, #6459, #2900, #4944, #27760, #9966 ) ) ;
#10881 = ORIENTED_EDGE ( 'NONE', *, *, #15426, .F. ) ;
#10882 = B_SPLINE_CURVE_WITH_KNOTS ( 'NONE', 5,
 ( #25882, #26181, #7137, #26032, #9027, #8867, #4473, #19097, #4788, #16575, #18471, #9336 ),
 .UNSPECIFIED., .F., .F.,
 ( 6, 3, 3, 6 ),
 ( 0.000000000000000000, 0.5717440563929999664, 1.143488112780000066, 1.429360140980000082 ),
 .UNSPECIFIED. ) ;
#10883 = FACE_OUTER_BOUND ( 'NONE', #18999, .T. ) ;
#10884 = DIRECTION ( 'NONE',  ( -1.224606353819999829E-16, -1.000000000000000000, 0.000000000000000000 ) ) ;
#10885 = ORIENTED_EDGE ( 'NONE', *, *, #9283, .T. ) ;
#10886 = CARTESIAN_POINT ( 'NONE',  ( -20.30396346370000060, 20.00000000000000000, 229.0000000000000000 ) ) ;
#10887 = CARTESIAN_POINT ( 'NONE',  ( 17.14656078602323319, -7.900182044548062166, -1.000005633855494125E-09 ) ) ;
#10888 = CARTESIAN_POINT ( 'NONE',  ( 6.756062549273604390, -26.65810324902503581, 208.5456572472911034 ) ) ;
#10889 = CARTESIAN_POINT ( 'NONE',  ( 9.000000000000000000, 19.99999999999999645, -43.39999999999999858 ) ) ;
#10890 = CARTESIAN_POINT ( 'NONE',  ( 23.77307027438179077, -14.41181805763359947, 4.926507320169768889 ) ) ;
#10891 = B_SPLINE_CURVE_WITH_KNOTS ( 'NONE', 5,
 ( #30737, #21454, #23974, #7434, #9167, #31048, #6818, #4776, #12003 ),
 .UNSPECIFIED., .F., .F.,
 ( 6, 3, 6 ),
 ( 8.011061266649999624, 9.405960541640000727, 10.80085981660000094 ),
 .UNSPECIFIED. ) ;
#10892 = CARTESIAN_POINT ( 'NONE',  ( 1.213582369797474136, 4.521795443253902924, -2.553410702900004825 ) ) ;
#10893 = CARTESIAN_POINT ( 'NONE',  ( -4.430040892179083478, 1.363067613765873931, -22.32289663399999924 ) ) ;
#10894 = CARTESIAN_POINT ( 'NONE',  ( -9.993285220779425160, -25.61999708228226069, 202.0000000000000000 ) ) ;
#10895 = CARTESIAN_POINT ( 'NONE',  ( 0.000000000000000000, 0.000000000000000000, 20.00000000000000355 ) ) ;
#10896 = CARTESIAN_POINT ( 'NONE',  ( -0.5424735333374979263, -3.475525990910468987, -90.24054733466465450 ) ) ;
#10897 = CARTESIAN_POINT ( 'NONE',  ( -25.33612502140000089, 14.05463924120000030, 229.7625741969999922 ) ) ;
#10898 = CARTESIAN_POINT ( 'NONE',  ( -0.9484597805798516967, -0.1361449379680841898, -98.10259367259483554 ) ) ;
#10899 = DIRECTION ( 'NONE',  ( 3.084553072890618732E-12, 0.8902635789277789646, -0.4554456718805243165 ) ) ;
#10900 = CARTESIAN_POINT ( 'NONE',  ( 25.41516571979999739, -14.56554164990000011, 229.0000000000000000 ) ) ;
#10901 = CARTESIAN_POINT ( 'NONE',  ( 26.30683953509999640, -5.612727362360000249, 230.6999999999999886 ) ) ;
#10902 = CARTESIAN_POINT ( 'NONE',  ( 2.114229738758179432E-14, 3.003144111683443606E-13, 231.6412452697749984 ) ) ;
#10903 = B_SPLINE_CURVE_WITH_KNOTS ( 'NONE', 3,
 ( #3234, #5902, #22746, #12523, #10334, #24493, #893, #15504, #25110, #14900, #10486, #29976, #3544, #20387, #22134, #592, #20866, #30464, #23224, #13456, #1353, #15826, #4177, #27938, #11414, #23071, #13773, #23391, #13619, #28089, #1825, #6534, #15657, #30138, #1665, #1515, #3863, #18643, #28240, #6684, #11106, #20700, #8886, #18491, #16287, #10946, #30299, #8731, #18335, #6379, #11263, #15977, #21017, #13933, #30621, #20541, #27772, #22911, #25266, #25587, #4023, #6219, #16130, #13301, #23544, #25743, #9045, #25434, #8568, #25900, #4338, #18169, #1981, #11572, #3699, #21168, #30766, #9194, #18798, #6062, #28406, #26658, #12340, #24148, #16443, #16899, #7314, #14559, #2443, #6841, #2589, #21640, #26052, #26360, #7004, #398, #21324, #4490, #26504, #2293, #14091, #4946, #14401, #4637, #19269, #21479, #28860 ),
 .UNSPECIFIED., .F., .F.,
 ( 4, 1, 2, 2, 1, 1, 2, 2, 1, 1, 1, 2, 2, 1, 1, 1, 1, 2, 2, 1, 1, 1, 2, 2, 1, 1, 1, 1, 2, 2, 1, 1, 1, 2, 2, 1, 1, 1, 1, 2, 2, 1, 1, 1, 2, 2, 1, 1, 1, 2, 2, 1, 1, 2, 2, 1, 1, 2, 2, 1, 2, 2, 1, 2, 2, 1, 2, 2, 2, 2, 2, 4 ),
 ( 0.000000000000000000, 0.06250000000000016653, 0.09375000000000027756, 0.1250000000000003886, 0.1875000000000005274, 0.2187500000000006106, 0.2343750000000006661, 0.2500000000000006661, 0.2812500000000007772, 0.2968750000000007772, 0.3046875000000008327, 0.3085937500000008327, 0.3125000000000008327, 0.3437500000000009992, 0.3593750000000010547, 0.3671875000000011102, 0.3710937500000010547, 0.3730468750000010547, 0.3750000000000010547, 0.3906250000000009437, 0.3984375000000008882, 0.4023437500000007772, 0.4042968750000006661, 0.4062500000000005551, 0.4140625000000003886, 0.4179687500000002220, 0.4199218750000000555, 0.4208984375000000000, 0.4213867187500000000, 0.4218750000000000000, 0.4296874999999996114, 0.4335937499999994449, 0.4355468749999994449, 0.4365234374999995004, 0.4374999999999995559, 0.4453125000000000555, 0.4492187500000002776, 0.4511718750000003886, 0.4521484375000004441, 0.4526367187500004996, 0.4531250000000005551, 0.4609375000000009992, 0.4648437500000011657, 0.4667968750000012212, 0.4677734375000013323, 0.4687500000000014988, 0.4765625000000021094, 0.4804687500000023870, 0.4824218750000024980, 0.4833984375000025535, 0.4843750000000026090, 0.4921875000000026090, 0.4960937500000026090, 0.4980468750000025535, 0.5000000000000025535, 0.5156250000000015543, 0.5234375000000012212, 0.5273437500000009992, 0.5312500000000007772, 0.5468750000000004441, 0.5546875000000003331, 0.5625000000000002220, 0.5937500000000001110, 0.6093750000000002220, 0.6250000000000002220, 0.6562500000000002220, 0.6718750000000002220, 0.6875000000000002220, 0.7187500000000002220, 0.7500000000000002220, 0.8750000000000001110, 1.000000000000000000 ),
 .UNSPECIFIED. ) ;
#10904 = ORIENTED_EDGE ( 'NONE', *, *, #21745, .F. ) ;
#10905 = CARTESIAN_POINT ( 'NONE',  ( -0.06606756225350368661, 5.646037861211643083, -57.31818518972499277 ) ) ;
#10906 = CARTESIAN_POINT ( 'NONE',  ( -23.88383647328724280, -15.55037090958975909, 5.498277346593025250 ) ) ;
#10907 = ORIENTED_EDGE ( 'NONE', *, *, #18448, .T. ) ;
#10908 = CARTESIAN_POINT ( 'NONE',  ( 3.256742448429973624, 4.730705660258329281, -17.21259163649999735 ) ) ;
#10909 = ORIENTED_EDGE ( 'NONE', *, *, #21707, .F. ) ;
#10910 = CARTESIAN_POINT ( 'NONE',  ( 2.131628207279999844E-14, 1.421085471519999843E-14, 231.6999999999999886 ) ) ;
#10911 = VERTEX_POINT ( 'NONE', #20591 ) ;
#10912 = LINE ( 'NONE', #30845, #418 ) ;
#10913 = EDGE_CURVE ( 'NONE', #19402, #18717, #20750, .T. ) ;
#10914 = ORIENTED_EDGE ( 'NONE', *, *, #23516, .F. ) ;
#10915 = ORIENTED_EDGE ( 'NONE', *, *, #5042, .F. ) ;
#10916 = DIRECTION ( 'NONE',  ( 0.000000000000000000, 0.000000000000000000, -1.000000000000000000 ) ) ;
#10917 = EDGE_LOOP ( 'NONE', ( #26743, #9032 ) ) ;
#10918 = CARTESIAN_POINT ( 'NONE',  ( 9.738910687886932038, -24.96785170200595161, 43.21714158840000408 ) ) ;
#10919 = CARTESIAN_POINT ( 'NONE',  ( 0.000000000000000000, 5.495185456771864096, -69.00660115587162124 ) ) ;
#10920 = CARTESIAN_POINT ( 'NONE',  ( -3.508509149557995421, -4.733412845326351537, -64.33409070562500176 ) ) ;
#10921 = ADVANCED_FACE ( 'NONE', ( #6278 ), #28530, .F. ) ;
#10922 = CARTESIAN_POINT ( 'NONE',  ( 1.645560275461343203, -28.45273235261698019, 4.999998581000003384 ) ) ;
#10923 = VECTOR ( 'NONE', #22109, 1000.000000000000000 ) ;
#10924 = VECTOR ( 'NONE', #4234, 1000.000000000000114 ) ;
#10925 = CARTESIAN_POINT ( 'NONE',  ( -10.69999999989999928, -25.00000000000000000, -2.399999999999999467 ) ) ;
#10926 = DIRECTION ( 'NONE',  ( 0.000000000000000000, 0.000000000000000000, 1.000000000000000000 ) ) ;
#10927 = CYLINDRICAL_SURFACE ( 'NONE', #539, 1.099999999999999867 ) ;
#10928 = FACE_BOUND ( 'NONE', #10526, .T. ) ;
#10929 = CARTESIAN_POINT ( 'NONE',  ( 5.967946066639521874, -1.056419632483374116, -8.771482634700005221 ) ) ;
#10930 = CARTESIAN_POINT ( 'NONE',  ( 1.099927927705516062, -26.77741881808359992, 5.145878552788805571 ) ) ;
#10931 = CARTESIAN_POINT ( 'NONE',  ( -26.84464183080000055, 3.287411895199999866E-15, 92.56249624490000372 ) ) ;
#10932 = ORIENTED_EDGE ( 'NONE', *, *, #15610, .T. ) ;
#10933 = CARTESIAN_POINT ( 'NONE',  ( 24.60092358069999818, -12.94742893959999819, 224.7916409239999780 ) ) ;
#10934 = DIRECTION ( 'NONE',  ( 0.9880370573969197157, -0.1542166437529880196, 2.958228394580000263E-31 ) ) ;
#10935 = CARTESIAN_POINT ( 'NONE',  ( -28.49999999970000175, -10.47094308429999998, 222.0000000000000000 ) ) ;
#10936 = CARTESIAN_POINT ( 'NONE',  ( 27.68716793528856712, 5.086682278514146560, 0.7069222069999991920 ) ) ;
#10937 = CARTESIAN_POINT ( 'NONE',  ( -10.69999999930000101, -29.30501631370000482, -26.47986984990000181 ) ) ;
#10938 = CARTESIAN_POINT ( 'NONE',  ( -13.99999999969999820, 21.69999999929999390, -58.51619611000000276 ) ) ;
#10939 = CARTESIAN_POINT ( 'NONE',  ( -12.68069379941013253, 20.99999999997307398, -56.02824004937883018 ) ) ;
#10940 = DIRECTION ( 'NONE',  ( 1.000000000000000000, -0.000000000000000000, -9.868649108069999529E-17 ) ) ;
#10941 = ORIENTED_EDGE ( 'NONE', *, *, #9420, .F. ) ;
#10942 = EDGE_CURVE ( 'NONE', #4997, #9909, #27617, .T. ) ;
#10943 = CARTESIAN_POINT ( 'NONE',  ( 26.95545381250000361, 8.667969360499998999, 229.0000000000000000 ) ) ;
#10944 = AXIS2_PLACEMENT_3D ( 'NONE', #10682, #29877, #8308 ) ;
#10945 = VECTOR ( 'NONE', #25784, 1000.000000000000000 ) ;
#10946 = CARTESIAN_POINT ( 'NONE',  ( 2.557726607724730705, -3.485748181607284835, -68.10000000002503384 ) ) ;
#10947 = CIRCLE ( 'NONE', #31055, 5.999999999999999112 ) ;
#10948 = B_SPLINE_CURVE_WITH_KNOTS ( 'NONE', 3,
 ( #8513, #18114, #21230, #4865, #18273, #25532 ),
 .UNSPECIFIED., .F., .F.,
 ( 4, 2, 4 ),
 ( 0.000000000000000000, 0.5000000000000000000, 1.000000000000000000 ),
 .UNSPECIFIED. ) ;
#10949 = CARTESIAN_POINT ( 'NONE',  ( 26.76132339671151072, 2.369424447203797524, -0.6999999999999784173 ) ) ;
#10950 = CARTESIAN_POINT ( 'NONE',  ( -3.857208203705276173, -1.109566970332652946, -44.10000000002499121 ) ) ;
#10951 = PLANE ( 'NONE',  #25773 ) ;
#10952 = CARTESIAN_POINT ( 'NONE',  ( -4.861312627816293919, -19.12054368222343470, -31.49126272763050238 ) ) ;
#10953 = CARTESIAN_POINT ( 'NONE',  ( -4.568101251964836074, -0.2431723019727868862, -65.56421022022500722 ) ) ;
#10954 = EDGE_LOOP ( 'NONE', ( #20826, #21277, #13107, #5367 ) ) ;
#10955 = EDGE_CURVE ( 'NONE', #31086, #7075, #4383, .T. ) ;
#10956 = CARTESIAN_POINT ( 'NONE',  ( -8.699999999730072986, -28.07050130677435362, -25.59757157925566773 ) ) ;
#10957 = AXIS2_PLACEMENT_3D ( 'NONE', #21245, #1318, #14014 ) ;
#10958 = ORIENTED_EDGE ( 'NONE', *, *, #8448, .T. ) ;
#10959 = CARTESIAN_POINT ( 'NONE',  ( 13.73773747404255552, -26.37022765825810922, 0.000000000000000000 ) ) ;
#10960 = ORIENTED_EDGE ( 'NONE', *, *, #7644, .T. ) ;
#10961 = CARTESIAN_POINT ( 'NONE',  ( 23.88690489929999927, -14.22221811490000043, 226.0424736289999714 ) ) ;
#10962 = CARTESIAN_POINT ( 'NONE',  ( -4.276011752261355880, -43.23306002164930817, -10.18642677534438512 ) ) ;
#10963 = CARTESIAN_POINT ( 'NONE',  ( -23.64633388399750658, -12.61377020593197784, 225.6389823649609525 ) ) ;
#10964 = CARTESIAN_POINT ( 'NONE',  ( 2.858922298043036214, 2.052062286655957024, 0.000000000000000000 ) ) ;
#10965 = CIRCLE ( 'NONE', #3936, 12.03781779370000038 ) ;
#10966 = DIRECTION ( 'NONE',  ( 0.000000000000000000, -0.4794255386042043932, -0.8775825618903719816 ) ) ;
#10967 = CARTESIAN_POINT ( 'NONE',  ( -16.60814955199252552, -10.08408157955485684, 0.000000000000000000 ) ) ;
#10968 = DIRECTION ( 'NONE',  ( -1.000000000000000000, 6.565028073413479156E-24, -2.257144471327815248E-12 ) ) ;
#10969 = ORIENTED_EDGE ( 'NONE', *, *, #12310, .T. ) ;
#10970 = FACE_BOUND ( 'NONE', #9254, .T. ) ;
#10971 = EDGE_CURVE ( 'NONE', #23430, #7509, #288, .T. ) ;
#10972 = CARTESIAN_POINT ( 'NONE',  ( 3.843630909669756957, -2.553018000905745044, -0.6999999999999992895 ) ) ;
#10973 = CARTESIAN_POINT ( 'NONE',  ( 1.041496722224801719, -27.78066294026401906, 225.3591738694975675 ) ) ;
#10974 = EDGE_CURVE ( 'NONE', #31001, #9026, #28295, .T. ) ;
#10975 = CARTESIAN_POINT ( 'NONE',  ( -3.945435489976578225, 0.1663052733796139271, 230.5790337530978036 ) ) ;
#10976 = CARTESIAN_POINT ( 'NONE',  ( -7.999999999720649235, -24.05737431392700287, -27.69631921959670251 ) ) ;
#10977 = B_SPLINE_CURVE_WITH_KNOTS ( 'NONE', 3,
 ( #22056, #507, #39, #7265, #10091, #19685 ),
 .UNSPECIFIED., .F., .F.,
 ( 4, 2, 4 ),
 ( 0.000000000000000000, 0.5000000000000000000, 1.000000000000000000 ),
 .UNSPECIFIED. ) ;
#10978 = PLANE ( 'NONE',  #23586 ) ;
#10979 = CARTESIAN_POINT ( 'NONE',  ( 23.52813227406869245, 14.80830602532641294, 4.039148185435011307 ) ) ;
#10980 = CARTESIAN_POINT ( 'NONE',  ( -15.88307796629033852, -8.427117116629231575, -0.6999999999999784173 ) ) ;
#10981 = CARTESIAN_POINT ( 'NONE',  ( -0.6751951171115599948, 5.935132877056520151, -48.26410749632500341 ) ) ;
#10982 = AXIS2_PLACEMENT_3D ( 'NONE', #8905, #23089, #4509 ) ;
#10983 = DIRECTION ( 'NONE',  ( 0.000000000000000000, -2.257145581549999994E-12, -1.000000000000000000 ) ) ;
#10984 = FACE_OUTER_BOUND ( 'NONE', #11692, .T. ) ;
#10985 = CARTESIAN_POINT ( 'NONE',  ( -7.031490306203408203, -7.073324205343428872, -34.02927844668474222 ) ) ;
#10986 = CARTESIAN_POINT ( 'NONE',  ( -27.92857142909999979, 3.420150602519999655E-15, 192.0603150150000147 ) ) ;
#10987 = CIRCLE ( 'NONE', #17514, 27.50000000000000000 ) ;
#10988 = DIRECTION ( 'NONE',  ( 0.000000000000000000, -1.000000000000000000, 0.000000000000000000 ) ) ;
#10989 = VERTEX_POINT ( 'NONE', #11317 ) ;
#10990 = CARTESIAN_POINT ( 'NONE',  ( -5.496316421720869982, 0.7952554554161578304, -35.25783976330000513 ) ) ;
#10992 = EDGE_CURVE ( 'NONE', #18650, #10676, #5388, .T. ) ;
#10991 = CIRCLE ( 'NONE', #20017, 4.000000000000001776 ) ;
#10993 = ORIENTED_EDGE ( 'NONE', *, *, #24054, .F. ) ;
#10994 = CARTESIAN_POINT ( 'NONE',  ( -3.108138112192400104, -3.359256988581868608, -50.59612412472500154 ) ) ;
#10995 = VERTEX_POINT ( 'NONE', #30516 ) ;
#10996 = PRODUCT_CONTEXT ( 'NONE', #8545, 'mechanical' ) ;
#10997 = EDGE_LOOP ( 'NONE', ( #12026, #14407 ) ) ;
#10998 = ORIENTED_EDGE ( 'NONE', *, *, #7552, .F. ) ;
#10999 = CYLINDRICAL_SURFACE ( 'NONE', #16286, 3.000000000000005329 ) ;
#11000 = ADVANCED_FACE ( 'NONE', ( #30669 ), #9094, .T. ) ;
#11001 = PLANE ( 'NONE',  #21517 ) ;
#11002 = DIRECTION ( 'NONE',  ( 0.000000000000000000, 0.000000000000000000, 1.000000000000000000 ) ) ;
#11003 = AXIS2_PLACEMENT_3D ( 'NONE', #19637, #26714, #19486 ) ;
#11004 = CARTESIAN_POINT ( 'NONE',  ( 9.000000000000000000, -55.00000000000000000, -43.39999999999999858 ) ) ;
#11005 = CARTESIAN_POINT ( 'NONE',  ( 31.69999999989999395, 19.99999999999999645, -0.6999999999999992895 ) ) ;
#11006 = DIRECTION ( 'NONE',  ( -1.000000000000000000, 0.000000000000000000, 0.000000000000000000 ) ) ;
#11007 = CARTESIAN_POINT ( 'NONE',  ( -0.9973419271877559389, -5.413498265897602302, -2.525234013000000832 ) ) ;
#11008 = CARTESIAN_POINT ( 'NONE',  ( -10.00000000070000183, -30.00000000000000000, -28.40000000000000213 ) ) ;
#11009 = DIRECTION ( 'NONE',  ( -1.595945597898660305E-12, 0.7071067811865475727, -0.7071067811865475727 ) ) ;
#11010 = CARTESIAN_POINT ( 'NONE',  ( -1.499765329346335108, -5.740821375879678001, -13.55022317839999424 ) ) ;
#11011 = DIRECTION ( 'NONE',  ( 0.000000000000000000, 0.000000000000000000, -1.000000000000000000 ) ) ;
#11012 = CIRCLE ( 'NONE', #28603, 0.2500000000000002220 ) ;
#11013 = CARTESIAN_POINT ( 'NONE',  ( 5.240471012820000496, 2.862882362300000150, 226.6412452697800006 ) ) ;
#11014 = CARTESIAN_POINT ( 'NONE',  ( 8.000000000730963734, -26.52402217160887332, -25.41208138063096200 ) ) ;
#11015 = CARTESIAN_POINT ( 'NONE',  ( 0.8959394325020000327, -28.48619164239999790, 224.3198498209999912 ) ) ;
#11016 = CARTESIAN_POINT ( 'NONE',  ( 12.88923445963852288, -24.80392650440079905, 8.000000000000007105 ) ) ;
#11017 = CARTESIAN_POINT ( 'NONE',  ( -3.576869721619468478, 0.8042774860780150803, 227.7419800002267039 ) ) ;
#11018 = B_SPLINE_CURVE_WITH_KNOTS ( 'NONE', 3,
 ( #26187, #4622, #16887, #12472, #14389, #23988, #9501, #7449, #7141, #31062, #14228, #26646, #75, #24137 ),
 .UNSPECIFIED., .F., .F.,
 ( 4, 2, 2, 2, 2, 2, 4 ),
 ( 0.000000000000000000, 0.2500000000000006106, 0.3750000000000016098, 0.4375000000000014433, 0.5000000000000013323, 0.7500000000000006661, 1.000000000000000000 ),
 .UNSPECIFIED. ) ;
#11019 = CARTESIAN_POINT ( 'NONE',  ( 23.20948082139999968, -13.40000000000000036, 226.0999999999999943 ) ) ;
#11020 = DIRECTION ( 'NONE',  ( 0.000000000000000000, 0.000000000000000000, -1.000000000000000000 ) ) ;
#11021 = FACE_OUTER_BOUND ( 'NONE', #14836, .T. ) ;
#11022 = ORIENTED_EDGE ( 'NONE', *, *, #7708, .T. ) ;
#11023 = VERTEX_POINT ( 'NONE', #16340 ) ;
#11024 = CARTESIAN_POINT ( 'NONE',  ( 23.29312071241426096, 15.17488100587054767, 5.506989593000027661 ) ) ;
#11025 = CARTESIAN_POINT ( 'NONE',  ( 17.95841148948556310, 10.23646161652002817, 0.000000000000000000 ) ) ;
#11026 = MANIFOLD_SOLID_BREP ( 'Stock-MAS-156-1', #4013 ) ;
#11027 = VERTEX_POINT ( 'NONE', #9570 ) ;
#11028 = CARTESIAN_POINT ( 'NONE',  ( -22.96035733413718916, -13.82212301906527863, 224.0048062721249664 ) ) ;
#11029 = CARTESIAN_POINT ( 'NONE',  ( -25.22658730140000216, -13.26242337740000110, 224.8957833819999621 ) ) ;
#11030 = EDGE_CURVE ( 'NONE', #20395, #3580, #18652, .T. ) ;
#11031 = CARTESIAN_POINT ( 'NONE',  ( -0.8540969733681119669, -5.154519737500188548, -0.7000226888021040539 ) ) ;
#11032 = ORIENTED_EDGE ( 'NONE', *, *, #11822, .T. ) ;
#11033 = CARTESIAN_POINT ( 'NONE',  ( -9.797681423453962424, -25.69548940455785413, 26.16126510391729454 ) ) ;
#11034 = ORIENTED_EDGE ( 'NONE', *, *, #30380, .T. ) ;
#11035 = ORIENTED_EDGE ( 'NONE', *, *, #27794, .F. ) ;
#11036 = EDGE_CURVE ( 'NONE', #30538, #3949, #16490, .T. ) ;
#11037 = AXIS2_PLACEMENT_3D ( 'NONE', #3327, #13229, #15298 ) ;
#11038 = VERTEX_POINT ( 'NONE', #16642 ) ;
#11039 = CARTESIAN_POINT ( 'NONE',  ( -8.699999998932284484, -16.96959321760381556, -37.81493174590716677 ) ) ;
#11040 = ADVANCED_FACE ( 'NONE', ( #11620 ), #2184, .F. ) ;
#11041 = ORIENTED_EDGE ( 'NONE', *, *, #12124, .T. ) ;
#11042 = CARTESIAN_POINT ( 'NONE',  ( -24.55564696219999732, -13.03410599059999875, 225.5071265450000055 ) ) ;
#11043 = CARTESIAN_POINT ( 'NONE',  ( -4.041451884379999804, 9.156941871420000667E-11, 227.9588918784999976 ) ) ;
#11044 = CARTESIAN_POINT ( 'NONE',  ( 2.604168029909177839, 2.875036802038033024, -35.70000000000000284 ) ) ;
#11045 = CARTESIAN_POINT ( 'NONE',  ( 17.29052661994763795, -7.897562529848215718, -4.336808689942017736E-16 ) ) ;
#11046 = CARTESIAN_POINT ( 'NONE',  ( 16.39979399493674705, -21.22530604129068266, -1.399999999999998357 ) ) ;
#11047 = FACE_OUTER_BOUND ( 'NONE', #30851, .T. ) ;
#11048 = CARTESIAN_POINT ( 'NONE',  ( -0.8259893078309999970, -28.48844349870000059, 225.7596419580000315 ) ) ;
#11049 = ORIENTED_EDGE ( 'NONE', *, *, #16873, .F. ) ;
#11050 = CARTESIAN_POINT ( 'NONE',  ( 3.206179479465854243, -3.994457159022797299, -4.042821867100004241 ) ) ;
#11051 = CARTESIAN_POINT ( 'NONE',  ( -4.215937884789282108, -1.105999120962573246, -24.54656121680000069 ) ) ;
#11052 = DIRECTION ( 'NONE',  ( -1.224606353819999829E-16, -1.000000000000000000, 0.000000000000000000 ) ) ;
#11053 = CARTESIAN_POINT ( 'NONE',  ( -8.699999999695858577, -28.58460556449822576, -30.97768745922355293 ) ) ;
#11054 = CARTESIAN_POINT ( 'NONE',  ( 3.043095165746811048, -3.198806529902668672, -95.69213379017060106 ) ) ;
#11055 = CARTESIAN_POINT ( 'NONE',  ( -28.50000000000000000, -3.445280580419999703E-14, 229.2404163060000144 ) ) ;
#11056 = DIRECTION ( 'NONE',  ( 0.9316362575375356503, 0.3633921898465274913, 0.000000000000000000 ) ) ;
#11057 = CARTESIAN_POINT ( 'NONE',  ( -23.95524095760000094, -14.10746636989999914, 226.0798679369999888 ) ) ;
#11058 = CARTESIAN_POINT ( 'NONE',  ( 25.41516571979999739, -14.56554165020000013, 222.0000000000000000 ) ) ;
#11059 = CARTESIAN_POINT ( 'NONE',  ( 0.5020148408599999224, -26.94192660829999753, 230.6999999999999886 ) ) ;
#11060 = DIRECTION ( 'NONE',  ( 0.000000000000000000, 0.000000000000000000, 1.000000000000000000 ) ) ;
#11061 = EDGE_LOOP ( 'NONE', ( #1555, #362, #2607, #4536 ) ) ;
#11062 = CARTESIAN_POINT ( 'NONE',  ( -0.8249440165340218289, 4.504533947698903695, -59.85324387862499407 ) ) ;
#11063 = DIRECTION ( 'NONE',  ( -1.000000000000000000, 5.665498452320000818E-16, 0.000000000000000000 ) ) ;
#11064 = ORIENTED_EDGE ( 'NONE', *, *, #9065, .T. ) ;
#11065 = CARTESIAN_POINT ( 'NONE',  ( 5.967946066722823240, -1.056419632538704967, -8.771482634700005221 ) ) ;
#11066 = VERTEX_POINT ( 'NONE', #21848 ) ;
#11067 = CARTESIAN_POINT ( 'NONE',  ( -17.49999999969999820, -24.00000000000000000, -28.40000000020000215 ) ) ;
#11068 = CARTESIAN_POINT ( 'NONE',  ( 10.00000000000000000, 21.70000000000000284, -62.10000000000000142 ) ) ;
#11069 = ORIENTED_EDGE ( 'NONE', *, *, #16930, .F. ) ;
#11070 = CARTESIAN_POINT ( 'NONE',  ( 8.000000000235820252, -29.73863906515999389, -27.17531388883937993 ) ) ;
#11071 = EDGE_LOOP ( 'NONE', ( #6503, #6801, #14229, #2052 ) ) ;
#11072 = ORIENTED_EDGE ( 'NONE', *, *, #16426, .T. ) ;
#11073 = CARTESIAN_POINT ( 'NONE',  ( -11.08346179031913437, -28.41490585489481191, 143.6055512749999821 ) ) ;
#11074 = EDGE_CURVE ( 'NONE', #24186, #12302, #2341, .T. ) ;
#11075 = ORIENTED_EDGE ( 'NONE', *, *, #7234, .T. ) ;
#11076 = CARTESIAN_POINT ( 'NONE',  ( -12.30000000041591512, -30.20000000000000284, -28.81887902048947225 ) ) ;
#11077 = AXIS2_PLACEMENT_3D ( 'NONE', #19834, #26912, #12580 ) ;
#11078 = ADVANCED_FACE ( 'NONE', ( #2494, #20841 ), #19688, .T. ) ;
#11079 = CARTESIAN_POINT ( 'NONE',  ( -9.999999999969999109, -120.5233595632000174, -31.26042064989999858 ) ) ;
#11080 = CARTESIAN_POINT ( 'NONE',  ( -4.155524648305278568, -2.455537445457764978, -67.92382590962499478 ) ) ;
#11081 = CARTESIAN_POINT ( 'NONE',  ( 27.09307779329999732, -7.097577590990000296, 229.9751247039999953 ) ) ;
#11082 = B_SPLINE_CURVE_WITH_KNOTS ( 'NONE', 5,
 ( #20669, #15784, #8535, #6183, #16517, #4563, #23771, #25396, #8690 ),
 .UNSPECIFIED., .F., .F.,
 ( 6, 3, 6 ),
 ( 0.000000000000000000, 0.6973066784960000319, 1.117931991580000117 ),
 .UNSPECIFIED. ) ;
#11083 = CARTESIAN_POINT ( 'NONE',  ( -7.999999999692728458, -26.29631921955218132, -31.34262568607297439 ) ) ;
#11084 = FACE_OUTER_BOUND ( 'NONE', #30265, .T. ) ;
#11085 = AXIS2_PLACEMENT_3D ( 'NONE', #8342, #17938, #5995 ) ;
#11086 = CARTESIAN_POINT ( 'NONE',  ( -17.20708009806455507, -22.48258290086466360, -25.23462928653505344 ) ) ;
#11087 = ORIENTED_EDGE ( 'NONE', *, *, #16138, .F. ) ;
#11088 = CARTESIAN_POINT ( 'NONE',  ( 4.000000000000000000, -31.83942647549183746, -80.46693306215520636 ) ) ;
#11089 = CARTESIAN_POINT ( 'NONE',  ( -4.992376002538913227, -2.377191163338420843, -11.97655742010000957 ) ) ;
#11090 = DIRECTION ( 'NONE',  ( -1.635844237846128888E-12, -0.6889064844606307414, 0.7248502298186121351 ) ) ;
#11091 = CARTESIAN_POINT ( 'NONE',  ( -9.738910687886855655, -24.96785170200598714, 136.7828584120000244 ) ) ;
#11092 = ORIENTED_EDGE ( 'NONE', *, *, #3075, .F. ) ;
#11093 = LINE ( 'NONE', #18322, #4140 ) ;
#11094 = CARTESIAN_POINT ( 'NONE',  ( -24.54452542612009225, -14.48555670042145138, 6.079852602000002548 ) ) ;
#11095 = CARTESIAN_POINT ( 'NONE',  ( -28.50000000000000000, 9.769962616700000205E-15, 222.0000000000000000 ) ) ;
#11096 = CARTESIAN_POINT ( 'NONE',  ( 18.48839925999793721, 20.72770726368470307, 0.7069223660000067966 ) ) ;
#11097 = B_SPLINE_CURVE_WITH_KNOTS ( 'NONE', 5,
 ( #11484, #30682, #16352, #3776, #25494, #6755, #4397, #14003, #9264, #18870, #22977, #11792 ),
 .UNSPECIFIED., .F., .F.,
 ( 6, 3, 3, 6 ),
 ( 11.50063931930000116, 13.17185654790000093, 19.75779804580000132, 23.00143448300000060 ),
 .UNSPECIFIED. ) ;
#11098 = CARTESIAN_POINT ( 'NONE',  ( 8.000000000279957391, -18.28443193505134445, -36.42483736938841332 ) ) ;
#11099 = CARTESIAN_POINT ( 'NONE',  ( 4.390418465362644795, -3.559810858784186127, -55.40923804942499942 ) ) ;
#11100 = CARTESIAN_POINT ( 'NONE',  ( -11.69999999989999928, -24.11120071670000087, -1.399999999999998579 ) ) ;
#11101 = CARTESIAN_POINT ( 'NONE',  ( 9.999999999770000869, 21.70000000000000284, -64.10000000000000853 ) ) ;
#11102 = ORIENTED_EDGE ( 'NONE', *, *, #21369, .F. ) ;
#11103 = FACE_OUTER_BOUND ( 'NONE', #24122, .T. ) ;
#11104 = CARTESIAN_POINT ( 'NONE',  ( 19.80538173169999894, 19.50875421069999760, 223.3999999999999773 ) ) ;
#11105 = EDGE_CURVE ( 'NONE', #13694, #7124, #12629, .T. ) ;
#11106 = CARTESIAN_POINT ( 'NONE',  ( 2.412651764529908593, -3.532429318983099087, -68.10000000002500542 ) ) ;
#11107 = CARTESIAN_POINT ( 'NONE',  ( -2.507604248437026229, -2.484315071403660813, -0.6999999999999784173 ) ) ;
#11108 = CARTESIAN_POINT ( 'NONE',  ( -4.242641152228525669, 0.8719201866695153180, -44.10000000002499831 ) ) ;
#11109 = CIRCLE ( 'NONE', #16625, 1.000000000000000888 ) ;
#11110 = CARTESIAN_POINT ( 'NONE',  ( 7.873274151039644231, -5.775076759590717757, -27.47943436997715594 ) ) ;
#11111 = LINE ( 'NONE', #20707, #3912 ) ;
#11112 = CARTESIAN_POINT ( 'NONE',  ( 5.885062339963589295, 0.1407603604956381704, -64.86686508972501031 ) ) ;
#11113 = VERTEX_POINT ( 'NONE', #15066 ) ;
#11114 = CARTESIAN_POINT ( 'NONE',  ( 19.67543717097858291, 20.00025387898711671, 230.1474802616772308 ) ) ;
#11115 = VERTEX_POINT ( 'NONE', #12858 ) ;
#11116 = CARTESIAN_POINT ( 'NONE',  ( -17.83931601609999973, 20.00000000000000000, 230.0000000010000178 ) ) ;
#11117 = ORIENTED_EDGE ( 'NONE', *, *, #19157, .T. ) ;
#11118 = CARTESIAN_POINT ( 'NONE',  ( 24.02382125689999981, -13.98923529139999999, 226.0959678990000157 ) ) ;
#11119 = CARTESIAN_POINT ( 'NONE',  ( -23.35655559444149887, -15.07705663921310446, 4.319305392000011068 ) ) ;
#11120 = CARTESIAN_POINT ( 'NONE',  ( -8.699999999669890016, -18.36515956938880478, -34.81167447243381474 ) ) ;
#11121 = CARTESIAN_POINT ( 'NONE',  ( -4.175165894169885483, -50.49316738903675628, -44.10000000000000142 ) ) ;
#11122 = B_SPLINE_CURVE_WITH_KNOTS ( 'NONE', 3,
 ( #30047, #8480, #1886, #30530, #28160, #18077, #11485, #20607, #27681, #30205, #15722 ),
 .UNSPECIFIED., .F., .F.,
 ( 4, 1, 1, 1, 2, 2, 4 ),
 ( 0.000000000000000000, 0.2500000000000012768, 0.3750000000000018874, 0.4375000000000022204, 0.4687500000000023870, 0.5000000000000025535, 1.000000000000000000 ),
 .UNSPECIFIED. ) ;
#11123 = CARTESIAN_POINT ( 'NONE',  ( -8.699999999662093586, -15.94902145834643115, -35.53273252493492862 ) ) ;
#11124 = CARTESIAN_POINT ( 'NONE',  ( 6.585786437629999490, -16.41511111490214603, -74.85294138696069410 ) ) ;
#11125 = CARTESIAN_POINT ( 'NONE',  ( -0.3738033647229999645, -27.79799560440000050, 223.9576764909999724 ) ) ;
#11126 = ORIENTED_EDGE ( 'NONE', *, *, #11427, .F. ) ;
#11127 = CARTESIAN_POINT ( 'NONE',  ( 25.77914806503467560, 15.40383291000323318, 8.000000000000007105 ) ) ;
#11128 = CARTESIAN_POINT ( 'NONE',  ( 28.50000000000000000, -2.380388045690000432E-15, 229.2404163060000144 ) ) ;
#11129 = CARTESIAN_POINT ( 'NONE',  ( 3.059320232295363873, -2.907977535978094163, -69.93674681397055792 ) ) ;
#11130 = ADVANCED_FACE ( 'NONE', ( #5460 ), #13006, .T. ) ;
#11131 = CARTESIAN_POINT ( 'NONE',  ( -3.520849940866991989, 0.9017090165965767623, 230.7589734104482488 ) ) ;
#11132 = CIRCLE ( 'NONE', #22179, 26.80000000000000071 ) ;
#11133 = LINE ( 'NONE', #27964, #9643 ) ;
#11134 = DIRECTION ( 'NONE',  ( 1.000000000000000000, 0.000000000000000000, 0.000000000000000000 ) ) ;
#11135 = CARTESIAN_POINT ( 'NONE',  ( 8.700000000246973286, -27.86619909556666030, -31.29895010227025409 ) ) ;
#11136 = CARTESIAN_POINT ( 'NONE',  ( -17.78039861525124365, 10.42209091420443379, -1.400000000000001910 ) ) ;
#11137 = CARTESIAN_POINT ( 'NONE',  ( -5.649653782182448403, -1.974543963569185046, -49.92743646232499799 ) ) ;
#11138 = EDGE_CURVE ( 'NONE', #18457, #29946, #10039, .T. ) ;
#11139 = CARTESIAN_POINT ( 'NONE',  ( 14.40197535836999876, -22.00000000000000000, -25.51324865394999719 ) ) ;
#11140 = CARTESIAN_POINT ( 'NONE',  ( 18.26639035964474900, 11.02001161816309072, -1.000005633855494125E-09 ) ) ;
#11141 = DIRECTION ( 'NONE',  ( 5.962915006522623408E-16, 0.4383711467890811231, 0.8987940462991652613 ) ) ;
#11142 = CARTESIAN_POINT ( 'NONE',  ( -13.67718144140000014, 20.99999999999999645, -57.16242377749999548 ) ) ;
#11143 = ORIENTED_EDGE ( 'NONE', *, *, #255, .F. ) ;
#11144 = CARTESIAN_POINT ( 'NONE',  ( 2.384687176691703936, 5.016209330407524369, -33.15113063600001198 ) ) ;
#11145 = ORIENTED_EDGE ( 'NONE', *, *, #17385, .F. ) ;
#11146 = EDGE_CURVE ( 'NONE', #4569, #27858, #8115, .T. ) ;
#11147 = CARTESIAN_POINT ( 'NONE',  ( 0.9406167415608388538, 5.909121140422558760, -54.89500058692500062 ) ) ;
#11148 = ORIENTED_EDGE ( 'NONE', *, *, #6177, .T. ) ;
#11149 = EDGE_CURVE ( 'NONE', #6137, #27823, #13962, .T. ) ;
#11150 = AXIS2_PLACEMENT_3D ( 'NONE', #27074, #27224, #13202 ) ;
#11151 = VERTEX_POINT ( 'NONE', #27473 ) ;
#11152 = EDGE_LOOP ( 'NONE', ( #14461, #7383, #17475, #13258, #23927, #4305, #26630 ) ) ;
#11153 = AXIS2_PLACEMENT_3D ( 'NONE', #12385, #9565, #26406 ) ;
#11154 = CARTESIAN_POINT ( 'NONE',  ( -8.699999999945166707, -111.9817663798742444, 5.760339591697572814 ) ) ;
#11155 = LINE ( 'NONE', #26252, #7430 ) ;
#11156 = CARTESIAN_POINT ( 'NONE',  ( 1.243449787579999883E-14, -31.15538618883996946, -82.34631830372681804 ) ) ;
#11157 = CARTESIAN_POINT ( 'NONE',  ( 9.000000000000000000, -130.0000000000000000, -43.40000000074500264 ) ) ;
#11158 = DIRECTION ( 'NONE',  ( 0.9316362575375349842, -0.3633921898465292122, 0.000000000000000000 ) ) ;
#11159 = FACE_OUTER_BOUND ( 'NONE', #781, .T. ) ;
#11160 = CARTESIAN_POINT ( 'NONE',  ( -4.646804529178781173, -0.2974863596997279203, -4.148838774900000637 ) ) ;
#11161 = FACE_OUTER_BOUND ( 'NONE', #17872, .T. ) ;
#11162 = CARTESIAN_POINT ( 'NONE',  ( 1.002713911322309359, 3.977955482547946620, -17.55080441500000177 ) ) ;
#11163 = CARTESIAN_POINT ( 'NONE',  ( 4.417684705200791484, 4.247747620870205409, -35.32341724620000178 ) ) ;
#11164 = EDGE_CURVE ( 'NONE', #28749, #6979, #16755, .T. ) ;
#11165 = CONICAL_SURFACE ( 'NONE', #4630, 11.99999999999999467, 1.243158134259999770 ) ;
#11166 = CARTESIAN_POINT ( 'NONE',  ( 11.20000000009999930, -29.49999999969999820, -32.73012701900000110 ) ) ;
#11167 = CARTESIAN_POINT ( 'NONE',  ( 28.49528339128749366, 0.5184828350247816520, 0.7595836940000044724 ) ) ;
#11168 = CARTESIAN_POINT ( 'NONE',  ( 1.015231355539999880, -28.48218680760000154, 224.4935313260000100 ) ) ;
#11169 = CARTESIAN_POINT ( 'NONE',  ( 27.16374163455390089, -6.594387936805345518, 8.000000000000007105 ) ) ;
#11170 = CARTESIAN_POINT ( 'NONE',  ( -23.55406855550000245, 16.04544956020000157, 222.0000000000000000 ) ) ;
#11171 = CARTESIAN_POINT ( 'NONE',  ( 25.72310959295396771, 9.312057329535781136, -0.6999999999999784173 ) ) ;
#11172 = FACE_OUTER_BOUND ( 'NONE', #14025, .T. ) ;
#11173 = CARTESIAN_POINT ( 'NONE',  ( -0.5575288593901739365, -27.79459983365126163, 4.689815098000011062 ) ) ;
#11174 = ADVANCED_FACE ( 'NONE', ( #5312 ), #17946, .T. ) ;
#11175 = DIRECTION ( 'NONE',  ( 1.000000000000000000, -1.224606353819998843E-16, 0.000000000000000000 ) ) ;
#11176 = VERTEX_POINT ( 'NONE', #10501 ) ;
#11177 = CARTESIAN_POINT ( 'NONE',  ( -0.9795220552721649598, -3.499999999999999556, 227.7235171295581893 ) ) ;
#11178 = CARTESIAN_POINT ( 'NONE',  ( -24.60124998910000116, -12.94761260449999973, 224.7915656799999908 ) ) ;
#11179 = VECTOR ( 'NONE', #16446, 1000.000000000000114 ) ;
#11180 = CARTESIAN_POINT ( 'NONE',  ( 9.999999999963856467, -42.68965130474573755, -27.18132884639398839 ) ) ;
#11181 = ORIENTED_EDGE ( 'NONE', *, *, #458, .T. ) ;
#11182 = CARTESIAN_POINT ( 'NONE',  ( -2.036891525988612894, -5.569677580567498509, -43.98640794712500224 ) ) ;
#11183 = ORIENTED_EDGE ( 'NONE', *, *, #18852, .F. ) ;
#11184 = VERTEX_POINT ( 'NONE', #15371 ) ;
#11185 = ORIENTED_EDGE ( 'NONE', *, *, #19483, .F. ) ;
#11186 = CARTESIAN_POINT ( 'NONE',  ( 20.30396079662882158, 20.00000000004802203, 3.000000000000002665 ) ) ;
#11187 = EDGE_CURVE ( 'NONE', #15714, #10257, #16955, .T. ) ;
#11188 = ORIENTED_EDGE ( 'NONE', *, *, #10803, .F. ) ;
#11189 = AXIS2_PLACEMENT_3D ( 'NONE', #11869, #9509, #4331 ) ;
#11190 = CARTESIAN_POINT ( 'NONE',  ( -24.58975347950000057, -12.96948186770000078, 225.3106485179999936 ) ) ;
#11191 = PRODUCT_RELATED_PRODUCT_CATEGORY ( 'part', '', ( #3526 ) ) ;
#11192 = CARTESIAN_POINT ( 'NONE',  ( 8.000000000278095769, -14.92844969908619035, -33.25053330389217621 ) ) ;
#11193 = CARTESIAN_POINT ( 'NONE',  ( -3.628915872023533495, -3.418898166067736000, -94.44574089075830159 ) ) ;
#11194 = CARTESIAN_POINT ( 'NONE',  ( 14.71344982770164300, -22.00000000000000000, -26.84691114990011584 ) ) ;
#11195 = CARTESIAN_POINT ( 'NONE',  ( 23.28322851840398755, -13.27226524188811752, 6.100000000000007638 ) ) ;
#11196 = FACE_OUTER_BOUND ( 'NONE', #13662, .T. ) ;
#11197 = VERTEX_POINT ( 'NONE', #3402 ) ;
#11198 = CARTESIAN_POINT ( 'NONE',  ( 5.763395275750641922, -2.111988417859953504, -6.436105321699997717 ) ) ;
#11199 = CARTESIAN_POINT ( 'NONE',  ( 4.700333466414979178, 3.591691549163662511, -22.36727430110000725 ) ) ;
#11200 = CARTESIAN_POINT ( 'NONE',  ( -10.69999999930000101, -24.87867965640000278, -26.27867965640000136 ) ) ;
#11201 = EDGE_CURVE ( 'NONE', #931, #4165, #26519, .T. ) ;
#11202 = CARTESIAN_POINT ( 'NONE',  ( 25.22625794089999829, -13.26224522399999906, 224.8958210039999983 ) ) ;
#11203 = CARTESIAN_POINT ( 'NONE',  ( -0.9813161448799405662, 3.499840617129988285, 227.7241098089419893 ) ) ;
#11204 = DIRECTION ( 'NONE',  ( 1.000000000000000000, -1.844929437980039379E-12, 2.650555428735150365E-12 ) ) ;
#11205 = CARTESIAN_POINT ( 'NONE',  ( -23.88727024790000186, -14.22229899360000083, 226.0425106499999970 ) ) ;
#11206 = ADVANCED_FACE ( 'NONE', ( #27630 ), #28259, .T. ) ;
#11207 = B_SPLINE_CURVE_WITH_KNOTS ( 'NONE', 3,
 ( #24176, #21508, #14430, #13524, #23136, #26229 ),
 .UNSPECIFIED., .F., .F.,
 ( 4, 2, 4 ),
 ( 0.000000000000000000, 0.5000000000000000000, 1.000000000000000000 ),
 .UNSPECIFIED. ) ;
#11208 = CARTESIAN_POINT ( 'NONE',  ( 23.95771897998607969, -13.50170546740720035, 223.9280906791277062 ) ) ;
#11209 = CARTESIAN_POINT ( 'NONE',  ( 7.576768089039999765, -25.98941641389999901, 230.6999999999999886 ) ) ;
#11210 = CARTESIAN_POINT ( 'NONE',  ( -15.51200411779723254, -21.88251757794091290, -1.399999999999998357 ) ) ;
#11211 = ORIENTED_EDGE ( 'NONE', *, *, #12589, .F. ) ;
#11212 = CARTESIAN_POINT ( 'NONE',  ( 3.449241269337446791, -4.803451378176493591, -61.52197827312500067 ) ) ;
#11213 = VECTOR ( 'NONE', #8442, 1000.000000000000114 ) ;
#11214 = CARTESIAN_POINT ( 'NONE',  ( -23.97364091617425785, -15.41162529020582994, 5.735001241127421601 ) ) ;
#11215 = ORIENTED_EDGE ( 'NONE', *, *, #2619, .T. ) ;
#11216 = ADVANCED_FACE ( 'NONE', ( #6239 ), #13155, .F. ) ;
#11217 = CARTESIAN_POINT ( 'NONE',  ( 26.96724923820000086, 10.13406330579999803, 222.0000000000000000 ) ) ;
#11218 = CARTESIAN_POINT ( 'NONE',  ( 0.3233900739386466605, 6.101867874933233793, -22.94418644579999977 ) ) ;
#11219 = ORIENTED_EDGE ( 'NONE', *, *, #3875, .T. ) ;
#11220 = CARTESIAN_POINT ( 'NONE',  ( -25.00949650969999993, -13.66806287920000074, 225.9014032059999977 ) ) ;
#11221 = CARTESIAN_POINT ( 'NONE',  ( -3.393799910883221305, -2.010794396684639107, -68.10000000002500542 ) ) ;
#11222 = ORIENTED_EDGE ( 'NONE', *, *, #4176, .T. ) ;
#11223 = ORIENTED_EDGE ( 'NONE', *, *, #9204, .T. ) ;
#11224 = ORIENTED_EDGE ( 'NONE', *, *, #5724, .F. ) ;
#11225 = CARTESIAN_POINT ( 'NONE',  ( 3.103047163856258006, -2.814705343703844065, -96.08088653434137427 ) ) ;
#11226 = ORIENTED_EDGE ( 'NONE', *, *, #16574, .F. ) ;
#11227 = DIRECTION ( 'NONE',  ( -1.000000000000000000, 0.000000000000000000, 0.000000000000000000 ) ) ;
#11228 = CARTESIAN_POINT ( 'NONE',  ( 23.70578532274842942, -13.93854223037613238, 3.912293196490389757 ) ) ;
#11229 = CARTESIAN_POINT ( 'NONE',  ( -3.200877993934835075, 3.183711413074212349, -68.94322600112499799 ) ) ;
#11230 = AXIS2_PLACEMENT_3D ( 'NONE', #26121, #18562, #14159 ) ;
#11231 = CARTESIAN_POINT ( 'NONE',  ( -13.75032424559999988, -27.60893268290000080, 229.1414204800000221 ) ) ;
#11232 =( GEOMETRIC_REPRESENTATION_CONTEXT ( 3 ) GLOBAL_UNCERTAINTY_ASSIGNED_CONTEXT ( ( #18816 ) ) GLOBAL_UNIT_ASSIGNED_CONTEXT ( ( #26854, #25973, #23464 ) ) REPRESENTATION_CONTEXT ( 'NONE', 'WORKASPACE' ) );
#11233 = CARTESIAN_POINT ( 'NONE',  ( -0.6805610060751490220, -26.79155681327128491, 224.1233511992632828 ) ) ;
#11234 = CARTESIAN_POINT ( 'NONE',  ( -0.9536751402149999945, -27.93707515359999860, 222.0000000000000000 ) ) ;
#11235 = B_SPLINE_CURVE_WITH_KNOTS ( 'NONE', 5,
 ( #11757, #13810, #6414, #11606, #21203, #13969 ),
 .UNSPECIFIED., .F., .F.,
 ( 6, 6 ),
 ( -2.000000000000000000, 0.000000000000000000 ),
 .UNSPECIFIED. ) ;
#11236 = CARTESIAN_POINT ( 'NONE',  ( -17.45644675878112650, -23.80350462838311998, -24.47196394343449199 ) ) ;
#11237 = ORIENTED_EDGE ( 'NONE', *, *, #4999, .T. ) ;
#11238 = CARTESIAN_POINT ( 'NONE',  ( -9.999999999959999997, -24.87868334570000073, -26.27868334529999927 ) ) ;
#11239 = CARTESIAN_POINT ( 'NONE',  ( -1.657635364023947400, -6.345118362804027079, -11.95022317840000525 ) ) ;
#11240 = DIRECTION ( 'NONE',  ( 0.000000000000000000, 0.000000000000000000, 1.000000000000000000 ) ) ;
#11241 = EDGE_CURVE ( 'NONE', #28672, #11806, #1531, .T. ) ;
#11242 = DIRECTION ( 'NONE',  ( 0.000000000000000000, -2.255973186040000320E-12, -1.000000000000000000 ) ) ;
#11243 = VERTEX_POINT ( 'NONE', #11121 ) ;
#11244 = CARTESIAN_POINT ( 'NONE',  ( 4.041451884329999800, 2.701186720849999812E-16, 227.9588918784999976 ) ) ;
#11245 = CARTESIAN_POINT ( 'NONE',  ( 1.000415564564199444, -28.48292217093161938, 3.997481721999984750 ) ) ;
#11246 = CYLINDRICAL_SURFACE ( 'NONE', #10272, 26.80000000000002203 ) ;
#11247 = B_SPLINE_CURVE_WITH_KNOTS ( 'NONE', 3,
 ( #678, #24735, #29140, #3019, #15134, #8187 ),
 .UNSPECIFIED., .F., .F.,
 ( 4, 2, 4 ),
 ( 0.000000000000000000, 0.5000000000000000000, 1.000000000000000000 ),
 .UNSPECIFIED. ) ;
#11248 = CARTESIAN_POINT ( 'NONE',  ( 26.71513120331084679, 4.908099852734520319, 0.000000000000000000 ) ) ;
#11249 = CARTESIAN_POINT ( 'NONE',  ( 22.65536398230910820, -14.31703479027868831, 4.711904017054809657 ) ) ;
#11250 = EDGE_CURVE ( 'NONE', #25431, #18612, #19390, .T. ) ;
#11251 = CARTESIAN_POINT ( 'NONE',  ( -4.213298386699523945, 4.800796338101376293, -53.98587006832499924 ) ) ;
#11252 = FACE_OUTER_BOUND ( 'NONE', #5353, .T. ) ;
#11254 = EDGE_CURVE ( 'NONE', #14439, #2704, #5110, .T. ) ;
#11253 = CARTESIAN_POINT ( 'NONE',  ( 8.000000000248585152, -27.47644226431772907, -31.38783462175427630 ) ) ;
#11255 = VECTOR ( 'NONE', #18411, 1000.000000000000114 ) ;
#11256 = ORIENTED_EDGE ( 'NONE', *, *, #14423, .F. ) ;
#11257 = DIRECTION ( 'NONE',  ( -0.000000000000000000, 0.9128796883888952163, -0.4082287037029530552 ) ) ;
#11258 = CARTESIAN_POINT ( 'NONE',  ( -28.49999999979999998, 7.466149641079999455, 222.0000000000000000 ) ) ;
#11259 = TOROIDAL_SURFACE ( 'NONE', #28826, 30.50000000000000000, 3.000000000000000000 ) ;
#11260 = AXIS2_PLACEMENT_3D ( 'NONE', #26770, #5369, #7871 ) ;
#11261 = VECTOR ( 'NONE', #1081, 1000.000000000000000 ) ;
#11262 = AXIS2_PLACEMENT_3D ( 'NONE', #21070, #28291, #8942 ) ;
#11263 = CARTESIAN_POINT ( 'NONE',  ( 2.661374056126577514, -3.457594787124394831, -68.10000000002499121 ) ) ;
#11264 = CARTESIAN_POINT ( 'NONE',  ( -1.783682052191536638, -3.046043134539063946, -0.6999999999999784173 ) ) ;
#11265 = CARTESIAN_POINT ( 'NONE',  ( -4.322424737952120566, 1.108769406212976039, -44.10000000002499831 ) ) ;
#11266 = ORIENTED_EDGE ( 'NONE', *, *, #23823, .T. ) ;
#11267 = DIRECTION ( 'NONE',  ( 1.000000000000000000, -0.000000000000000000, -2.257150022439999944E-12 ) ) ;
#11268 = CARTESIAN_POINT ( 'NONE',  ( 3.415065912822992988, 4.318092861595879128, -64.43768011632499793 ) ) ;
#11269 = ORIENTED_EDGE ( 'NONE', *, *, #1416, .T. ) ;
#11270 = CARTESIAN_POINT ( 'NONE',  ( 7.453090060300315400, -2.907137518772522355, 202.0000000000000000 ) ) ;
#11271 = EDGE_LOOP ( 'NONE', ( #8708, #132, #28775, #11344 ) ) ;
#11272 = CARTESIAN_POINT ( 'NONE',  ( -20.26572724632349320, -21.15151735177849091, 0.9999999979999896205 ) ) ;
#11273 = ORIENTED_EDGE ( 'NONE', *, *, #29489, .F. ) ;
#11274 = AXIS2_PLACEMENT_3D ( 'NONE', #29310, #7757, #17359 ) ;
#11275 = EDGE_CURVE ( 'NONE', #3695, #22220, #14985, .T. ) ;
#11276 = AXIS2_PLACEMENT_3D ( 'NONE', #26845, #24797, #14897 ) ;
#11278 = EDGE_CURVE ( 'NONE', #18284, #25472, #22533, .T. ) ;
#11277 = AXIS2_PLACEMENT_3D ( 'NONE', #14206, #12305, #2254 ) ;
#11279 = CARTESIAN_POINT ( 'NONE',  ( -13.00000000000000000, 21.72305290929948640, -60.97178489257708378 ) ) ;
#11280 = CARTESIAN_POINT ( 'NONE',  ( -28.08055191791969563, 6.526239597828547900, 8.000000000000007105 ) ) ;
#11281 = VECTOR ( 'NONE', #2239, 1000.000000000000000 ) ;
#11282 = VECTOR ( 'NONE', #464, 999.9999999999998863 ) ;
#11283 = CARTESIAN_POINT ( 'NONE',  ( 0.000000000000000000, 0.000000000000000000, 230.6999999999999886 ) ) ;
#11284 = CARTESIAN_POINT ( 'NONE',  ( 10.69999999989999928, -25.00000000000000000, -4.837481085799996805 ) ) ;
#11285 = DIRECTION ( 'NONE',  ( -6.326189572192214457E-12, -0.3568421334038989756, 0.9341647027306019258 ) ) ;
#11286 = VERTEX_POINT ( 'NONE', #4191 ) ;
#11287 = FACE_BOUND ( 'NONE', #27546, .T. ) ;
#11288 = DIRECTION ( 'NONE',  ( 0.000000000000000000, 0.000000000000000000, -1.000000000000000000 ) ) ;
#11289 = CARTESIAN_POINT ( 'NONE',  ( 19.80537707599999919, 19.50874960799999869, 229.0000000010000178 ) ) ;
#11290 = CARTESIAN_POINT ( 'NONE',  ( -3.509522867613010355, 0.9213280829735164268, 230.7624477058855632 ) ) ;
#11291 = CARTESIAN_POINT ( 'NONE',  ( -24.55841378230000061, -14.46270012129999927, 226.0798679369999888 ) ) ;
#11292 = LINE ( 'NONE', #20896, #30103 ) ;
#11293 = CARTESIAN_POINT ( 'NONE',  ( 12.12499559729999810, 21.69999999929999390, -55.73512174120000395 ) ) ;
#11294 = CARTESIAN_POINT ( 'NONE',  ( -16.38556888388364641, 9.985034189104762703, -1.400000000000002132 ) ) ;
#11295 = CARTESIAN_POINT ( 'NONE',  ( 4.421972129926214023, 1.961202595004077232, -51.47998794302500158 ) ) ;
#11296 = CARTESIAN_POINT ( 'NONE',  ( -0.6215321085541587465, 3.500000000000000000, 230.8123217011518022 ) ) ;
#11297 = CARTESIAN_POINT ( 'NONE',  ( 8.999999999799992878, 20.99999999999851497, -51.75449846949787513 ) ) ;
#11298 = CARTESIAN_POINT ( 'NONE',  ( 14.84482701754090606, -29.21177333770954476, -32.89653475988580311 ) ) ;
#11299 = DIRECTION ( 'NONE',  ( -1.000000000000000000, 0.000000000000000000, 0.000000000000000000 ) ) ;
#11300 = AXIS2_PLACEMENT_3D ( 'NONE', #1780, #23651, #26157 ) ;
#11301 = CIRCLE ( 'NONE', #28882, 3.200000004570001888 ) ;
#11302 = CARTESIAN_POINT ( 'NONE',  ( -12.12499970530000049, 21.69999999919999212, -55.73512393530000253 ) ) ;
#11303 = ORIENTED_EDGE ( 'NONE', *, *, #23615, .F. ) ;
#11304 = CARTESIAN_POINT ( 'NONE',  ( -23.74375282219999761, -14.46070769699999836, 224.0986003170000060 ) ) ;
#11305 = ORIENTED_EDGE ( 'NONE', *, *, #29371, .F. ) ;
#11306 = EDGE_CURVE ( 'NONE', #28246, #8650, #8835, .T. ) ;
#11307 = CARTESIAN_POINT ( 'NONE',  ( -1.293561172433232986, -6.216321778783836294, -53.40706695232499612 ) ) ;
#11308 = EDGE_LOOP ( 'NONE', ( #23966, #10706, #20996, #15937 ) ) ;
#11309 = APPLICATION_PROTOCOL_DEFINITION ( 'draft international standard', 'automotive_design', 1998, #2139 ) ;
#11310 = ORIENTED_EDGE ( 'NONE', *, *, #29248, .T. ) ;
#11311 = DIRECTION ( 'NONE',  ( -1.000000000000000000, 1.662859514859999923E-15, -6.790296706416999781E-12 ) ) ;
#11312 = ORIENTED_EDGE ( 'NONE', *, *, #24288, .F. ) ;
#11313 = AXIS2_PLACEMENT_3D ( 'NONE', #7969, #8587, #13007 ) ;
#11314 = CARTESIAN_POINT ( 'NONE',  ( 14.78499923084727286, -30.41584920728202235, -24.59895335003452743 ) ) ;
#11315 = EDGE_CURVE ( 'NONE', #13930, #5717, #8049, .T. ) ;
#11316 = DIRECTION ( 'NONE',  ( 1.000000000000000000, -1.843431230200084908E-12, 2.650498504963248473E-12 ) ) ;
#11317 = CARTESIAN_POINT ( 'NONE',  ( 3.550686850769999806E-05, -28.50022181210000127, 226.1000014189999945 ) ) ;
#11318 = CARTESIAN_POINT ( 'NONE',  ( -11.83960380690193404, -32.88057757210000176, -29.59113702762771680 ) ) ;
#11319 = CARTESIAN_POINT ( 'NONE',  ( 10.69999999999999929, -130.0000000000000000, -41.82335799894999440 ) ) ;
#11320 = CARTESIAN_POINT ( 'NONE',  ( -4.528911865900279388, -2.588562295002507785, -0.6999999999999992895 ) ) ;
#11321 = CARTESIAN_POINT ( 'NONE',  ( -5.885952403586735215, -0.3768160556055083488, -3.148838774900004189 ) ) ;
#11322 = CARTESIAN_POINT ( 'NONE',  ( 26.01645409420000021, -14.91014372119999898, 229.4982322489999831 ) ) ;
#11323 = EDGE_LOOP ( 'NONE', ( #20498, #23449, #1995, #23191 ) ) ;
#11324 = CARTESIAN_POINT ( 'NONE',  ( 8.000000000462277328, -18.10926874255784469, -36.88339488450507986 ) ) ;
#11325 = CIRCLE ( 'NONE', #5782, 28.50000000000000000 ) ;
#11326 = CARTESIAN_POINT ( 'NONE',  ( -5.420006065778396831, -1.021773059489365032, -17.09949426530000238 ) ) ;
#11327 = CARTESIAN_POINT ( 'NONE',  ( -3.850850186879767545, -3.402327863231305205, -32.89697003410000065 ) ) ;
#11328 = CARTESIAN_POINT ( 'NONE',  ( -0.9003584927496220969, -26.78512143699428094, 5.633487050009015285 ) ) ;
#11329 = CARTESIAN_POINT ( 'NONE',  ( 0.4821455017210000138, -28.49635764770000179, 223.9974824469999817 ) ) ;
#11330 = CARTESIAN_POINT ( 'NONE',  ( -28.47941833768584985, -1.391725289281258160, 8.000000000000007105 ) ) ;
#11331 = CARTESIAN_POINT ( 'NONE',  ( -25.47204932480000039, 13.22994448760000097, 222.0000000000000000 ) ) ;
#11332 = CARTESIAN_POINT ( 'NONE',  ( 28.35455043824866550, 0.5159221438580620100, 0.2374258030000131470 ) ) ;
#11333 = CARTESIAN_POINT ( 'NONE',  ( -3.458129700889219116, 0.5397582531354577773, 226.6412452697749984 ) ) ;
#11334 = DIRECTION ( 'NONE',  ( -1.000000000000000000, 0.000000000000000000, 0.000000000000000000 ) ) ;
#11335 = AXIS2_PLACEMENT_3D ( 'NONE', #21252, #28784, #25980 ) ;
#11336 = ADVANCED_FACE ( 'NONE', ( #12158 ), #7743, .F. ) ;
#11337 = CARTESIAN_POINT ( 'NONE',  ( 27.50000000000000000, -3.367667472999999580E-15, 65.00000000000000000 ) ) ;
#11338 = ORIENTED_EDGE ( 'NONE', *, *, #4593, .T. ) ;
#11339 = CARTESIAN_POINT ( 'NONE',  ( 17.93011078763067090, 11.79183908526299085, 0.000000000000000000 ) ) ;
#11340 = CARTESIAN_POINT ( 'NONE',  ( -23.77307140041805411, 14.41181874028064591, 4.999998581000003384 ) ) ;
#11341 = CARTESIAN_POINT ( 'NONE',  ( 0.6479068412426576273, -26.79235971056621324, 4.090187300791521707 ) ) ;
#11342 = ORIENTED_EDGE ( 'NONE', *, *, #19160, .F. ) ;
#11343 = CARTESIAN_POINT ( 'NONE',  ( -10.00000000057973359, -129.9999999999998010, -39.98135228930375007 ) ) ;
#11344 = ORIENTED_EDGE ( 'NONE', *, *, #19314, .F. ) ;
#11345 = ORIENTED_EDGE ( 'NONE', *, *, #14233, .T. ) ;
#11346 = ORIENTED_EDGE ( 'NONE', *, *, #1348, .T. ) ;
#11347 = CARTESIAN_POINT ( 'NONE',  ( 3.372732847734490225, -1.748957314603980739, -35.69999999999999574 ) ) ;
#11348 = ORIENTED_EDGE ( 'NONE', *, *, #24567, .F. ) ;
#11349 = CARTESIAN_POINT ( 'NONE',  ( -24.68204616399999907, -14.25020164319999871, 226.1000014189999945 ) ) ;
#11350 = SURFACE_SIDE_STYLE ('',( #27553 ) ) ;
#11351 = EDGE_CURVE ( 'NONE', #15903, #6922, #9965, .T. ) ;
#11352 = CARTESIAN_POINT ( 'NONE',  ( -24.49999999589999788, 3.000285566369999841E-15, 40.00000000000000000 ) ) ;
#11353 = CARTESIAN_POINT ( 'NONE',  ( -10.00000000020000002, -28.65356604289999964, -25.83278327859999735 ) ) ;
#11354 = DIRECTION ( 'NONE',  ( -1.000000000000000000, 0.000000000000000000, 0.000000000000000000 ) ) ;
#11355 = CARTESIAN_POINT ( 'NONE',  ( 14.72842623554610419, -21.99999999999999645, -26.93849963251682311 ) ) ;
#11356 = CARTESIAN_POINT ( 'NONE',  ( 23.73988890810274910, -12.43614388128991877, 5.145878552484940194 ) ) ;
#11357 = CARTESIAN_POINT ( 'NONE',  ( 12.55799324160000019, 21.70000000000000284, -55.95247857500000066 ) ) ;
#11358 = VERTEX_POINT ( 'NONE', #6701 ) ;
#11359 = CARTESIAN_POINT ( 'NONE',  ( -4.273751495587445604, 4.364932658710685587, -5.168732180600002835 ) ) ;
#11360 = CARTESIAN_POINT ( 'NONE',  ( 4.275653884846098762, -3.504702130532165505, -22.99674734060000958 ) ) ;
#11361 = CARTESIAN_POINT ( 'NONE',  ( -8.986416953306164856, -25.99194954040540040, 206.0369953409331174 ) ) ;
#11362 = CARTESIAN_POINT ( 'NONE',  ( 23.67414648230973739, -12.56096907828687392, 225.5575347054845281 ) ) ;
#11363 = EDGE_CURVE ( 'NONE', #5989, #10856, #1999, .T. ) ;
#11364 = CARTESIAN_POINT ( 'NONE',  ( -0.3140692933633429940, 3.500175508921068435, 227.6463701859492517 ) ) ;
#11365 = CARTESIAN_POINT ( 'NONE',  ( 6.000000000000000000, -29.96004123392021157, -79.78289277550334191 ) ) ;
#11366 = CARTESIAN_POINT ( 'NONE',  ( -24.10559463919999956, -15.20494734660000091, 225.2084356629999888 ) ) ;
#11367 = EDGE_CURVE ( 'NONE', #27091, #21618, #10356, .T. ) ;
#11368 = FACE_BOUND ( 'NONE', #18095, .T. ) ;
#11369 = CARTESIAN_POINT ( 'NONE',  ( 0.5057536231481117861, -27.79562098839016571, 6.099998581000020792 ) ) ;
#11370 = CARTESIAN_POINT ( 'NONE',  ( -17.93590711828372974, 11.12626540400258790, -0.6999999999999784173 ) ) ;
#11371 = ORIENTED_EDGE ( 'NONE', *, *, #18688, .F. ) ;
#11372 = CARTESIAN_POINT ( 'NONE',  ( -1.231152431062140007, -5.073857922501755269, -61.19311227092500616 ) ) ;
#11373 = CARTESIAN_POINT ( 'NONE',  ( -24.92013865347427171, 13.82966157970119525, 6.099998581000020792 ) ) ;
#11374 = ORIENTED_EDGE ( 'NONE', *, *, #6563, .T. ) ;
#11375 = ORIENTED_EDGE ( 'NONE', *, *, #3232, .T. ) ;
#11376 = EDGE_CURVE ( 'NONE', #1757, #8590, #16303, .T. ) ;
#11377 = DIRECTION ( 'NONE',  ( 0.000000000000000000, 0.000000000000000000, -1.000000000000000000 ) ) ;
#11378 = CARTESIAN_POINT ( 'NONE',  ( 5.503465972401561324, -2.627571514393519436, -20.88180150029999993 ) ) ;
#11379 = VERTEX_POINT ( 'NONE', #21767 ) ;
#11380 = CARTESIAN_POINT ( 'NONE',  ( -23.77307140041805411, 14.41181874028064591, 4.999998581000003384 ) ) ;
#11381 = CARTESIAN_POINT ( 'NONE',  ( -3.862012131226881806, -1.085429931028346395, -68.10000000002500542 ) ) ;
#11382 = ORIENTED_EDGE ( 'NONE', *, *, #16930, .T. ) ;
#11383 = ORIENTED_EDGE ( 'NONE', *, *, #673, .T. ) ;
#11384 = ORIENTED_EDGE ( 'NONE', *, *, #9836, .T. ) ;
#11385 = FACE_OUTER_BOUND ( 'NONE', #7287, .T. ) ;
#11386 = SURFACE_STYLE_FILL_AREA ( #15945 ) ;
#11387 = ORIENTED_EDGE ( 'NONE', *, *, #24498, .F. ) ;
#11388 = CARTESIAN_POINT ( 'NONE',  ( -12.30000000002208438, -26.58112097952136565, -31.60000000001083365 ) ) ;
#11389 = EDGE_CURVE ( 'NONE', #22717, #23873, #225, .T. ) ;
#11390 = CARTESIAN_POINT ( 'NONE',  ( -25.46368746804859740, 12.80129684245613575, 4.999998581000003384 ) ) ;
#11391 = CARTESIAN_POINT ( 'NONE',  ( -5.434147616959247529, -3.211087428728324866, -68.32382590962500046 ) ) ;
#11392 = CARTESIAN_POINT ( 'NONE',  ( -23.81866442513186755, -14.33570206443695838, 3.899998581000013509 ) ) ;
#11393 = DIRECTION ( 'NONE',  ( 0.000000000000000000, -1.000000000000000000, 0.000000000000000000 ) ) ;
#11394 = CARTESIAN_POINT ( 'NONE',  ( -25.53422772419999731, -11.61914357240000051, 222.0000000000000000 ) ) ;
#11395 = CARTESIAN_POINT ( 'NONE',  ( -23.73992238018677980, -12.43607998452291774, 5.097059004422684225 ) ) ;
#11396 = VERTEX_POINT ( 'NONE', #10120 ) ;
#11397 = ADVANCED_FACE ( 'NONE', ( #19247 ), #14689, .F. ) ;
#11398 = CARTESIAN_POINT ( 'NONE',  ( -23.13685276725654916, -13.52579547987099140, 226.1000000000000227 ) ) ;
#11399 = CARTESIAN_POINT ( 'NONE',  ( -5.517889265940039145, -2.627421812126006451, -12.97655742010000246 ) ) ;
#11400 = CARTESIAN_POINT ( 'NONE',  ( 26.62724484483131349, -3.508068424019962883, 136.7828584120000528 ) ) ;
#11401 = CARTESIAN_POINT ( 'NONE',  ( 10.52451969703728096, -6.422810664934133662, 232.6627636643594599 ) ) ;
#11402 = EDGE_LOOP ( 'NONE', ( #16636, #29922, #24546, #26731 ) ) ;
#11403 = DIRECTION ( 'NONE',  ( 1.000000000000000000, 0.000000000000000000, 0.000000000000000000 ) ) ;
#11404 = CARTESIAN_POINT ( 'NONE',  ( -10.69999999999999929, -128.0330808734999835, -35.24741685077000142 ) ) ;
#11405 = CARTESIAN_POINT ( 'NONE',  ( 24.93720649360215802, -13.79881813812812297, 3.899998581000013509 ) ) ;
#11406 = CARTESIAN_POINT ( 'NONE',  ( 6.984668861240829862, -26.60192251835760402, 21.60853132520131936 ) ) ;
#11407 = CARTESIAN_POINT ( 'NONE',  ( 11.59065746419999954, -24.20066399999999973, -1.404983722799999057 ) ) ;
#11408 = CARTESIAN_POINT ( 'NONE',  ( 2.137930486642451555, 6.059703978454344941, -45.49079303332499791 ) ) ;
#11409 = CARTESIAN_POINT ( 'NONE',  ( 26.80000000000000071, 4.525613202499999765, 230.0000000000000000 ) ) ;
#11410 = CARTESIAN_POINT ( 'NONE',  ( 10.69999999997749640, -124.7625450005068615, -32.43068487539576950 ) ) ;
#11411 = VERTEX_POINT ( 'NONE', #22081 ) ;
#11412 = DIRECTION ( 'NONE',  ( 0.3633921898465272138, -0.9316362575375356503, -1.850371707708593498E-14 ) ) ;
#11413 = B_SPLINE_CURVE_WITH_KNOTS ( 'NONE', 3,
 ( #16847, #24097, #14349, #2231, #18900, #11825 ),
 .UNSPECIFIED., .F., .F.,
 ( 4, 2, 4 ),
 ( 0.000000000000000000, 0.5000000000000000000, 1.000000000000000000 ),
 .UNSPECIFIED. ) ;
#11414 = CARTESIAN_POINT ( 'NONE',  ( 1.880866539809174398, -3.711827103239287329, -68.10000000002501963 ) ) ;
#11415 = PRODUCT_DEFINITION_SHAPE ( 'NONE', 'NONE',  #2358 ) ;
#11416 = AXIS2_PLACEMENT_3D ( 'NONE', #24273, #9960, #2269 ) ;
#11417 = CARTESIAN_POINT ( 'NONE',  ( -2.813577582307066560, -2.131591337269397979, -0.6999999999999784173 ) ) ;
#11418 = CARTESIAN_POINT ( 'NONE',  ( -4.160135742341998899, 0.1489380525860333204, -44.10000000002499121 ) ) ;
#11419 = SHAPE_REPRESENTATION_RELATIONSHIP ( 'NONE' , 'NONE' ,  #22833, #2064 ) ;
#11420 = ORIENTED_EDGE ( 'NONE', *, *, #29712, .T. ) ;
#11421 = LINE ( 'NONE', #16291, #17470 ) ;
#11422 = EDGE_CURVE ( 'NONE', #26986, #49, #24277, .T. ) ;
#11423 = MECHANICAL_DESIGN_GEOMETRIC_PRESENTATION_REPRESENTATION (  '', ( #869 ), #1877 ) ;
#11424 = CARTESIAN_POINT ( 'NONE',  ( 1.165515511296630446, -4.760067307266074188, -65.45397119102499062 ) ) ;
#11425 = ORIENTED_EDGE ( 'NONE', *, *, #25216, .T. ) ;
#11426 = PLANE ( 'NONE',  #1379 ) ;
#11427 = EDGE_CURVE ( 'NONE', #3166, #18608, #15577, .T. ) ;
#11428 = ADVANCED_FACE ( 'NONE', ( #16880 ), #14849, .F. ) ;
#11429 = CARTESIAN_POINT ( 'NONE',  ( -20.26572724641438228, -21.15151735228022645, 0.8585790890000000175 ) ) ;
#11430 = ORIENTED_EDGE ( 'NONE', *, *, #284, .T. ) ;
#11431 = LINE ( 'NONE', #30480, #19573 ) ;
#11432 = DIRECTION ( 'NONE',  ( 1.000000000000000000, -1.843431230200084908E-12, 2.650498504963248473E-12 ) ) ;
#11433 = CARTESIAN_POINT ( 'NONE',  ( 9.929578881719999472, 19.99999999999999645, -42.78784606711000293 ) ) ;
#11434 = CARTESIAN_POINT ( 'NONE',  ( -2.611298560087381038, 2.373819477306434500, 0.000000000000000000 ) ) ;
#11435 = B_SPLINE_SURFACE_WITH_KNOTS ( 'NONE', 5, 1, ( 
 ( #30683, #15892 ),
 ( #25495, #26723 ),
 ( #2508, #4555 ),
 ( #9585, #28626 ),
 ( #5161, #16508 ),
 ( #7223, #11637 ),
 ( #23762, #26118 ),
 ( #23922, #12095 ),
 ( #24069, #26576 ),
 ( #21550, #21399 ),
 ( #254, #24213 ),
 ( #16969, #153 ),
 ( #14321, #21703 ),
 ( #17123, #23611 ),
 ( #16813, #9733 ) ),
 .UNSPECIFIED., .F., .F., .F.,
 ( 6, 3, 3, 3, 6 ),
 ( 2, 2 ),
 ( 0.000000000000000000, 0.5778102094429999891, 1.155620418890000112, 2.022335733049999806, 2.889051047220000168 ),
 ( -3.133915349450000281E-11, 0.7031437918980000257 ),
 .UNSPECIFIED. ) ;
#11436 = DIRECTION ( 'NONE',  ( -1.000000000000000000, 5.687697913153403713E-16, -6.771501495041734442E-12 ) ) ;
#11437 = AXIS2_PLACEMENT_3D ( 'NONE', #3918, #20751, #29725 ) ;
#11438 = CARTESIAN_POINT ( 'NONE',  ( -12.40388755361936468, -22.00000000000000000, -29.70864971667464971 ) ) ;
#11439 = CARTESIAN_POINT ( 'NONE',  ( 10.69999999989999928, 19.99999999999999645, -2.399999999999999467 ) ) ;
#11440 = EDGE_LOOP ( 'NONE', ( #17400, #10672, #7933, #23322, #11733, #2409 ) ) ;
#11441 = CARTESIAN_POINT ( 'NONE',  ( -1.331528626038261054, -3.699456877748816375, -44.10000000002499121 ) ) ;
#11442 = CARTESIAN_POINT ( 'NONE',  ( -1.482055586095422983, 0.2313249656292047651, 231.6412452697749984 ) ) ;
#11443 = CARTESIAN_POINT ( 'NONE',  ( 19.80537707610000098, 19.50874960790000046, 229.0739602739999725 ) ) ;
#11444 = AXIS2_PLACEMENT_3D ( 'NONE', #16378, #9293, #30704 ) ;
#11445 = CARTESIAN_POINT ( 'NONE',  ( -2.572901307054817011, 2.543604213323934271, 230.7685035973561583 ) ) ;
#11446 = CARTESIAN_POINT ( 'NONE',  ( -7.999999999717977595, -23.99023929173318948, -28.09088343939654209 ) ) ;
#11447 = MANIFOLD_SOLID_BREP ( 'PartBody', #8015 ) ;
#11448 = CARTESIAN_POINT ( 'NONE',  ( 7.877322421339998826, -9.296057209400000687, 230.6412452697800006 ) ) ;
#11449 = AXIS2_PLACEMENT_3D ( 'NONE', #7744, #18819, #15145 ) ;
#11450 = CARTESIAN_POINT ( 'NONE',  ( 8.700000000249984211, -26.29631921959126117, -31.34262568600063759 ) ) ;
#11451 = DIRECTION ( 'NONE',  ( 0.000000000000000000, 1.000000000000000000, 0.000000000000000000 ) ) ;
#11452 = CARTESIAN_POINT ( 'NONE',  ( -4.185672079393978784, 2.483218523716627768, -50.83267869292499341 ) ) ;
#11453 = CARTESIAN_POINT ( 'NONE',  ( -23.81569860410000317, -13.75000000000000000, 6.099999999630000502 ) ) ;
#11454 = CARTESIAN_POINT ( 'NONE',  ( 5.114250173089999407, 17.43050732989999929, 231.6999999999999886 ) ) ;
#11455 = FACE_OUTER_BOUND ( 'NONE', #22678, .T. ) ;
#11456 = AXIS2_PLACEMENT_3D ( 'NONE', #7077, #14329, #1480 ) ;
#11457 = CARTESIAN_POINT ( 'NONE',  ( -17.59696597926837214, -9.791839085300418688, -0.6999999989999727834 ) ) ;
#11458 = CARTESIAN_POINT ( 'NONE',  ( 3.123710955063051298, -2.074832491810060020, -35.95875473020000612 ) ) ;
#11459 = VECTOR ( 'NONE', #28062, 1000.000000000000114 ) ;
#11460 = ORIENTED_EDGE ( 'NONE', *, *, #64, .T. ) ;
#11461 = CARTESIAN_POINT ( 'NONE',  ( -4.803332065605933288, -2.627392435372716495, -54.14982952342499800 ) ) ;
#11462 = VERTEX_POINT ( 'NONE', #11647 ) ;
#11463 = AXIS2_PLACEMENT_3D ( 'NONE', #5869, #15479, #1323 ) ;
#11464 = VERTEX_POINT ( 'NONE', #11951 ) ;
#11466 = CARTESIAN_POINT ( 'NONE',  ( -17.40256142132136929, -30.59124499734533131, -32.10008654271492645 ) ) ;
#11465 = VECTOR ( 'NONE', #2433, 1000.000000000000000 ) ;
#11467 = ADVANCED_FACE ( 'NONE', ( #23619 ), #26041, .T. ) ;
#11468 = EDGE_LOOP ( 'NONE', ( #27974, #22177, #6846, #10121 ) ) ;
#11469 = CARTESIAN_POINT ( 'NONE',  ( -8.699999999970339459, -115.7892272537997371, 9.034522706526081137 ) ) ;
#11470 = CARTESIAN_POINT ( 'NONE',  ( 4.638687372223565752, -11.03139726556875999, -35.43660304871379907 ) ) ;
#11471 = DIRECTION ( 'NONE',  ( 0.000000000000000000, 0.000000000000000000, 1.000000000000000000 ) ) ;
#11472 = CARTESIAN_POINT ( 'NONE',  ( -5.359734053730000447, -10.98902024870000105, 232.6627648150000027 ) ) ;
#11473 = DIRECTION ( 'NONE',  ( 3.868433351431744750E-13, -0.9784859933254772546, -0.2063132590645932463 ) ) ;
#11474 = DIRECTION ( 'NONE',  ( 0.000000000000000000, 1.000000000000000000, 0.000000000000000000 ) ) ;
#11475 = CARTESIAN_POINT ( 'NONE',  ( -3.885731905334990799, 2.027028853511393613, -1.418764356299999418 ) ) ;
#11476 = CARTESIAN_POINT ( 'NONE',  ( 5.135309658569999769, -30.28532181790000166, 230.6577119970000069 ) ) ;
#11477 = ORIENTED_EDGE ( 'NONE', *, *, #1690, .T. ) ;
#11478 = CARTESIAN_POINT ( 'NONE',  ( 25.20441738229720485, -13.30520055401376922, 5.965619088697175165 ) ) ;
#11479 = CIRCLE ( 'NONE', #11003, 4.276011752367103291 ) ;
#11480 = CARTESIAN_POINT ( 'NONE',  ( 1.270104287659547859, 5.038743611242932907, -18.05080441500000532 ) ) ;
#11481 = CARTESIAN_POINT ( 'NONE',  ( 6.465364827590567742, 5.909465029206098841, -40.36140784685665750 ) ) ;
#11482 = CARTESIAN_POINT ( 'NONE',  ( -0.6479069172523121978, -26.79235980091754143, 5.909812225168041167 ) ) ;
#11483 = CARTESIAN_POINT ( 'NONE',  ( 3.550686846709999450E-05, -28.50022181210000127, 223.9000014189999774 ) ) ;
#11484 = CARTESIAN_POINT ( 'NONE',  ( -7.999999999628359504, -14.95611408987656965, -40.37595097054163773 ) ) ;
#11485 = CARTESIAN_POINT ( 'NONE',  ( -17.38968115012163196, -28.33218551802936602, -33.40436502465443169 ) ) ;
#11486 = CARTESIAN_POINT ( 'NONE',  ( 26.91640669801677177, 9.744044393141841454, -0.2432540810000105580 ) ) ;
#11487 = CARTESIAN_POINT ( 'NONE',  ( 8.700000000289719537, -13.99335427294626832, -37.12410235030684902 ) ) ;
#11488 = CARTESIAN_POINT ( 'NONE',  ( -10.35667741062608371, -26.55163333981974816, 140.0000000000000000 ) ) ;
#11489 = TOROIDAL_SURFACE ( 'NONE', #31078, 24.50000000000000000, 4.000000000000000000 ) ;
#11490 = EDGE_CURVE ( 'NONE', #17095, #11806, #14488, .T. ) ;
#11491 = CARTESIAN_POINT ( 'NONE',  ( -25.46368746804859740, 12.80129684245613575, 4.999998581000003384 ) ) ;
#11492 = VERTEX_POINT ( 'NONE', #18134 ) ;
#11493 = CARTESIAN_POINT ( 'NONE',  ( -10.92440694859999972, 19.99999999999999645, -0.8628532294999990970 ) ) ;
#11494 = CARTESIAN_POINT ( 'NONE',  ( 1.018915990056934673, -26.78112376029977426, 4.579415541090104291 ) ) ;
#11495 = ORIENTED_EDGE ( 'NONE', *, *, #3659, .T. ) ;
#11496 = CARTESIAN_POINT ( 'NONE',  ( -4.592700181227117540, -1.655560342997611123, -44.81497819512500058 ) ) ;
#11497 = ORIENTED_EDGE ( 'NONE', *, *, #26958, .F. ) ;
#11498 = VERTEX_POINT ( 'NONE', #9273 ) ;
#11499 = VECTOR ( 'NONE', #5150, 1000.000000000000000 ) ;
#11500 = ORIENTED_EDGE ( 'NONE', *, *, #20430, .T. ) ;
#11501 = LINE ( 'NONE', #18420, #18490 ) ;
#11502 = VERTEX_POINT ( 'NONE', #18295 ) ;
#11503 = CARTESIAN_POINT ( 'NONE',  ( 7.368918569919999939, 16.61433718970000228, 230.6999999999999886 ) ) ;
#11504 = DIRECTION ( 'NONE',  ( 0.000000000000000000, 0.000000000000000000, 1.000000000000000000 ) ) ;
#11505 = CARTESIAN_POINT ( 'NONE',  ( -24.16679028379773797, -15.10730798416152609, 3.997250019000003540 ) ) ;
#11506 = CARTESIAN_POINT ( 'NONE',  ( 0.000000000000000000, 0.000000000000000000, 190.0000000000000000 ) ) ;
#11507 = CARTESIAN_POINT ( 'NONE',  ( -0.5968465743326634154, -28.49391676915515603, 4.791896188000022150 ) ) ;
#11508 = VECTOR ( 'NONE', #1694, 1000.000000000000114 ) ;
#11509 = CARTESIAN_POINT ( 'NONE',  ( 14.81428820541019142, -22.00000000000000711, -27.51054546844379445 ) ) ;
#11510 = CARTESIAN_POINT ( 'NONE',  ( -24.08673398027933388, -11.88135228261326226, -0.000000000000000000 ) ) ;
#11511 = EDGE_CURVE ( 'NONE', #2408, #17004, #16476, .T. ) ;
#11512 = CARTESIAN_POINT ( 'NONE',  ( -18.41918783629999723, 20.00000925869999691, 230.6632488119999778 ) ) ;
#11513 = EDGE_LOOP ( 'NONE', ( #23744, #831, #16675, #1754 ) ) ;
#11514 = CARTESIAN_POINT ( 'NONE',  ( 3.194067125856711264, 4.998308969841025906, -6.200967428500008261 ) ) ;
#11515 = CARTESIAN_POINT ( 'NONE',  ( -4.555585884337687297, -4.059738318096004939, -24.84101932450000305 ) ) ;
#11516 = CARTESIAN_POINT ( 'NONE',  ( -4.963640651960628425, -9.105767507093087687, -102.7632020892250040 ) ) ;
#11517 = CARTESIAN_POINT ( 'NONE',  ( -3.388043077342722142, -1.111846212892217522, -88.52261276308685467 ) ) ;
#11518 = DIRECTION ( 'NONE',  ( 0.000000000000000000, -1.000000000000000000, 2.257145581549999994E-12 ) ) ;
#11519 = DIRECTION ( 'NONE',  ( 0.000000000000000000, 0.000000000000000000, -1.000000000000000000 ) ) ;
#11520 = CARTESIAN_POINT ( 'NONE',  ( -2.017871889752692383, -3.161030873707806332, -0.6999999999999992895 ) ) ;
#11521 = EDGE_CURVE ( 'NONE', #20223, #21635, #10912, .T. ) ;
#11522 = VECTOR ( 'NONE', #9067, 1000.000000000000000 ) ;
#11523 = DIRECTION ( 'NONE',  ( 1.000000000000000000, 0.000000000000000000, 0.000000000000000000 ) ) ;
#11524 = CARTESIAN_POINT ( 'NONE',  ( -16.04158896040112126, -9.763537949678049443, 0.000000000000000000 ) ) ;
#11525 = CARTESIAN_POINT ( 'NONE',  ( -10.00000000054610005, -24.99999999999988987, -8.540325878496638268 ) ) ;
#11526 = ORIENTED_EDGE ( 'NONE', *, *, #22370, .T. ) ;
#11527 = CARTESIAN_POINT ( 'NONE',  ( -0.9941633020186212422, 5.428540911361258381, -59.45324387862500259 ) ) ;
#11528 = CARTESIAN_POINT ( 'NONE',  ( -25.84755624059999946, 9.037785233839999322, 230.0000000000000000 ) ) ;
#11529 = ADVANCED_FACE ( 'NONE', ( #13418 ), #28476, .F. ) ;
#11530 = EDGE_LOOP ( 'NONE', ( #21155, #785, #23397, #24693 ) ) ;
#11531 = DIRECTION ( 'NONE',  ( -0.9316362575375349842, 0.3633921898465292122, -0.000000000000000000 ) ) ;
#11532 = DIRECTION ( 'NONE',  ( 0.000000000000000000, 0.000000000000000000, 1.000000000000000000 ) ) ;
#11533 = VECTOR ( 'NONE', #2910, 1000.000000000000114 ) ;
#11534 = EDGE_LOOP ( 'NONE', ( #22875, #27732 ) ) ;
#11535 = CARTESIAN_POINT ( 'NONE',  ( 23.24667624907481667, -14.69156368041588934, 5.145673169868544505 ) ) ;
#11536 = CARTESIAN_POINT ( 'NONE',  ( -1.861312627816293253, -17.80543024186813383, -28.79488058872718881 ) ) ;
#11537 = VERTEX_POINT ( 'NONE', #11070 ) ;
#11538 = ORIENTED_EDGE ( 'NONE', *, *, #8753, .T. ) ;
#11539 = VERTEX_POINT ( 'NONE', #30264 ) ;
#11540 =( LENGTH_UNIT ( ) NAMED_UNIT ( * ) SI_UNIT ( .MILLI., .METRE. ) );
#11541 = ORIENTED_EDGE ( 'NONE', *, *, #26945, .T. ) ;
#11542 = CARTESIAN_POINT ( 'NONE',  ( 24.37821946547973084, -14.76389286113969490, 5.208432824000020389 ) ) ;
#11543 = B_SPLINE_CURVE_WITH_KNOTS ( 'NONE', 5,
 ( #17226, #12358, #29181, #575, #26381, #24018, #10156, #19600, #2605, #29337, #21495, #5280 ),
 .UNSPECIFIED., .F., .F.,
 ( 6, 3, 3, 6 ),
 ( 2.782752057460000206, 3.293393370880000059, 4.940089941970000176, 5.565010780559999759 ),
 .UNSPECIFIED. ) ;
#11544 = CARTESIAN_POINT ( 'NONE',  ( 8.903108651239925564, -22.82508830966962421, 140.0000000000000000 ) ) ;
#11545 = EDGE_CURVE ( 'NONE', #28246, #8534, #27737, .T. ) ;
#11546 = CARTESIAN_POINT ( 'NONE',  ( 4.434603606047636148, 2.142645224023219441, -66.10315453652499684 ) ) ;
#11547 = SURFACE_STYLE_FILL_AREA ( #23519 ) ;
#11548 = EDGE_CURVE ( 'NONE', #13159, #5171, #11082, .T. ) ;
#11549 = CARTESIAN_POINT ( 'NONE',  ( -18.94275355761817181, 21.23709850871491511, 0.5017677510000262409 ) ) ;
#11550 = CYLINDRICAL_SURFACE ( 'NONE', #20064, 1.100000000000002309 ) ;
#11551 = DIRECTION ( 'NONE',  ( 0.000000000000000000, -1.000000000000000000, 0.000000000000000000 ) ) ;
#11552 = ORIENTED_EDGE ( 'NONE', *, *, #2143, .F. ) ;
#11553 = CARTESIAN_POINT ( 'NONE',  ( -18.66939278141083136, 19.99991229567540074, -0.6052796912250372197 ) ) ;
#11554 = ADVANCED_FACE ( 'NONE', ( #2213 ), #8952, .T. ) ;
#11555 = VECTOR ( 'NONE', #16299, 1000.000000000000114 ) ;
#11556 = CARTESIAN_POINT ( 'NONE',  ( 1.387648159808060999, -4.113210426322157609, -15.26414732020000464 ) ) ;
#11557 = CARTESIAN_POINT ( 'NONE',  ( 26.62825631580874131, -3.503650093567661106, -0.000000000000000000 ) ) ;
#11558 = LINE ( 'NONE', #25727, #16523 ) ;
#11559 = ORIENTED_EDGE ( 'NONE', *, *, #26804, .T. ) ;
#11560 = CARTESIAN_POINT ( 'NONE',  ( 26.57440914490000239, -3.469982507400000582, -1.399999999999998579 ) ) ;
#11561 = DIRECTION ( 'NONE',  ( -1.000000000000000000, 5.687697999151106851E-16, -6.771501495036750356E-12 ) ) ;
#11562 = CARTESIAN_POINT ( 'NONE',  ( -25.12323886820000141, 13.67941525610000042, 222.0000000000000000 ) ) ;
#11563 = CARTESIAN_POINT ( 'NONE',  ( 0.8057459563030000549, -27.78864806999999715, 225.7596297540000023 ) ) ;
#11564 = FACE_BOUND ( 'NONE', #5099, .T. ) ;
#11565 = DIRECTION ( 'NONE',  ( 0.000000000000000000, 0.000000000000000000, 1.000000000000000000 ) ) ;
#11566 = ADVANCED_FACE ( 'NONE', ( #23929 ), #12971, .T. ) ;
#11567 = CARTESIAN_POINT ( 'NONE',  ( 9.999999999959999997, -25.00000000000000000, -26.16393202319999745 ) ) ;
#11568 = FACE_OUTER_BOUND ( 'NONE', #9987, .T. ) ;
#11569 = ORIENTED_EDGE ( 'NONE', *, *, #947, .F. ) ;
#11570 = DIRECTION ( 'NONE',  ( 0.000000000000000000, 0.000000000000000000, -1.000000000000000000 ) ) ;
#11571 = LINE ( 'NONE', #9516, #22669 ) ;
#11572 = CARTESIAN_POINT ( 'NONE',  ( 2.738791508839905742, -3.809105199416136234, -68.10000000002500542 ) ) ;
#11573 = ADVANCED_FACE ( 'NONE', ( #24859 ), #4939, .T. ) ;
#11574 = CARTESIAN_POINT ( 'NONE',  ( 3.015246714024014452, 1.304698913893802104, -68.40345797962162067 ) ) ;
#11575 = CARTESIAN_POINT ( 'NONE',  ( 9.599333684284403034, -15.14023671706337915, -74.38892505371892128 ) ) ;
#11576 = SURFACE_STYLE_FILL_AREA ( #1987 ) ;
#11577 = VERTEX_POINT ( 'NONE', #5954 ) ;
#11578 = CARTESIAN_POINT ( 'NONE',  ( 27.54391550599999761, -3.373045393770000084E-15, 37.04374668510000390 ) ) ;
#11579 = CARTESIAN_POINT ( 'NONE',  ( -3.807105672873282831, -5.136256491778199873, -65.61409070562500290 ) ) ;
#11580 = VERTEX_POINT ( 'NONE', #3287 ) ;
#11581 = CARTESIAN_POINT ( 'NONE',  ( 24.39448487261446274, -13.33383073951642928, 3.899998581000052145 ) ) ;
#11582 = ADVANCED_FACE ( 'NONE', ( #25160 ), #3592, .F. ) ;
#11583 = CARTESIAN_POINT ( 'NONE',  ( -19.49313842129999941, 19.58644462790000063, 229.5590894759999969 ) ) ;
#11584 = VERTEX_POINT ( 'NONE', #6277 ) ;
#11585 = CARTESIAN_POINT ( 'NONE',  ( -1.094484693600000114, 5.799375430310000468, 226.6412452697800006 ) ) ;
#11586 = CARTESIAN_POINT ( 'NONE',  ( -27.06563796000000366, 3.314475221609999872E-15, 188.0597313979999967 ) ) ;
#11587 = CARTESIAN_POINT ( 'NONE',  ( -8.699999999661049088, -18.40166527955781817, -36.11775795388252419 ) ) ;
#11588 = PRODUCT_DEFINITION_CONTEXT ( 'detailed design', #544, 'design' ) ;
#11589 = B_SPLINE_CURVE_WITH_KNOTS ( 'NONE', 3,
 ( #6847, #6691, #23398, #4181, #1829, #28412 ),
 .UNSPECIFIED., .F., .F.,
 ( 4, 2, 4 ),
 ( 0.000000000000000000, 0.5000000000000000000, 1.000000000000000000 ),
 .UNSPECIFIED. ) ;
#11590 = CARTESIAN_POINT ( 'NONE',  ( -0.4846640835643744039, -27.79604706135699033, 4.493528488000025689 ) ) ;
#11591 = CARTESIAN_POINT ( 'NONE',  ( -3.063879268240000009, -1.673804873600000187, 230.8412452700000017 ) ) ;
#11592 = DIRECTION ( 'NONE',  ( 0.000000000000000000, 0.000000000000000000, 1.000000000000000000 ) ) ;
#11593 = ORIENTED_EDGE ( 'NONE', *, *, #19066, .F. ) ;
#11594 = CARTESIAN_POINT ( 'NONE',  ( 20.30396079662882158, 20.00000000004802203, 3.000000000000002665 ) ) ;
#11595 = CARTESIAN_POINT ( 'NONE',  ( 0.1474953887282549891, -26.80000000000001492, 226.0999999999999943 ) ) ;
#11596 = FACE_OUTER_BOUND ( 'NONE', #4825, .T. ) ;
#11597 = DIRECTION ( 'NONE',  ( -1.000000000000000000, 0.000000000000000000, 0.000000000000000000 ) ) ;
#11598 = CARTESIAN_POINT ( 'NONE',  ( 0.2766207017872922003, 12.09920997781417107, 232.0000000000052864 ) ) ;
#11599 = CARTESIAN_POINT ( 'NONE',  ( 4.792542393929999811, -11.13937006400000129, 230.6412452697800006 ) ) ;
#11600 = EDGE_CURVE ( 'NONE', #6881, #24307, #15704, .T. ) ;
#11601 = CARTESIAN_POINT ( 'NONE',  ( 12.27487041388367395, 21.70000000000035811, -55.79574881355755878 ) ) ;
#11602 = CARTESIAN_POINT ( 'NONE',  ( 0.5234957687185606279, 1.947945353336631324, 227.6412452700308791 ) ) ;
#11603 = CARTESIAN_POINT ( 'NONE',  ( 2.259239758627727745, -4.069767828330737913, -54.83172062782499268 ) ) ;
#11604 = EDGE_CURVE ( 'NONE', #2594, #25714, #17091, .T. ) ;
#11605 = AXIS2_PLACEMENT_3D ( 'NONE', #28738, #23728, #24180 ) ;
#11606 = CARTESIAN_POINT ( 'NONE',  ( -20.30396346370000060, 20.00000000000000000, 228.1999999999999886 ) ) ;
#11607 = DIRECTION ( 'NONE',  ( 0.2815395311429191305, 0.9595496299847262600, 0.000000000000000000 ) ) ;
#11608 = CARTESIAN_POINT ( 'NONE',  ( 2.721155027367574863, -2.286694320792284962, 230.8124538892466262 ) ) ;
#11609 = CARTESIAN_POINT ( 'NONE',  ( -0.9950318224731415917, -27.48257863589062566, 224.5094458579580987 ) ) ;
#11610 = CARTESIAN_POINT ( 'NONE',  ( -24.02415253779999915, -13.98938335050000070, 223.9040321109999923 ) ) ;
#11611 = B_SPLINE_CURVE_WITH_KNOTS ( 'NONE', 3,
 ( #23047, #23521, #21146, #16419 ),
 .UNSPECIFIED., .F., .F.,
 ( 4, 4 ),
 ( 0.000000000000000000, 1.000000000000000000 ),
 .UNSPECIFIED. ) ;
#11612 = CARTESIAN_POINT ( 'NONE',  ( -1.157762119782732135, -5.359362766143966006, -56.73033560642500817 ) ) ;
#11613 = ORIENTED_EDGE ( 'NONE', *, *, #8085, .F. ) ;
#11614 = ITEM_DEFINED_TRANSFORMATION ( 'NONE', 'NONE', #8296,  #17722 ) ;
#11615 = ORIENTED_EDGE ( 'NONE', *, *, #11993, .T. ) ;
#11616 = CARTESIAN_POINT ( 'NONE',  ( -17.49199711315135986, -29.39779533043000015, -32.78913491261000246 ) ) ;
#11617 = ORIENTED_EDGE ( 'NONE', *, *, #27014, .T. ) ;
#11618 = DIRECTION ( 'NONE',  ( -1.821459649777283484E-13, 0.9753733754015535551, -0.2205601472564346632 ) ) ;
#11619 = CARTESIAN_POINT ( 'NONE',  ( 6.438687372225744276, -8.560122214837054599, -36.64192442626541890 ) ) ;
#11620 = FACE_OUTER_BOUND ( 'NONE', #27534, .T. ) ;
#11621 = TOROIDAL_SURFACE ( 'NONE', #2593, 12.03781779390000040, 5.000000000000000000 ) ;
#11622 = CARTESIAN_POINT ( 'NONE',  ( -3.862368227480000193, -11.41372166100000207, 231.9999991140000191 ) ) ;
#11623 = CARTESIAN_POINT ( 'NONE',  ( -24.32472894358752313, 13.45989150749028873, 6.099998581000020792 ) ) ;
#11624 = DIRECTION ( 'NONE',  ( 0.000000000000000000, -0.5000000000001900702, -0.8660254037843290176 ) ) ;
#11625 = CARTESIAN_POINT ( 'NONE',  ( 2.032938288397245330, -5.563452252945958243, -5.260585232200003070 ) ) ;
#11626 = CARTESIAN_POINT ( 'NONE',  ( -27.56257419730000180, 3.552713678799999608E-15, 230.5592437530000041 ) ) ;
#11627 = B_SPLINE_CURVE_WITH_KNOTS ( 'NONE', 3,
 ( #2931, #4983, #24032, #2476, #12066, #14742, #9386, #21825, #19306, #24338, #7036, #14594, #21362, #28900, #7497, #2782, #26234, #11908 ),
 .UNSPECIFIED., .F., .F.,
 ( 4, 2, 2, 2, 2, 2, 2, 2, 4 ),
 ( 0.000000000000000000, 0.1250000000000000555, 0.2500000000000001110, 0.3750000000000001665, 0.5000000000000001110, 0.6250000000000001110, 0.7500000000000001110, 0.8750000000000000000, 1.000000000000000000 ),
 .UNSPECIFIED. ) ;
#11628 = ORIENTED_EDGE ( 'NONE', *, *, #1514, .F. ) ;
#11629 = CARTESIAN_POINT ( 'NONE',  ( 10.00000000000000000, 21.70000000000000284, -62.10000000019999788 ) ) ;
#11630 = CARTESIAN_POINT ( 'NONE',  ( 3.256742448429973624, 4.730705660258329281, -17.21259163649999735 ) ) ;
#11631 = CARTESIAN_POINT ( 'NONE',  ( -0.9837773765372604950, -27.78287111172183899, 225.4958527047016617 ) ) ;
#11632 = DIRECTION ( 'NONE',  ( 1.666951178525963134E-12, -0.4082287037029531107, -0.9128796883888953273 ) ) ;
#11633 = EDGE_CURVE ( 'NONE', #4159, #15947, #30040, .T. ) ;
#11634 = CARTESIAN_POINT ( 'NONE',  ( 28.22605159097494010, -9.791255285991017132, -0.2432540810000105580 ) ) ;
#11635 = CARTESIAN_POINT ( 'NONE',  ( -24.39524108170000360, -13.33235248870000156, 224.0985996330000205 ) ) ;
#11636 = CARTESIAN_POINT ( 'NONE',  ( -27.79539923781770128, -0.5057481688779102980, 8.000000000000007105 ) ) ;
#11637 = CARTESIAN_POINT ( 'NONE',  ( -19.56375666326936269, 19.56885676738829005, 0.5004811919999962999 ) ) ;
#11638 = CARTESIAN_POINT ( 'NONE',  ( 28.03861306157277866, 0.5101735396241825482, -0.2432540810000105580 ) ) ;
#11639 = EDGE_CURVE ( 'NONE', #24853, #6068, #18196, .T. ) ;
#11640 = CARTESIAN_POINT ( 'NONE',  ( -3.509503079120555036, -0.3786683407750112695, 226.6412452697750268 ) ) ;
#11641 = DIRECTION ( 'NONE',  ( -1.000000000000000000, 5.687697937797165957E-16, -6.771501495045624776E-12 ) ) ;
#11642 = ADVANCED_FACE ( 'NONE', ( #17746 ), #29033, .F. ) ;
#11643 = CARTESIAN_POINT ( 'NONE',  ( 27.92857142909999979, -3.420150602509999660E-15, 187.9396849849999853 ) ) ;
#11644 = AXIS2_PLACEMENT_3D ( 'NONE', #3893, #25134, #4050 ) ;
#11645 = EDGE_LOOP ( 'NONE', ( #3590, #23663, #9091, #2232 ) ) ;
#11646 = CARTESIAN_POINT ( 'NONE',  ( 8.700000000246273402, -23.99025505878464060, -28.09032254495748049 ) ) ;
#11647 = CARTESIAN_POINT ( 'NONE',  ( -12.29999999969999891, -29.39114981890000067, -32.77697038446999755 ) ) ;
#11648 = CARTESIAN_POINT ( 'NONE',  ( -0.3681746154257226067, -5.199302247677223932, -0.7000416189860052540 ) ) ;
#11649 = CIRCLE ( 'NONE', #5546, 6.000000000000001776 ) ;
#11650 = VERTEX_POINT ( 'NONE', #30031 ) ;
#11651 = ORIENTED_EDGE ( 'NONE', *, *, #26573, .T. ) ;
#11652 = VERTEX_POINT ( 'NONE', #6111 ) ;
#11653 = DIRECTION ( 'NONE',  ( 1.000000000000000000, 0.000000000000000000, 0.000000000000000000 ) ) ;
#11654 = EDGE_LOOP ( 'NONE', ( #5678, #22673 ) ) ;
#11655 = DIRECTION ( 'NONE',  ( -0.9316362575375356503, -0.3633921898465274913, 0.000000000000000000 ) ) ;
#11656 = VERTEX_POINT ( 'NONE', #29723 ) ;
#11657 = CARTESIAN_POINT ( 'NONE',  ( -24.69967241520000201, -14.21967358789999913, 226.1000014189999945 ) ) ;
#11658 = CARTESIAN_POINT ( 'NONE',  ( 23.87963657767028280, 15.55698410313905988, 4.493007569000006640 ) ) ;
#11659 = CARTESIAN_POINT ( 'NONE',  ( -23.81776757772072983, -15.65134804123479917, 4.999998581000003384 ) ) ;
#11660 = CARTESIAN_POINT ( 'NONE',  ( 1.960433969464639770, 3.445019499235556282, -35.70000000000000284 ) ) ;
#11661 = CARTESIAN_POINT ( 'NONE',  ( 19.55507467582014414, 20.00006801630439668, -0.2385979495973736264 ) ) ;
#11662 = CARTESIAN_POINT ( 'NONE',  ( 14.75563848642255849, -22.00000000000000000, -29.68302488264445671 ) ) ;
#11663 = DIRECTION ( 'NONE',  ( 0.7071067811780481493, 0.6644630243965948813, 0.2418447626510653869 ) ) ;
#11664 = CARTESIAN_POINT ( 'NONE',  ( -17.83931601680000156, 20.00000000000000000, 229.9999991770000065 ) ) ;
#11665 = ORIENTED_EDGE ( 'NONE', *, *, #26276, .F. ) ;
#11666 = ADVANCED_FACE ( 'NONE', ( #10681, #25479 ), #18218, .T. ) ;
#11667 = CIRCLE ( 'NONE', #3608, 27.50000000000000000 ) ;
#11668 = CARTESIAN_POINT ( 'NONE',  ( 1.604951280288046567, -4.392199147046019547, -6.760585232199999517 ) ) ;
#11669 = CARTESIAN_POINT ( 'NONE',  ( -5.367600138795724618, 3.713494282866228069, -25.46779765530001072 ) ) ;
#11670 = CARTESIAN_POINT ( 'NONE',  ( -9.999999999559999964, 21.35000000040000145, -60.10000000000000142 ) ) ;
#11671 = CARTESIAN_POINT ( 'NONE',  ( -3.886410967837877539, -2.904140848474241920, -94.91462932778338768 ) ) ;
#11672 = FACE_OUTER_BOUND ( 'NONE', #5412, .T. ) ;
#11673 = PLANE ( 'NONE',  #13114 ) ;
#11674 = CARTESIAN_POINT ( 'NONE',  ( -23.74375282219999761, -14.46070769699999836, 225.9014025209999943 ) ) ;
#11675 = DIRECTION ( 'NONE',  ( 0.000000000000000000, 0.9396926207858125046, 0.3420201433259318358 ) ) ;
#11676 = CARTESIAN_POINT ( 'NONE',  ( 1.413941964927726946, -28.46527362969718311, 5.680166690000016061 ) ) ;
#11677 = DIRECTION ( 'NONE',  ( 1.000000000000000000, 0.000000000000000000, 0.000000000000000000 ) ) ;
#11678 = VERTEX_POINT ( 'NONE', #17903 ) ;
#11679 = CARTESIAN_POINT ( 'NONE',  ( -1.078772944755383767, 5.890544393200768170, -59.77324387862499577 ) ) ;
#11680 = CARTESIAN_POINT ( 'NONE',  ( -21.78691859319999935, 17.45882806430000045, 229.7313258739999924 ) ) ;
#11681 = ORIENTED_EDGE ( 'NONE', *, *, #17819, .T. ) ;
#11682 = CARTESIAN_POINT ( 'NONE',  ( 8.700000000273695022, -16.20708930593283625, -33.02464488162291900 ) ) ;
#11683 = DIRECTION ( 'NONE',  ( 0.5532886644841251700, 0.8329895880221872551, -0.000000000000000000 ) ) ;
#11684 = VERTEX_POINT ( 'NONE', #27507 ) ;
#11685 = CARTESIAN_POINT ( 'NONE',  ( 25.22625794089999829, -13.26224522399999906, 225.0000014190000002 ) ) ;
#11686 = CARTESIAN_POINT ( 'NONE',  ( 24.36375418468539067, 14.78716628296302282, 3.904032100999987875 ) ) ;
#11688 = VERTEX_POINT ( 'NONE', #22959 ) ;
#11687 = AXIS2_PLACEMENT_3D ( 'NONE', #806, #22658, #8162 ) ;
#11689 = B_SPLINE_CURVE_WITH_KNOTS ( 'NONE', 3,
 ( #11333, #21090, #11640, #21240, #8803, #30837, #23143, #9268, #28004, #19028, #6601, #18874, #20768, #28471, #1584, #6908, #16510, #8963 ),
 .UNSPECIFIED., .F., .F.,
 ( 4, 2, 2, 2, 2, 2, 2, 2, 4 ),
 ( 0.000000000000000000, 0.1250000000000000555, 0.2500000000000001110, 0.3750000000000001665, 0.5000000000000001110, 0.6250000000000001110, 0.7500000000000001110, 0.8750000000000000000, 1.000000000000000000 ),
 .UNSPECIFIED. ) ;
#11690 = ORIENTED_EDGE ( 'NONE', *, *, #17902, .F. ) ;
#11691 = ORIENTED_EDGE ( 'NONE', *, *, #11633, .F. ) ;
#11692 = EDGE_LOOP ( 'NONE', ( #12228, #10932, #2171, #18501 ) ) ;
#11693 = CARTESIAN_POINT ( 'NONE',  ( 24.74993095452947856, -14.13250376044891965, 6.042507811999997536 ) ) ;
#11694 = CARTESIAN_POINT ( 'NONE',  ( 9.799999999982377474, -17.77478083483991966, -34.71627511718394032 ) ) ;
#11695 = ADVANCED_FACE ( 'NONE', ( #1407 ), #11001, .T. ) ;
#11696 = CARTESIAN_POINT ( 'NONE',  ( 0.3196029497759475535, 5.089975830446680227, -68.87875473022501183 ) ) ;
#11697 = EDGE_CURVE ( 'NONE', #11462, #1593, #11968, .T. ) ;
#11698 = CARTESIAN_POINT ( 'NONE',  ( 24.63023943419999995, -14.11569779149999881, 230.0000000000000000 ) ) ;
#11699 = CARTESIAN_POINT ( 'NONE',  ( 17.95841148951064525, -9.763538383420391042, -0.6999999989999727834 ) ) ;
#11700 = CARTESIAN_POINT ( 'NONE',  ( 24.05322775159999793, -15.76571806769999995, 222.0000000000000000 ) ) ;
#11701 = CARTESIAN_POINT ( 'NONE',  ( 3.580158647405435435, -3.257180914152149054, -0.6998395211047659936 ) ) ;
#11702 = ORIENTED_EDGE ( 'NONE', *, *, #10251, .F. ) ;
#11703 = EDGE_CURVE ( 'NONE', #4659, #21418, #6933, .T. ) ;
#11704 = CARTESIAN_POINT ( 'NONE',  ( -18.63748837690081572, 19.99991059812205307, -0.6126749037462432268 ) ) ;
#11705 = CARTESIAN_POINT ( 'NONE',  ( 5.093259405240584847, 0.3640143666580218373, -13.70704535869999852 ) ) ;
#11706 = FACE_OUTER_BOUND ( 'NONE', #16673, .T. ) ;
#11707 = CARTESIAN_POINT ( 'NONE',  ( 2.900346228477644228, -11.98357204604639392, 232.6627637253559442 ) ) ;
#11708 = VECTOR ( 'NONE', #29158, 1000.000000000000000 ) ;
#11709 = VERTEX_POINT ( 'NONE', #30356 ) ;
#11710 = CARTESIAN_POINT ( 'NONE',  ( 26.79009884939612363, -1.309321278689688173, -1.399999999999998801 ) ) ;
#11711 = CARTESIAN_POINT ( 'NONE',  ( 1.379247882464924579, -27.76613141686495823, 4.319830470999985295 ) ) ;
#11712 = CARTESIAN_POINT ( 'NONE',  ( 18.23234009272960776, 11.30637938200976045, -0.6999999999999785283 ) ) ;
#11713 = CARTESIAN_POINT ( 'NONE',  ( -23.23277431133845994, -15.26692929363520257, 4.999998581000003384 ) ) ;
#11714 = LINE ( 'NONE', #1974, #20231 ) ;
#11715 = CARTESIAN_POINT ( 'NONE',  ( -10.00000000010863133, -25.15635984007449721, -30.79900052719556669 ) ) ;
#11716 = CARTESIAN_POINT ( 'NONE',  ( 8.754113545170000556E-10, -26.80000000020000073, 230.0000000000000000 ) ) ;
#11717 = VERTEX_POINT ( 'NONE', #23595 ) ;
#11718 = EDGE_CURVE ( 'NONE', #7680, #90, #13669, .T. ) ;
#11719 = PLANE ( 'NONE',  #21836 ) ;
#11720 = CARTESIAN_POINT ( 'NONE',  ( -7.999999999669004325, -18.23122067930106027, -34.51216076568240965 ) ) ;
#11721 = CARTESIAN_POINT ( 'NONE',  ( -10.69999999999999929, -29.06671945329999929, -26.22544931050000017 ) ) ;
#11722 = CARTESIAN_POINT ( 'NONE',  ( -4.817157408371211424, 0.2680464973864214451, -68.10000000002500542 ) ) ;
#11723 = VECTOR ( 'NONE', #8722, 1000.000000000000000 ) ;
#11724 = DIRECTION ( 'NONE',  ( 1.000000000000000000, 0.000000000000000000, 0.000000000000000000 ) ) ;
#11725 = CARTESIAN_POINT ( 'NONE',  ( 16.40303402075260308, 10.20816091466531716, -0.6999999999999784173 ) ) ;
#11726 = ORIENTED_EDGE ( 'NONE', *, *, #21391, .F. ) ;
#11727 = CARTESIAN_POINT ( 'NONE',  ( -11.98357192835155338, -2.900346203988739102, 232.6627637660202481 ) ) ;
#11728 = VECTOR ( 'NONE', #24983, 1000.000000000000114 ) ;
#11729 = CARTESIAN_POINT ( 'NONE',  ( 1.495522319887057749, -27.76012052182125345, 4.493506933999996455 ) ) ;
#11730 = ORIENTED_EDGE ( 'NONE', *, *, #30355, .F. ) ;
#11731 = CARTESIAN_POINT ( 'NONE',  ( -10.35667741062608371, -26.55163333981974816, 90.00000000000000000 ) ) ;
#11732 = CARTESIAN_POINT ( 'NONE',  ( -27.66290831536099759, -7.787312998881454895, 1.000000000000000888 ) ) ;
#11733 = ORIENTED_EDGE ( 'NONE', *, *, #5945, .T. ) ;
#11734 = CARTESIAN_POINT ( 'NONE',  ( -2.862882362289999705, 5.240471012849999610, 226.6412452697800006 ) ) ;
#11735 = CARTESIAN_POINT ( 'NONE',  ( 17.73945528632581059, -9.950349630033622716, -0.6999999999999784173 ) ) ;
#11736 = CARTESIAN_POINT ( 'NONE',  ( -12.77820031409999935, 21.69999999929999390, -56.09999999999999432 ) ) ;
#11737 = ADVANCED_FACE ( 'NONE', ( #4382 ), #20915, .T. ) ;
#11738 = PLANE ( 'NONE',  #7771 ) ;
#11739 = CARTESIAN_POINT ( 'NONE',  ( -12.59933368422367472, 25.69710080817275255, -59.52534974783780086 ) ) ;
#11740 = CARTESIAN_POINT ( 'NONE',  ( -10.00000000020000002, -29.15099216359999801, -26.30554312050000121 ) ) ;
#11741 = ORIENTED_EDGE ( 'NONE', *, *, #7883, .F. ) ;
#11742 = DIRECTION ( 'NONE',  ( 1.000000000000000000, -9.219999999999999084E-13, 4.710999999999999616E-12 ) ) ;
#11743 = CARTESIAN_POINT ( 'NONE',  ( 0.2892544100089353698, -26.79878419707955572, 226.0714905181768017 ) ) ;
#11744 = AXIS2_PLACEMENT_3D ( 'NONE', #16821, #14630, #12256 ) ;
#11745 = CYLINDRICAL_SURFACE ( 'NONE', #15293, 1.000000000000000666 ) ;
#11746 = PLANE ( 'NONE',  #21318 ) ;
#11747 = CARTESIAN_POINT ( 'NONE',  ( -12.39150945512032109, -30.55429417067527709, -32.12142999588005665 ) ) ;
#11748 = AXIS2_PLACEMENT_3D ( 'NONE', #13421, #10916, #13587 ) ;
#11749 = CARTESIAN_POINT ( 'NONE',  ( -0.03443693864400000637, -27.80022362959999782, 226.1000014189999945 ) ) ;
#11750 = CARTESIAN_POINT ( 'NONE',  ( 24.07552309629999954, -13.90001137839999856, 223.9000014189999774 ) ) ;
#11751 = EDGE_CURVE ( 'NONE', #6489, #8030, #17963, .T. ) ;
#11752 = CARTESIAN_POINT ( 'NONE',  ( -11.08346179031915568, -28.41490585489482967, 36.39444872449999480 ) ) ;
#11753 = CARTESIAN_POINT ( 'NONE',  ( 1.229093439949827005, -1.599333684796362176, 227.6412452702929841 ) ) ;
#11754 = CARTESIAN_POINT ( 'NONE',  ( -4.803332065605933288, -2.627392435372716495, -52.54982952342499658 ) ) ;
#11755 = EDGE_CURVE ( 'NONE', #12454, #6451, #10465, .T. ) ;
#11756 = EDGE_CURVE ( 'NONE', #20656, #4699, #28547, .T. ) ;
#11757 = CARTESIAN_POINT ( 'NONE',  ( -20.30396346370000060, 20.00000000000000000, 227.0000000000000000 ) ) ;
#11758 = CARTESIAN_POINT ( 'NONE',  ( -27.77512470430000135, -2.247280056659999669E-11, 229.2930777930000090 ) ) ;
#11759 = CARTESIAN_POINT ( 'NONE',  ( 7.620434517626458515, -115.2052681231116509, 21.76600287036780301 ) ) ;
#11760 = ORIENTED_EDGE ( 'NONE', *, *, #3742, .F. ) ;
#11761 = CARTESIAN_POINT ( 'NONE',  ( 0.8697582157835563876, -2.615810859153466783, -36.20335296958887028 ) ) ;
#11762 = EDGE_CURVE ( 'NONE', #16094, #20043, #28294, .T. ) ;
#11763 = ORIENTED_EDGE ( 'NONE', *, *, #27821, .T. ) ;
#11764 = CARTESIAN_POINT ( 'NONE',  ( -24.11911872370000154, -15.18353100999999938, 224.6893563800000209 ) ) ;
#11765 = VECTOR ( 'NONE', #10481, 1000.000000000000114 ) ;
#11766 = CARTESIAN_POINT ( 'NONE',  ( -1.650988191866306742, 3.989749455477753504, -57.14652090042499566 ) ) ;
#11767 = ORIENTED_EDGE ( 'NONE', *, *, #23494, .F. ) ;
#11768 = CONTEXT_DEPENDENT_SHAPE_REPRESENTATION ( #6766, #12931 ) ;
#11769 = VECTOR ( 'NONE', #22008, 1000.000000000000000 ) ;
#11770 = ORIENTED_EDGE ( 'NONE', *, *, #10636, .T. ) ;
#11772 = EDGE_CURVE ( 'NONE', #26210, #12302, #8435, .T. ) ;
#11771 = CARTESIAN_POINT ( 'NONE',  ( -10.00000000001596767, -17.89976820896369247, -35.09161223051660983 ) ) ;
#11773 = VERTEX_POINT ( 'NONE', #1870 ) ;
#11774 =( LENGTH_UNIT ( ) NAMED_UNIT ( * ) SI_UNIT ( .MILLI., .METRE. ) );
#11775 = CARTESIAN_POINT ( 'NONE',  ( -8.699999999649387306, -11.00382829991729849, -37.83919293449501708 ) ) ;
#11776 = CARTESIAN_POINT ( 'NONE',  ( -25.38146355688813216, 12.59839640969179975, 6.600000000000022737 ) ) ;
#11777 = DIRECTION ( 'NONE',  ( -1.000000000000000000, 5.665498452320000818E-16, 0.000000000000000000 ) ) ;
#11778 = CARTESIAN_POINT ( 'NONE',  ( -26.79556473285982321, -0.4875557887250224209, 0.000000000000000000 ) ) ;
#11779 = APPLICATION_CONTEXT ( 'automotive_design' ) ;
#11780 = CARTESIAN_POINT ( 'NONE',  ( -19.80535357377644701, 19.50875577052588739, 1.000000000000000888 ) ) ;
#11781 = CARTESIAN_POINT ( 'NONE',  ( -3.993179150428259661, -2.644027878211168581, -5.952429326000007848 ) ) ;
#11782 = CARTESIAN_POINT ( 'NONE',  ( 21.06251243579999866, -21.19733559970000414, 229.7625741969999922 ) ) ;
#11783 = ORIENTED_EDGE ( 'NONE', *, *, #28437, .T. ) ;
#11784 = CARTESIAN_POINT ( 'NONE',  ( -18.95046173579999760, -18.95046173579999760, 43.21714158840000408 ) ) ;
#11785 = EDGE_CURVE ( 'NONE', #4633, #25869, #26134, .T. ) ;
#11786 = CARTESIAN_POINT ( 'NONE',  ( 5.864965375735811115, 0.4191680585659274261, -15.64454535870001095 ) ) ;
#11787 = CARTESIAN_POINT ( 'NONE',  ( -1.070949874232112187, -27.77969728621822298, 225.2892653499953326 ) ) ;
#11788 = DIRECTION ( 'NONE',  ( 0.000000000000000000, 0.000000000000000000, -1.000000000000000000 ) ) ;
#11789 = VECTOR ( 'NONE', #156, 1000.000000000000000 ) ;
#11790 = DIRECTION ( 'NONE',  ( 0.000000000000000000, 0.3420201433259318913, -0.9396926207858126157 ) ) ;
#11791 = CIRCLE ( 'NONE', #10800, 17.61822726820000184 ) ;
#11792 = CARTESIAN_POINT ( 'NONE',  ( -7.999999999638116144, -22.83323352248630655, -39.84673050082100332 ) ) ;
#11793 = CARTESIAN_POINT ( 'NONE',  ( -3.948109860491266776, 2.321589337205137937, -44.84354844312500177 ) ) ;
#11794 = DIRECTION ( 'NONE',  ( 1.000000000000000000, 0.000000000000000000, 0.000000000000000000 ) ) ;
#11795 = CARTESIAN_POINT ( 'NONE',  ( -23.73992238019999945, -12.43607998449999918, 5.000000000000000000 ) ) ;
#11796 = CARTESIAN_POINT ( 'NONE',  ( -24.98081131316241255, -13.71897606304888662, 5.104178996000019453 ) ) ;
#11797 = DIRECTION ( 'NONE',  ( 0.000000000000000000, 0.7071067811870488384, 0.7071067811860461960 ) ) ;
#11798 = ORIENTED_EDGE ( 'NONE', *, *, #20055, .F. ) ;
#11799 = CARTESIAN_POINT ( 'NONE',  ( -10.49049139480000115, 19.99999999999999645, -1.182260226200000597 ) ) ;
#11800 = CARTESIAN_POINT ( 'NONE',  ( 17.16657240420000008, 10.97998838177520931, 0.05106179917585291356 ) ) ;
#11801 = AXIS2_PLACEMENT_3D ( 'NONE', #16611, #25609, #4353 ) ;
#11802 = CYLINDRICAL_SURFACE ( 'NONE', #27260, 1.099999999999999201 ) ;
#11803 = COLOUR_RGB ( '', 0.66274510, 0.83137255, 0.94901961) ;
#11804 = ORIENTED_EDGE ( 'NONE', *, *, #29973, .T. ) ;
#11805 = CARTESIAN_POINT ( 'NONE',  ( -3.552713678799999608E-15, 0.000000000000000000, 193.2171415880000040 ) ) ;
#11806 = VERTEX_POINT ( 'NONE', #6737 ) ;
#11807 = VERTEX_POINT ( 'NONE', #9246 ) ;
#11808 = DIRECTION ( 'NONE',  ( 0.000000000000000000, 0.000000000000000000, 1.000000000000000000 ) ) ;
#11809 = ORIENTED_EDGE ( 'NONE', *, *, #8464, .T. ) ;
#11810 = CARTESIAN_POINT ( 'NONE',  ( -17.49227996845844402, -9.885041018070451102, 0.000000000000000000 ) ) ;
#11811 = ADVANCED_FACE ( 'NONE', ( #13829 ), #2031, .F. ) ;
#11812 = ORIENTED_EDGE ( 'NONE', *, *, #18978, .T. ) ;
#11814 = FACE_OUTER_BOUND ( 'NONE', #23664, .T. ) ;
#11813 = CIRCLE ( 'NONE', #29390, 26.80000000069999899 ) ;
#11815 = FACE_OUTER_BOUND ( 'NONE', #27696, .T. ) ;
#11816 = CARTESIAN_POINT ( 'NONE',  ( 0.8664230844016814759, 4.728695873782988279, -35.70000000000000995 ) ) ;
#11817 = EDGE_CURVE ( 'NONE', #9298, #7204, #11155, .T. ) ;
#11818 = B_SPLINE_CURVE_WITH_KNOTS ( 'NONE', 3,
 ( #3070, #26683, #17541, #10164, #12668, #22593, #3374, #5123 ),
 .UNSPECIFIED., .F., .F.,
 ( 4, 2, 2, 4 ),
 ( 0.000000000000000000, 0.2500000000000015543, 0.5000000000000031086, 1.000000000000000000 ),
 .UNSPECIFIED. ) ;
#11819 = B_SPLINE_CURVE_WITH_KNOTS ( 'NONE', 5,
 ( #22027, #14326, #320, #628, #158, #5168, #478, #2363, #19188, #11947, #26272, #28940 ),
 .UNSPECIFIED., .F., .F.,
 ( 6, 3, 3, 6 ),
 ( 0.000000000000000000, 1.357884646170000043, 2.715789077110000171, 3.784579750909999873 ),
 .UNSPECIFIED. ) ;
#11820 = EDGE_CURVE ( 'NONE', #13699, #29409, #13972, .T. ) ;
#11821 = DIRECTION ( 'NONE',  ( 0.9316362575375356503, 0.3633921898465274913, 0.000000000000000000 ) ) ;
#11822 = EDGE_CURVE ( 'NONE', #8842, #17525, #12966, .T. ) ;
#11823 = CARTESIAN_POINT ( 'NONE',  ( -8.903108651239966420, -22.82508830966961000, 40.00000000000000000 ) ) ;
#11824 = CARTESIAN_POINT ( 'NONE',  ( 10.69999999999999929, 19.99999999999999645, -42.39999999999999858 ) ) ;
#11825 = CARTESIAN_POINT ( 'NONE',  ( 17.95841148951064525, -9.763538383420391042, 0.000000000000000000 ) ) ;
#11826 = ORIENTED_EDGE ( 'NONE', *, *, #30137, .T. ) ;
#11827 = CARTESIAN_POINT ( 'NONE',  ( 3.530284718056032833, 5.524446756132658898, -5.800967428500003464 ) ) ;
#11828 = CARTESIAN_POINT ( 'NONE',  ( -3.357682761866084498, 3.860481585313637609, -27.64978588869999854 ) ) ;
#11829 = FACE_OUTER_BOUND ( 'NONE', #21842, .T. ) ;
#11830 = AXIS2_PLACEMENT_3D ( 'NONE', #18889, #28484, #6925 ) ;
#11831 = CARTESIAN_POINT ( 'NONE',  ( -3.374110856211531395, -1.022585090133552033, -90.77455165165939377 ) ) ;
#11832 = CARTESIAN_POINT ( 'NONE',  ( 24.34942395457898101, 13.41447635819141126, 5.310538874999992665 ) ) ;
#11833 = FACE_OUTER_BOUND ( 'NONE', #30058, .T. ) ;
#11834 = CARTESIAN_POINT ( 'NONE',  ( 3.950106903291103588, 1.853988655799144958, -2.479170051700008148 ) ) ;
#11835 = CARTESIAN_POINT ( 'NONE',  ( -1.421085471519999843E-14, -1.065814103639999922E-14, 136.7828584120000244 ) ) ;
#11836 = CARTESIAN_POINT ( 'NONE',  ( 7.468697110890166080, -6.348049517532677655, -34.38301854759198761 ) ) ;
#11837 = CARTESIAN_POINT ( 'NONE',  ( -17.62526668104891314, 11.76353838341477953, -0.6999999999999784173 ) ) ;
#11838 = VERTEX_POINT ( 'NONE', #4690 ) ;
#11839 = CYLINDRICAL_SURFACE ( 'NONE', #25337, 4.175165894169885483 ) ;
#11840 = CARTESIAN_POINT ( 'NONE',  ( 8.700000000270996736, -18.23122067931645773, -34.51216076560373125 ) ) ;
#11841 = VERTEX_POINT ( 'NONE', #30515 ) ;
#11842 = CARTESIAN_POINT ( 'NONE',  ( -23.55406855550000245, 16.04544956020000157, 222.0000000000000000 ) ) ;
#11843 = LINE ( 'NONE', #6811, #2744 ) ;
#11844 = ORIENTED_EDGE ( 'NONE', *, *, #20932, .T. ) ;
#11845 = ORIENTED_EDGE ( 'NONE', *, *, #13199, .F. ) ;
#11846 = VERTEX_POINT ( 'NONE', #8943 ) ;
#11847 =( NAMED_UNIT ( * ) PLANE_ANGLE_UNIT ( ) SI_UNIT ( $, .RADIAN. ) );
#11848 = ORIENTED_EDGE ( 'NONE', *, *, #25739, .T. ) ;
#11849 = CARTESIAN_POINT ( 'NONE',  ( 27.06563796540000411, -3.314475222259999564E-15, 38.05973140639999741 ) ) ;
#11850 = PRODUCT_DEFINITION_FORMATION_WITH_SPECIFIED_SOURCE ( 'ANY', '', #10831, .NOT_KNOWN. ) ;
#11851 = CARTESIAN_POINT ( 'NONE',  ( -8.903108651239966420, -22.82508830966961000, 90.00000000000000000 ) ) ;
#11852 = CARTESIAN_POINT ( 'NONE',  ( -7.999999999669917372, -18.13635916017433658, -34.30003174772016905 ) ) ;
#11853 = ORIENTED_EDGE ( 'NONE', *, *, #3778, .T. ) ;
#11854 = FACE_OUTER_BOUND ( 'NONE', #3308, .T. ) ;
#11855 = CARTESIAN_POINT ( 'NONE',  ( 24.53921759442506101, -13.06412590950472818, 225.5623281039913763 ) ) ;
#11856 = EDGE_CURVE ( 'NONE', #20367, #1634, #21052, .T. ) ;
#11857 = CARTESIAN_POINT ( 'NONE',  ( 27.79999999999999716, 2.345590388590000174E-11, 222.0000000000000000 ) ) ;
#11858 = CARTESIAN_POINT ( 'NONE',  ( 1.015231355570000105, -28.48218680760000154, 225.5064715119999903 ) ) ;
#11859 = ORIENTED_EDGE ( 'NONE', *, *, #30210, .F. ) ;
#11860 = CARTESIAN_POINT ( 'NONE',  ( -22.86552662831838489, -13.97920826416505946, 225.8816713824261910 ) ) ;
#11861 = CARTESIAN_POINT ( 'NONE',  ( -5.295622588438499534, 1.541709225419852780, -15.30443125760000100 ) ) ;
#11862 = CARTESIAN_POINT ( 'NONE',  ( -3.389121577140000063, -11.55088360979999962, 230.6412452697800006 ) ) ;
#11863 = DIRECTION ( 'NONE',  ( -0.9880370573969196046, 0.1542166437529879086, 0.000000000000000000 ) ) ;
#11864 = ORIENTED_EDGE ( 'NONE', *, *, #1101, .T. ) ;
#11865 = CARTESIAN_POINT ( 'NONE',  ( 8.000000000869471606, -28.58317312643325536, -30.97832802804627406 ) ) ;
#11866 = CARTESIAN_POINT ( 'NONE',  ( 1.533144572060379796, -28.45911136072525238, 4.493506933999996455 ) ) ;
#11867 = CARTESIAN_POINT ( 'NONE',  ( 25.79280520781986041, 13.25682296313440389, 1.000000000000000888 ) ) ;
#11868 = CARTESIAN_POINT ( 'NONE',  ( -13.67718144140000014, 20.99999999999999645, -57.16242377749999548 ) ) ;
#11869 = CARTESIAN_POINT ( 'NONE',  ( 17.16657240420000008, 10.97998838177520931, 0.05106179917585291356 ) ) ;
#11870 = CARTESIAN_POINT ( 'NONE',  ( 9.999999999959999997, -24.90230200559999574, -26.25506237459999781 ) ) ;
#11871 = CARTESIAN_POINT ( 'NONE',  ( -9.738910687886987105, -24.96785170200594095, 93.21714158839999698 ) ) ;
#11872 = ORIENTED_EDGE ( 'NONE', *, *, #16040, .F. ) ;
#11873 = EDGE_CURVE ( 'NONE', #24923, #22531, #4449, .T. ) ;
#11874 = CARTESIAN_POINT ( 'NONE',  ( -10.69999999999999929, -24.00000000000000000, -28.40910480009999617 ) ) ;
#11875 = CARTESIAN_POINT ( 'NONE',  ( 0.000000000000000000, 0.000000000000000000, 115.0000000000000000 ) ) ;
#11876 = B_SPLINE_CURVE_WITH_KNOTS ( 'NONE', 5,
 ( #7219, #28765, #21393, #9257, #23918, #7373 ),
 .UNSPECIFIED., .F., .F.,
 ( 6, 6 ),
 ( -3.500000000000000000, 3.500000000000000000 ),
 .UNSPECIFIED. ) ;
#11877 = CYLINDRICAL_SURFACE ( 'NONE', #18839, 27.50000000000000000 ) ;
#11878 = CARTESIAN_POINT ( 'NONE',  ( -7.861312627709997614, 3.765626869335708449, -39.31578811167678111 ) ) ;
#11879 = ORIENTED_EDGE ( 'NONE', *, *, #26802, .T. ) ;
#11880 = EDGE_CURVE ( 'NONE', #29903, #9281, #18597, .T. ) ;
#11881 = CARTESIAN_POINT ( 'NONE',  ( -3.552713678799999608E-15, 0.000000000000000000, 93.21714158839999698 ) ) ;
#11882 = EDGE_LOOP ( 'NONE', ( #2536, #10715, #10871, #13134 ) ) ;
#11883 = CARTESIAN_POINT ( 'NONE',  ( 23.97364091749897952, 15.41162527761334289, 5.735001252146398443 ) ) ;
#11884 = CARTESIAN_POINT ( 'NONE',  ( 1.257215589593053906, -4.341675124665346885, -67.70367649352500905 ) ) ;
#11885 = ORIENTED_EDGE ( 'NONE', *, *, #12141, .T. ) ;
#11886 = CARTESIAN_POINT ( 'NONE',  ( 0.000000000000000000, 0.000000000000000000, 226.6412452697749984 ) ) ;
#11887 = CARTESIAN_POINT ( 'NONE',  ( -4.240613917342963113, -1.711409762446096439, -59.38491726642499202 ) ) ;
#11888 = VERTEX_POINT ( 'NONE', #14452 ) ;
#11889 = CARTESIAN_POINT ( 'NONE',  ( 0.000000000000000000, 0.000000000000000000, 40.00000000000000000 ) ) ;
#11890 = CARTESIAN_POINT ( 'NONE',  ( -23.69427943501400691, -14.54081806258934861, 3.920145809000019632 ) ) ;
#11891 = CARTESIAN_POINT ( 'NONE',  ( 24.66410523950000311, -14.28055064019999953, 223.9000014189999774 ) ) ;
#11892 = UNCERTAINTY_MEASURE_WITH_UNIT (LENGTH_MEASURE( 1.000000000000000082E-05 ), #10483, 'distance_accuracy_value', 'NONE');
#11893 = CARTESIAN_POINT ( 'NONE',  ( 3.072394438959999974, 1.678456730820000020, 230.8356432492296619 ) ) ;
#11894 = CARTESIAN_POINT ( 'NONE',  ( -10.69999999994264250, -27.47131626858717368, -16.98885458297168327 ) ) ;
#11895 = CARTESIAN_POINT ( 'NONE',  ( 10.06596365874881194, -25.80632433378973900, 40.00000000000000000 ) ) ;
#11896 = EDGE_CURVE ( 'NONE', #30472, #19387, #7816, .T. ) ;
#11897 = ORIENTED_EDGE ( 'NONE', *, *, #5282, .F. ) ;
#11898 = DIRECTION ( 'NONE',  ( 0.000000000000000000, 0.000000000000000000, 1.000000000000000000 ) ) ;
#11899 = DIRECTION ( 'NONE',  ( 5.962915006522622422E-16, 0.4383711467890810676, 0.8987940462991651502 ) ) ;
#11900 = CARTESIAN_POINT ( 'NONE',  ( 19.90436025690000221, 20.00000717710000231, 229.9507895630000007 ) ) ;
#11901 = CARTESIAN_POINT ( 'NONE',  ( 0.000000000000000000, 0.000000000000000000, 191.6604601750000256 ) ) ;
#11902 = DIRECTION ( 'NONE',  ( 0.000000000000000000, 0.9396926207858125046, 0.3420201433259318358 ) ) ;
#11903 = CARTESIAN_POINT ( 'NONE',  ( -1.063084826879999945, -27.77996807399999923, 225.3102023309999993 ) ) ;
#11904 = CARTESIAN_POINT ( 'NONE',  ( 24.14759035961400713, -13.77518824758847416, 223.9000014190000059 ) ) ;
#11905 = CARTESIAN_POINT ( 'NONE',  ( 10.14902473058288912, -26.01926976374856437, 137.9396849850000137 ) ) ;
#11906 = LINE ( 'NONE', #21511, #21671 ) ;
#11907 = AXIS2_PLACEMENT_3D ( 'NONE', #14879, #12044, #24621 ) ;
#11908 = CARTESIAN_POINT ( 'NONE',  ( 3.378474373710000034, 11.51459555979999827, 232.0000000000000000 ) ) ;
#11909 = CARTESIAN_POINT ( 'NONE',  ( 17.29283780512531621, -7.897520476889244634, -0.6999999999999784173 ) ) ;
#11910 = CARTESIAN_POINT ( 'NONE',  ( 24.66346747934004568, 14.28208995973567141, 6.002748562000004284 ) ) ;
#11911 = ORIENTED_EDGE ( 'NONE', *, *, #12913, .T. ) ;
#11912 = ADVANCED_FACE ( 'NONE', ( #14609 ), #5935, .T. ) ;
#11913 = DIRECTION ( 'NONE',  ( 0.3633921898465291567, 0.9316362575375349842, 0.000000000000000000 ) ) ;
#11914 = B_SPLINE_CURVE_WITH_KNOTS ( 'NONE', 3,
 ( #14718, #24159, #24309, #21651, #2600, #7473, #19282, #7325 ),
 .UNSPECIFIED., .F., .F.,
 ( 4, 2, 2, 4 ),
 ( 0.000000000000000000, 0.2499999999999998890, 0.4999999999999997780, 1.000000000000000000 ),
 .UNSPECIFIED. ) ;
#11915 = VERTEX_POINT ( 'NONE', #7658 ) ;
#11916 = CARTESIAN_POINT ( 'NONE',  ( 3.956700543085249322, -2.628121156294186633, -36.95875473020000612 ) ) ;
#11917 = CARTESIAN_POINT ( 'NONE',  ( 4.824840617521342523, -2.656518825645647119, -59.10843849682499496 ) ) ;
#11918 = EDGE_LOOP ( 'NONE', ( #2700, #15578, #17892, #2222 ) ) ;
#11919 = ORIENTED_EDGE ( 'NONE', *, *, #18840, .F. ) ;
#11920 = CARTESIAN_POINT ( 'NONE',  ( -7.999999999650268201, -15.05691661382650537, -37.86814300153927348 ) ) ;
#11921 = VERTEX_POINT ( 'NONE', #17108 ) ;
#11922 = ADVANCED_FACE ( 'NONE', ( #15065 ), #21999, .T. ) ;
#11923 = FACE_OUTER_BOUND ( 'NONE', #23120, .T. ) ;
#11924 = CARTESIAN_POINT ( 'NONE',  ( 9.195955003099999914, 19.99999999999999645, -43.38800044014699608 ) ) ;
#11925 = EDGE_CURVE ( 'NONE', #6489, #1522, #2493, .T. ) ;
#11926 = CIRCLE ( 'NONE', #30003, 12.03781779370000038 ) ;
#11927 = DIRECTION ( 'NONE',  ( 0.000000000000000000, 1.000000000000000000, 9.516197338740001367E-15 ) ) ;
#11928 = B_SPLINE_CURVE_WITH_KNOTS ( 'NONE', 5,
 ( #10591, #5551, #30095, #20184, #27267, #3822 ),
 .UNSPECIFIED., .F., .F.,
 ( 6, 6 ),
 ( 0.000000000000000000, 0.2292465731912854965 ),
 .UNSPECIFIED. ) ;
#11929 = CARTESIAN_POINT ( 'NONE',  ( 14.25032083441342934, -27.35421241409322946, 1.000000000000000888 ) ) ;
#11930 = DIRECTION ( 'NONE',  ( 0.000000000000000000, 0.000000000000000000, 1.000000000000000000 ) ) ;
#11931 = CARTESIAN_POINT ( 'NONE',  ( 0.2164205762250857590, 5.520452575866341860, -6.937690181099999798 ) ) ;
#11932 = CARTESIAN_POINT ( 'NONE',  ( -27.29823224869999976, -10.02941179569999974, 230.6577119970000069 ) ) ;
#11933 = ORIENTED_EDGE ( 'NONE', *, *, #19427, .T. ) ;
#11934 = DIRECTION ( 'NONE',  ( 0.000000000000000000, 0.000000000000000000, 1.000000000000000000 ) ) ;
#11935 = EDGE_CURVE ( 'NONE', #20235, #17095, #4728, .T. ) ;
#11936 = CARTESIAN_POINT ( 'NONE',  ( 3.931047123110473329, -1.876836795983962469, -20.88180150029999993 ) ) ;
#11937 = CARTESIAN_POINT ( 'NONE',  ( -0.1441937193057689637, -27.80022590917395675, 226.1000014190000229 ) ) ;
#11938 = CARTESIAN_POINT ( 'NONE',  ( 18.26639035964474900, 11.02001161816309072, -0.6999999999999784173 ) ) ;
#11939 = CARTESIAN_POINT ( 'NONE',  ( -12.09065967409999942, 0.9322763426430000777, 230.6412452697800006 ) ) ;
#11940 = CARTESIAN_POINT ( 'NONE',  ( -1.421085471519999843E-14, -1.065814103639999922E-14, 136.7828584120000244 ) ) ;
#11941 = CARTESIAN_POINT ( 'NONE',  ( 3.001777156698443250, -4.698362801289899693, -43.56966640442499283 ) ) ;
#11942 = DIRECTION ( 'NONE',  ( 1.000000000000000000, 0.000000000000000000, 0.000000000000000000 ) ) ;
#11943 = CARTESIAN_POINT ( 'NONE',  ( 27.79999999999999716, -2.355626804729999831E-11, 222.0000000000000000 ) ) ;
#11944 = DIRECTION ( 'NONE',  ( -6.208823127015005183E-10, -0.4383711467890810676, -0.8987940462991651502 ) ) ;
#11945 = ADVANCED_FACE ( 'NONE', ( #11923 ), #5101, .T. ) ;
#11946 = CIRCLE ( 'NONE', #2418, 26.80000000000000071 ) ;
#11947 = CARTESIAN_POINT ( 'NONE',  ( 8.999999999770000869, 21.68327394420000687, -44.79835558794399475 ) ) ;
#11948 = VERTEX_POINT ( 'NONE', #25124 ) ;
#11949 = AXIS2_PLACEMENT_3D ( 'NONE', #21646, #95, #24155 ) ;
#11950 = CARTESIAN_POINT ( 'NONE',  ( 6.000000000000000000, -17.74403716370463968, -75.33663091226621589 ) ) ;
#11951 = CARTESIAN_POINT ( 'NONE',  ( 16.37473331889771089, 11.76353838340827984, -0.6999999999999784173 ) ) ;
#11952 = CIRCLE ( 'NONE', #7441, 1.120011618224791450 ) ;
#11953 = CARTESIAN_POINT ( 'NONE',  ( -7.999999999654174410, -13.78556554857453698, -36.79016579852192592 ) ) ;
#11954 = ORIENTED_EDGE ( 'NONE', *, *, #29436, .F. ) ;
#11955 = CARTESIAN_POINT ( 'NONE',  ( 25.44662323365202639, -12.83524168329857318, 4.689351482000003735 ) ) ;
#11956 = CARTESIAN_POINT ( 'NONE',  ( 3.389692407805913632, 3.523397910813151679, -48.69426496242499525 ) ) ;
#11957 = ORIENTED_EDGE ( 'NONE', *, *, #19991, .F. ) ;
#11958 = EDGE_CURVE ( 'NONE', #18690, #29368, #24816, .T. ) ;
#11959 = ORIENTED_EDGE ( 'NONE', *, *, #6124, .T. ) ;
#11960 =( LENGTH_UNIT ( ) NAMED_UNIT ( * ) SI_UNIT ( .MILLI., .METRE. ) );
#11961 = EDGE_LOOP ( 'NONE', ( #29787, #722, #16067, #10842 ) ) ;
#11962 = CARTESIAN_POINT ( 'NONE',  ( -17.04621913067799710, -32.00000000058999916, -25.51324865459000080 ) ) ;
#11963 = ORIENTED_EDGE ( 'NONE', *, *, #14798, .T. ) ;
#11964 = CARTESIAN_POINT ( 'NONE',  ( 23.62697774660000150, -14.64965012210000062, 225.6806946080000102 ) ) ;
#11965 = CARTESIAN_POINT ( 'NONE',  ( 2.625702655411691566, 2.452149595252573366, 227.6997972603473386 ) ) ;
#11966 = CARTESIAN_POINT ( 'NONE',  ( -12.41421356240000051, 26.55509710711128335, -61.34142017886538412 ) ) ;
#11967 = CARTESIAN_POINT ( 'NONE',  ( 0.5618833952078471361, 4.215050809562369771, -35.70000000000000284 ) ) ;
#11968 = CIRCLE ( 'NONE', #3418, 4.987531172950001590 ) ;
#11969 = CARTESIAN_POINT ( 'NONE',  ( 11.08346179031909884, -28.41490585489484744, 143.6055512749999821 ) ) ;
#11970 = CARTESIAN_POINT ( 'NONE',  ( -2.993757627400086552, -2.302355992395527018, -0.6999999999999990674 ) ) ;
#11971 = CARTESIAN_POINT ( 'NONE',  ( 2.873028037699999811E-09, -3.314704954960000014E-09, 230.0000000000000000 ) ) ;
#11972 = DIRECTION ( 'NONE',  ( 0.000000000000000000, 0.000000000000000000, 1.000000000000000000 ) ) ;
#11973 = CARTESIAN_POINT ( 'NONE',  ( -5.857861475075242019, -1.837656413297739766, -10.02323088899999881 ) ) ;
#11974 = CARTESIAN_POINT ( 'NONE',  ( -1.611722395286938170, -6.291674585240492057, -27.54882611459999353 ) ) ;
#11975 = DIRECTION ( 'NONE',  ( -6.028162111955455897E-12, 0.4554456718800332649, 0.8902635789280302081 ) ) ;
#11976 = AXIS2_PLACEMENT_3D ( 'NONE', #955, #10545, #8159 ) ;
#11977 = CARTESIAN_POINT ( 'NONE',  ( -3.589938226060418902, -0.3047141992580486569, -93.72782450567366652 ) ) ;
#11978 = CARTESIAN_POINT ( 'NONE',  ( 19.68707593455170368, 19.53815609463533320, 0.6304112420000007599 ) ) ;
#11979 = CARTESIAN_POINT ( 'NONE',  ( 12.55799324160000019, 20.99999999999999645, -55.95247857500000066 ) ) ;
#11980 = CARTESIAN_POINT ( 'NONE',  ( -2.624260084387257219, -3.463915187244964056, -3.728945369300004753 ) ) ;
#11981 = PRODUCT_DEFINITION_SHAPE ( 'NONE', 'NONE',  #31144 ) ;
#11982 = CARTESIAN_POINT ( 'NONE',  ( 23.89202021435673728, -14.21382295584061417, 5.677594575767613172 ) ) ;
#11983 = CARTESIAN_POINT ( 'NONE',  ( 14.54393567127463172, -26.57411906178515082, -22.87237978256219151 ) ) ;
#11984 = CARTESIAN_POINT ( 'NONE',  ( 0.5453808542213991473, -3.499787565727024763, 230.8124249489340230 ) ) ;
#11985 = EDGE_CURVE ( 'NONE', #14204, #30811, #22723, .T. ) ;
#11986 = EDGE_LOOP ( 'NONE', ( #16450, #24988, #13985, #7192 ) ) ;
#11987 = AXIS2_PLACEMENT_3D ( 'NONE', #7254, #23637, #21264 ) ;
#11988 = EDGE_CURVE ( 'NONE', #18431, #9370, #18524, .T. ) ;
#11989 = CARTESIAN_POINT ( 'NONE',  ( -10.69999999999999929, 19.99999999999999645, -42.39999999999999858 ) ) ;
#11990 = DIRECTION ( 'NONE',  ( 0.000000000000000000, 1.000000000000000000, 0.000000000000000000 ) ) ;
#11991 = VERTEX_POINT ( 'NONE', #27328 ) ;
#11992 = B_SPLINE_CURVE_WITH_KNOTS ( 'NONE', 3,
 ( #17046, #21776, #2733, #386, #2579, #5544, #2882, #26957, #26494, #4936, #19570, #22088, #7450, #17505 ),
 .UNSPECIFIED., .F., .F.,
 ( 4, 2, 2, 1, 1, 2, 2, 4 ),
 ( 0.000000000000000000, 0.2500000000000167644, 0.3750000000000232592, 0.4375000000000246470, 0.4687500000000254796, 0.4843750000000243694, 0.5000000000000232037, 1.000000000000000000 ),
 .UNSPECIFIED. ) ;
#11993 = EDGE_CURVE ( 'NONE', #24893, #21140, #26847, .T. ) ;
#11994 = B_SPLINE_CURVE_WITH_KNOTS ( 'NONE', 3,
 ( #6084, #25770, #23250, #15682, #6711, #21046, #25293, #4201, #27802, #3729, #30646, #13802, #22937, #6251 ),
 .UNSPECIFIED., .F., .F.,
 ( 4, 2, 2, 1, 1, 2, 2, 4 ),
 ( 0.000000000000000000, 0.2499999999999499845, 0.3749999999999247269, 0.4374999999999122924, 0.4687499999999084621, 0.4843749999999067413, 0.4999999999999050759, 1.000000000000000000 ),
 .UNSPECIFIED. ) ;
#11995 = CARTESIAN_POINT ( 'NONE',  ( -22.97554992469999746, 15.65135060219999907, 222.0000000000000000 ) ) ;
#11996 = CARTESIAN_POINT ( 'NONE',  ( 8.000000000264140709, -18.27877680372071723, -30.94409471150577318 ) ) ;
#11997 = ORIENTED_EDGE ( 'NONE', *, *, #17550, .T. ) ;
#11998 = VERTEX_POINT ( 'NONE', #27629 ) ;
#11999 = ORIENTED_EDGE ( 'NONE', *, *, #15927, .F. ) ;
#12000 = ORIENTED_EDGE ( 'NONE', *, *, #1629, .T. ) ;
#12001 = CARTESIAN_POINT ( 'NONE',  ( 9.999999999958141927, -27.37998968026300872, -25.40000000000158309 ) ) ;
#12002 = CIRCLE ( 'NONE', #476, 2.000000000000000000 ) ;
#12003 = CARTESIAN_POINT ( 'NONE',  ( 28.49528339128749366, 0.5184828350247212558, 1.000000000000000888 ) ) ;
#12004 = B_SPLINE_CURVE_WITH_KNOTS ( 'NONE', 3,
 ( #17863, #20398, #22296, #15366, #10341, #19934, #10805, #8419, #3556, #12688 ),
 .UNSPECIFIED., .F., .F.,
 ( 4, 2, 2, 2, 4 ),
 ( 0.000000000000000000, 0.2500000000000000000, 0.5000000000000000000, 0.7500000000000000000, 1.000000000000000000 ),
 .UNSPECIFIED. ) ;
#12005 = DIRECTION ( 'NONE',  ( 1.000000000000000000, 0.000000000000000000, 0.000000000000000000 ) ) ;
#12006 = ORIENTED_EDGE ( 'NONE', *, *, #17325, .T. ) ;
#12007 = LINE ( 'NONE', #2567, #2109 ) ;
#12008 = CARTESIAN_POINT ( 'NONE',  ( 18.62349342026574917, 19.80369317695730302, 0.06728435000000199118 ) ) ;
#12009 = CARTESIAN_POINT ( 'NONE',  ( 10.69999999994971240, -29.61896394763918039, -20.12083078305406048 ) ) ;
#12010 = CARTESIAN_POINT ( 'NONE',  ( 2.970736324804301720, -3.997174458241568917, -0.6999965274516192215 ) ) ;
#12011 = ORIENTED_EDGE ( 'NONE', *, *, #16712, .T. ) ;
#12012 = CYLINDRICAL_SURFACE ( 'NONE', #14994, 27.50000000000000000 ) ;
#12013 = AXIS2_PLACEMENT_3D ( 'NONE', #3886, #17715, #20561 ) ;
#12014 = B_SPLINE_SURFACE_WITH_KNOTS ( 'NONE', 5, 1, ( 
 ( #23416, #11289 ),
 ( #1846, #11443 ),
 ( #26224, #23572 ),
 ( #30949, #8914 ),
 ( #18979, #26078 ),
 ( #9071, #6863 ),
 ( #11900, #21501 ),
 ( #2006, #4517 ),
 ( #28586, #18516 ),
 ( #28118, #31102 ),
 ( #16312, #14115 ),
 ( #6556, #20893 ),
 ( #21193, #13961 ),
 ( #7028, #6402 ),
 ( #25924, #4662 ) ),
 .UNSPECIFIED., .F., .F., .F.,
 ( 6, 3, 3, 3, 6 ),
 ( 2, 2 ),
 ( 0.000000000000000000, 0.5778133628420000223, 1.155626725680000133, 2.022346769939999955, 2.889066814210000000 ),
 ( -1.229628401229999994E-05, 0.7031504239110000221 ),
 .UNSPECIFIED. ) ;
#12015 = CARTESIAN_POINT ( 'NONE',  ( -2.227024806490486508, -3.476280271252723431, -18.70544088819999118 ) ) ;
#12016 = CARTESIAN_POINT ( 'NONE',  ( 2.131628207279999844E-14, 1.421085471519999843E-14, 230.7531949689999919 ) ) ;
#12017 = FACE_OUTER_BOUND ( 'NONE', #26973, .T. ) ;
#12018 = EDGE_LOOP ( 'NONE', ( #12855, #8143, #20774, #3833 ) ) ;
#12019 = CARTESIAN_POINT ( 'NONE',  ( 16.29938252758261186, 10.30810785441514454, -0.6999999999999783062 ) ) ;
#12020 = CARTESIAN_POINT ( 'NONE',  ( 24.48133297869999936, 13.22453720200000227, 222.0000000000000000 ) ) ;
#12021 = CARTESIAN_POINT ( 'NONE',  ( 22.63992238021892334, -14.34133587286723710, 5.097059004917531944 ) ) ;
#12022 = CARTESIAN_POINT ( 'NONE',  ( 6.760007715859398303, 5.672256964573851867, -40.24571374301982729 ) ) ;
#12023 = DIRECTION ( 'NONE',  ( 0.000000000000000000, -1.000000000000000000, 0.000000000000000000 ) ) ;
#12024 = CARTESIAN_POINT ( 'NONE',  ( 0.000000000000000000, 0.000000000000000000, 40.00000000000000000 ) ) ;
#12025 = CARTESIAN_POINT ( 'NONE',  ( 0.5184513693225318853, -28.49550581263314086, 3.899998581000013509 ) ) ;
#12026 = ORIENTED_EDGE ( 'NONE', *, *, #20386, .F. ) ;
#12027 = CIRCLE ( 'NONE', #14554, 26.80000000000000071 ) ;
#12028 = FACE_OUTER_BOUND ( 'NONE', #22447, .T. ) ;
#12029 = LINE ( 'NONE', #28854, #24181 ) ;
#12030 = B_SPLINE_CURVE_WITH_KNOTS ( 'NONE', 3,
 ( #28243, #23547, #1518, #15661, #10794, #20389, #27941, #6064, #28094, #15830, #6687, #10950, #6536, #3867, #30624, #16132, #25747, #25268, #25905, #23226, #16289, #11418, #1668, #30141, #21021, #9050, #3703, #22915, #13305, #11108, #18645, #18339, #1356, #15981, #20704, #30301, #6383, #11265, #20869, #30467, #8891, #18496, #19703, #9355, #22217, #29287, #7728, #6844, #17482, #26777, #7877, #10106, #3014, #22069, #30769, #12308, #24580, #28565, #21920, #4641, #29444, #12451, #7007, #24426, #17334, #21328, #2861, #15129, #2135, #26940, #366, #19551, #523 ),
 .UNSPECIFIED., .F., .F.,
 ( 4, 2, 1, 1, 1, 1, 2, 2, 1, 1, 1, 1, 1, 2, 2, 1, 1, 2, 2, 1, 1, 1, 1, 2, 2, 1, 1, 2, 2, 1, 1, 1, 2, 2, 1, 1, 1, 2, 2, 1, 2, 2, 1, 2, 2, 2, 2, 2, 4 ),
 ( 0.000000000000000000, 0.1250000000000015821, 0.1875000000000024425, 0.2187500000000028588, 0.2343750000000030809, 0.2421875000000031641, 0.2460937500000032196, 0.2500000000000032752, 0.3125000000000044409, 0.3437500000000050515, 0.3593750000000053846, 0.3671875000000055511, 0.3710937500000056621, 0.3730468750000056621, 0.3750000000000057176, 0.4062500000000063283, 0.4218750000000066058, 0.4296875000000067724, 0.4375000000000069389, 0.4531250000000072720, 0.4609375000000074940, 0.4648437500000076050, 0.4667968750000076050, 0.4677734375000076050, 0.4687500000000075495, 0.4843750000000066058, 0.4921875000000061617, 0.4960937500000061062, 0.5000000000000059952, 0.5156250000000046629, 0.5234375000000037748, 0.5273437500000033307, 0.5292968750000031086, 0.5312500000000029976, 0.5468750000000023315, 0.5546875000000021094, 0.5585937500000021094, 0.5605468750000019984, 0.5625000000000018874, 0.5937500000000017764, 0.6093750000000016653, 0.6250000000000016653, 0.6562500000000015543, 0.6718750000000015543, 0.6875000000000014433, 0.7187500000000013323, 0.7500000000000011102, 0.8750000000000006661, 1.000000000000000000 ),
 .UNSPECIFIED. ) ;
#12031 = EDGE_CURVE ( 'NONE', #4065, #14380, #1328, .T. ) ;
#12032 = FACE_OUTER_BOUND ( 'NONE', #24557, .T. ) ;
#12033 = CARTESIAN_POINT ( 'NONE',  ( 9.000000000000000000, -130.0000000000000000, -44.10000000000000142 ) ) ;
#12034 = EDGE_CURVE ( 'NONE', #25525, #10448, #29459, .T. ) ;
#12035 = VERTEX_POINT ( 'NONE', #13316 ) ;
#12036 = CARTESIAN_POINT ( 'NONE',  ( -3.181902231748757526, 1.609514238137835118, -88.52261276242234089 ) ) ;
#12037 =( NAMED_UNIT ( * ) PLANE_ANGLE_UNIT ( ) SI_UNIT ( $, .RADIAN. ) );
#12038 = B_SPLINE_CURVE_WITH_KNOTS ( 'NONE', 3,
 ( #1533, #18026, #30156, #20887, #13476, #11124 ),
 .UNSPECIFIED., .F., .F.,
 ( 4, 2, 4 ),
 ( 0.000000000000000000, 0.5000000000000000000, 1.000000000000000000 ),
 .UNSPECIFIED. ) ;
#12039 = ORIENTED_EDGE ( 'NONE', *, *, #25645, .F. ) ;
#12040 = CARTESIAN_POINT ( 'NONE',  ( 3.573234815572619905, 2.267560867816098558, -38.58513250291310470 ) ) ;
#12041 = CARTESIAN_POINT ( 'NONE',  ( 0.3196029497759475535, 5.089975830446680227, -69.35875473022500159 ) ) ;
#12042 = ORIENTED_EDGE ( 'NONE', *, *, #7790, .T. ) ;
#12043 = CARTESIAN_POINT ( 'NONE',  ( -5.430430790592723156, -2.746024268427175841, -27.96472909260000606 ) ) ;
#12044 = DIRECTION ( 'NONE',  ( 0.000000000000000000, 0.000000000000000000, 1.000000000000000000 ) ) ;
#12045 = COLOUR_RGB ( '', 0.72549020, 0.75294118, 0.79215686) ;
#12046 = AXIS2_PLACEMENT_3D ( 'NONE', #23405, #23560, #14105 ) ;
#12047 = CARTESIAN_POINT ( 'NONE',  ( 3.312932182603874232, 3.356011527877053702, -57.70805965152499795 ) ) ;
#12048 = CARTESIAN_POINT ( 'NONE',  ( -23.81569860410000317, -13.75000000000000000, 3.900000000369999942 ) ) ;
#12049 = DIRECTION ( 'NONE',  ( 0.000000000000000000, 0.000000000000000000, 1.000000000000000000 ) ) ;
#12050 = CARTESIAN_POINT ( 'NONE',  ( 24.68173674080000168, -14.25001227039999918, 223.9000014189999774 ) ) ;
#12051 = CLOSED_SHELL ( 'NONE', ( #5601, #4146, #28101, #12223, #6987, #8853, #16354, #13809, #6800, #6163, #8749, #9855, #14426, #19383, #21000, #7587, #29058, #4451, #466, #16963, #20153, #20188, #30783, #5713, #5777, #17618, #22730, #5513, #3624, #4809, #11573, #14129, #9782, #28894, #17937, #12766, #3460, #2297, #23557, #10415, #4330, #560, #5579, #28237, #10633, #22157, #1228, #12489 ) ) ;
#12052 = CARTESIAN_POINT ( 'NONE',  ( 8.700000000287184676, -13.53252229041972043, -36.25298318319556046 ) ) ;
#12053 = CARTESIAN_POINT ( 'NONE',  ( 9.999999999959607422, -29.15099216425362272, -26.30554312115310722 ) ) ;
#12054 = ORIENTED_EDGE ( 'NONE', *, *, #23476, .T. ) ;
#12055 = FACE_OUTER_BOUND ( 'NONE', #12123, .T. ) ;
#12056 = CARTESIAN_POINT ( 'NONE',  ( 24.09856112909999837, -15.21545593799999985, 225.0000014190000002 ) ) ;
#12057 = EDGE_CURVE ( 'NONE', #16896, #13818, #28419, .T. ) ;
#12058 = CARTESIAN_POINT ( 'NONE',  ( -4.751854023639999092, -11.13496319879999952, 231.9999989789999972 ) ) ;
#12059 = CARTESIAN_POINT ( 'NONE',  ( -27.79999999999999716, -2.358050544769999872E-11, 226.2000000000000171 ) ) ;
#12060 = DIRECTION ( 'NONE',  ( -1.553705081258626668E-12, 0.7253743710120288402, -0.6883545756940265825 ) ) ;
#12061 = FACE_OUTER_BOUND ( 'NONE', #27276, .T. ) ;
#12062 = CARTESIAN_POINT ( 'NONE',  ( -28.50000000000000000, 3.490128108389999698E-15, 90.00000000000000000 ) ) ;
#12063 = B_SPLINE_CURVE_WITH_KNOTS ( 'NONE', 1,
 ( #22161, #3108 ),
 .UNSPECIFIED., .F., .F.,
 ( 2, 2 ),
 ( -2.556331299420000144E-06, 0.7000000000009999335 ),
 .UNSPECIFIED. ) ;
#12064 = CARTESIAN_POINT ( 'NONE',  ( 3.510330247560000227, 1.917702154400000136, -44.00000000037249492 ) ) ;
#12065 = CARTESIAN_POINT ( 'NONE',  ( -5.009717977351991536, -17.07423824983273875, 230.0306840897816016 ) ) ;
#12066 = CARTESIAN_POINT ( 'NONE',  ( 4.374602741782418036, -11.28406995535170765, 232.0000002394077683 ) ) ;
#12067 = CARTESIAN_POINT ( 'NONE',  ( -18.95046173579999760, -18.95046173579999760, 186.7828584120000244 ) ) ;
#12068 = DIRECTION ( 'NONE',  ( 0.000000000000000000, 0.000000000000000000, -1.000000000000000000 ) ) ;
#12069 = VERTEX_POINT ( 'NONE', #4037 ) ;
#12070 = CARTESIAN_POINT ( 'NONE',  ( 7.105427357599999217E-15, 3.552713678799999608E-15, 193.6055512750000105 ) ) ;
#12071 = ORIENTED_EDGE ( 'NONE', *, *, #27532, .F. ) ;
#12072 = CARTESIAN_POINT ( 'NONE',  ( 24.58943550720000104, -12.96928235400000062, 225.3105417090000060 ) ) ;
#12073 = CARTESIAN_POINT ( 'NONE',  ( -3.855177830964256813, -4.571422008809257420, -59.65407541852500373 ) ) ;
#12074 = ORIENTED_EDGE ( 'NONE', *, *, #7284, .T. ) ;
#12075 = ORIENTED_EDGE ( 'NONE', *, *, #4208, .T. ) ;
#12076 = AXIS2_PLACEMENT_3D ( 'NONE', #8946, #11158, #15881 ) ;
#12077 = CARTESIAN_POINT ( 'NONE',  ( -23.41419870089999833, 16.84247076400000154, 229.0000000000000000 ) ) ;
#12078 = VERTEX_POINT ( 'NONE', #6394 ) ;
#12079 = CARTESIAN_POINT ( 'NONE',  ( 0.000000000000000000, 0.000000000000000000, 115.0000000000000000 ) ) ;
#12080 = CARTESIAN_POINT ( 'NONE',  ( -5.945069363104309446, -15.39359683734632611, -109.1271631200178547 ) ) ;
#12081 = CARTESIAN_POINT ( 'NONE',  ( -27.07233446881437899, 8.380004974182886812, 8.000000000000007105 ) ) ;
#12082 = EDGE_CURVE ( 'NONE', #2058, #19001, #9571, .T. ) ;
#12083 = CARTESIAN_POINT ( 'NONE',  ( 8.161936297539998719, -9.194081254939998615, 232.6627648150000027 ) ) ;
#12084 = DIRECTION ( 'NONE',  ( 0.8775825618903722036, 0.4794255386042041156, 0.000000000000000000 ) ) ;
#12085 = CARTESIAN_POINT ( 'NONE',  ( 5.506451109007332256, 0.7220432749125509364, -4.626979598400001947 ) ) ;
#12086 = CARTESIAN_POINT ( 'NONE',  ( 28.35924375250000296, -2.486899575159999765E-14, 229.7625741969999922 ) ) ;
#12087 = VERTEX_POINT ( 'NONE', #11279 ) ;
#12088 = CARTESIAN_POINT ( 'NONE',  ( -1.459689923256333843, -4.879907760210503653, -44.10000000002499121 ) ) ;
#12089 = EDGE_CURVE ( 'NONE', #22839, #3906, #1440, .T. ) ;
#12090 = CARTESIAN_POINT ( 'NONE',  ( -6.228182343209494043, 0.8662545139425728014, -19.25159460730001371 ) ) ;
#12091 = DIRECTION ( 'NONE',  ( -0.9595496299847263710, 0.2815395311429191305, 0.000000000000000000 ) ) ;
#12092 = DIRECTION ( 'NONE',  ( 1.000000000000000000, -1.224606353819998843E-16, 0.000000000000000000 ) ) ;
#12093 = CARTESIAN_POINT ( 'NONE',  ( -9.954078586509998772, -7.027540153349999485, 230.6412452697800006 ) ) ;
#12094 = DIRECTION ( 'NONE',  ( 1.000000000000000000, 0.000000000000000000, 0.000000000000000000 ) ) ;
#12095 = CARTESIAN_POINT ( 'NONE',  ( -19.29841003509485375, 19.63499152630128108, 0.3044381840000276451 ) ) ;
#12096 = DIRECTION ( 'NONE',  ( 1.000000000000000000, 0.000000000000000000, 0.000000000000000000 ) ) ;
#12097 = CARTESIAN_POINT ( 'NONE',  ( 0.9242233386863408784, -26.78436825977087565, 224.4020708179980659 ) ) ;
#12098 = CARTESIAN_POINT ( 'NONE',  ( 1.030019577584203890E-10, -106.6790623149837245, 18.95265870294618082 ) ) ;
#12099 = EDGE_CURVE ( 'NONE', #3424, #21696, #30941, .T. ) ;
#12100 = CARTESIAN_POINT ( 'NONE',  ( -16.83342759575507586, 10.99999999997565503, -0.6999999999999784173 ) ) ;
#12101 = ORIENTED_EDGE ( 'NONE', *, *, #18448, .F. ) ;
#12102 = CARTESIAN_POINT ( 'NONE',  ( -4.274658871253808279, -0.8336587121505223408, -31.59652066320000330 ) ) ;
#12103 = CARTESIAN_POINT ( 'NONE',  ( 9.599999999813990215, -13.94068574325910426, -36.43083477791316227 ) ) ;
#12104 = ORIENTED_EDGE ( 'NONE', *, *, #805, .T. ) ;
#12105 = CARTESIAN_POINT ( 'NONE',  ( 24.08956650209805872, -13.26503430050375876, 4.040453396065998959 ) ) ;
#12106 = CARTESIAN_POINT ( 'NONE',  ( 5.200437648300224147, 1.853818095060352222, -46.72627377572500507 ) ) ;
#12107 = EDGE_LOOP ( 'NONE', ( #10029, #20668, #449, #10506, #2984 ) ) ;
#12108 = ORIENTED_EDGE ( 'NONE', *, *, #1449, .F. ) ;
#12109 = CARTESIAN_POINT ( 'NONE',  ( 0.000000000000000000, 0.000000000000000000, 0.000000000000000000 ) ) ;
#12110 = VECTOR ( 'NONE', #28496, 1000.000000000000000 ) ;
#12111 = VERTEX_POINT ( 'NONE', #1530 ) ;
#12112 = CARTESIAN_POINT ( 'NONE',  ( -7.999999999730073696, -28.07052495761531219, -25.59750966829892960 ) ) ;
#12113 = ORIENTED_EDGE ( 'NONE', *, *, #8628, .T. ) ;
#12114 = DIRECTION ( 'NONE',  ( -0.9316362575375349842, 0.3633921898465292122, -0.000000000000000000 ) ) ;
#12115 = CARTESIAN_POINT ( 'NONE',  ( 3.748453146079709697, -2.489798990173139437, -0.6999999999999992895 ) ) ;
#12116 = DIRECTION ( 'NONE',  ( -1.000000000000000000, 6.565028073413479156E-24, -2.257144471327815248E-12 ) ) ;
#12117 = CARTESIAN_POINT ( 'NONE',  ( 1.101338864442481968, 3.961910147693631590, -35.69999999999999574 ) ) ;
#12118 = CARTESIAN_POINT ( 'NONE',  ( 18.12303402403091113, 19.99995697021033081, -0.6894527066783940894 ) ) ;
#12119 = EDGE_CURVE ( 'NONE', #8812, #5207, #4664, .T. ) ;
#12120 = CARTESIAN_POINT ( 'NONE',  ( -24.32472894358752313, 13.45989150749028873, 6.099998581000020792 ) ) ;
#12121 = CARTESIAN_POINT ( 'NONE',  ( -5.991145565605879852, -7.574673455881642425, -33.78475407894417515 ) ) ;
#12122 = CARTESIAN_POINT ( 'NONE',  ( -24.05392374927932053, 13.13253365033636477, -0.6999999999999784173 ) ) ;
#12123 = EDGE_LOOP ( 'NONE', ( #6887, #10182, #29753, #21888 ) ) ;
#12124 = EDGE_CURVE ( 'NONE', #20972, #15836, #8441, .T. ) ;
#12125 = CARTESIAN_POINT ( 'NONE',  ( 4.689100480956518879, -0.8300439969826994835, -9.708982634699996339 ) ) ;
#12126 = CARTESIAN_POINT ( 'NONE',  ( 6.118976883090258667, 2.212479739890888197, -26.51249766020000109 ) ) ;
#12127 = CARTESIAN_POINT ( 'NONE',  ( -2.635643612059070051, -2.346759556412466363, 0.000000000000000000 ) ) ;
#12128 = CARTESIAN_POINT ( 'NONE',  ( -8.700000000050449600, -115.5267901941123370, 21.04701626955306537 ) ) ;
#12129 = FACE_OUTER_BOUND ( 'NONE', #1944, .T. ) ;
#12130 = CARTESIAN_POINT ( 'NONE',  ( -23.76736455417796279, -13.83371703020049637, 226.1000000000011312 ) ) ;
#12131 = CARTESIAN_POINT ( 'NONE',  ( 9.509259942401945054, -25.80376675868338765, 25.15654267891509122 ) ) ;
#12132 = CARTESIAN_POINT ( 'NONE',  ( 1.348918213770415653, 4.124136235849971577, -11.07047964830000453 ) ) ;
#12133 = AXIS2_PLACEMENT_3D ( 'NONE', #30414, #9306, #11204 ) ;
#12134 = CARTESIAN_POINT ( 'NONE',  ( 16.20123158649999695, 11.52736809289999620, -1.399999999999998579 ) ) ;
#12135 = CARTESIAN_POINT ( 'NONE',  ( -24.41841039498785193, -14.69667350221323865, 3.899998581000013509 ) ) ;
#12136 = CARTESIAN_POINT ( 'NONE',  ( -1.650600432482589808, -3.499825479288129593, 230.6249086619309310 ) ) ;
#12137 = ORIENTED_EDGE ( 'NONE', *, *, #2464, .F. ) ;
#12138 = CARTESIAN_POINT ( 'NONE',  ( -8.699999999674142614, -13.61360970150653316, -34.64062719139432289 ) ) ;
#12139 = CARTESIAN_POINT ( 'NONE',  ( -12.75378086759999796, -32.00000000058999916, -25.51324865459000080 ) ) ;
#12140 = ORIENTED_EDGE ( 'NONE', *, *, #1690, .F. ) ;
#12141 = EDGE_CURVE ( 'NONE', #20382, #25546, #16499, .T. ) ;
#12142 = DIRECTION ( 'NONE',  ( -2.764840495839172918E-12, -0.9128796883888953273, 0.4082287037029531107 ) ) ;
#12143 = CARTESIAN_POINT ( 'NONE',  ( 24.16679028237082960, 15.10730797463399000, 3.997250016000014838 ) ) ;
#12144 = ORIENTED_EDGE ( 'NONE', *, *, #30380, .F. ) ;
#12145 = PRODUCT_RELATED_PRODUCT_CATEGORY ( 'part', '', ( #16179 ) ) ;
#12146 = ORIENTED_EDGE ( 'NONE', *, *, #24678, .T. ) ;
#12147 = VERTEX_POINT ( 'NONE', #16456 ) ;
#12148 = ORIENTED_EDGE ( 'NONE', *, *, #29066, .T. ) ;
#12149 = LINE ( 'NONE', #28987, #22026 ) ;
#12150 = FACE_OUTER_BOUND ( 'NONE', #1051, .T. ) ;
#12151 = CARTESIAN_POINT ( 'NONE',  ( 16.63016908737474253, 10.02891580959015094, -0.6999999999999784173 ) ) ;
#12152 = ORIENTED_EDGE ( 'NONE', *, *, #7072, .T. ) ;
#12153 = CARTESIAN_POINT ( 'NONE',  ( -24.83827471527357744, 12.48687850854618198, 5.104216618000034345 ) ) ;
#12154 = AXIS2_PLACEMENT_3D ( 'NONE', #29229, #5623, #2959 ) ;
#12155 = LINE ( 'NONE', #11699, #22588 ) ;
#12156 = EDGE_CURVE ( 'NONE', #553, #16515, #21185, .T. ) ;
#12157 = CARTESIAN_POINT ( 'NONE',  ( -10.14902473071754940, -26.01926976409365722, 87.93968498540000667 ) ) ;
#12158 = FACE_OUTER_BOUND ( 'NONE', #20008, .T. ) ;
#12159 = CARTESIAN_POINT ( 'NONE',  ( 3.380278521335310593, -3.553170434758972096, -0.6997606425626067272 ) ) ;
#12160 = ORIENTED_EDGE ( 'NONE', *, *, #7334, .F. ) ;
#12161 = LINE ( 'NONE', #29885, #17008 ) ;
#12162 = EDGE_CURVE ( 'NONE', #21103, #17104, #5768, .T. ) ;
#12163 = CARTESIAN_POINT ( 'NONE',  ( 3.800013225884300905, -1.579422177728472487, -17.37122516810000405 ) ) ;
#12164 = DIRECTION ( 'NONE',  ( -0.000000000000000000, -0.9396926207858126157, -0.3420201433259318913 ) ) ;
#12165 = LINE ( 'NONE', #9814, #10019 ) ;
#12166 = DIRECTION ( 'NONE',  ( 0.000000000000000000, 0.3420201433259318913, -0.9396926207858126157 ) ) ;
#12167 = CARTESIAN_POINT ( 'NONE',  ( -10.69999999999999929, -29.30501631370000482, -26.47986984990000181 ) ) ;
#12168 = CARTESIAN_POINT ( 'NONE',  ( -8.699999998988344529, -24.19750589173278499, -27.32947359979484858 ) ) ;
#12169 = EDGE_CURVE ( 'NONE', #2554, #9917, #13998, .T. ) ;
#12170 = CARTESIAN_POINT ( 'NONE',  ( 10.69999999999999929, -77.50000000000000000, -29.00566191750000300 ) ) ;
#12171 = CARTESIAN_POINT ( 'NONE',  ( 6.379024725906915272, -4.237078256518207908, -35.69999999999999574 ) ) ;
#12172 = CARTESIAN_POINT ( 'NONE',  ( 24.82944511390000031, 13.78896019239999937, 229.1414195099999915 ) ) ;
#12173 = CARTESIAN_POINT ( 'NONE',  ( 3.511461757819999807, 17.90077826259999938, 230.6999999999999886 ) ) ;
#12174 = EDGE_LOOP ( 'NONE', ( #17744, #28264, #26407, #30429, #9591, #5603, #24441, #23715, #13892, #23658 ) ) ;
#12175 = AXIS2_PLACEMENT_3D ( 'NONE', #18436, #2241, #21270 ) ;
#12176 = CARTESIAN_POINT ( 'NONE',  ( -1.100001419170000050, -27.77850706310000106, 225.0000014190000002 ) ) ;
#12177 = CYLINDRICAL_SURFACE ( 'NONE', #26884, 3.000000000000002220 ) ;
#12178 = CARTESIAN_POINT ( 'NONE',  ( 23.81866173088643635, 14.33570044285385947, 6.099998581000020792 ) ) ;
#12179 = ORIENTED_EDGE ( 'NONE', *, *, #9821, .T. ) ;
#12180 = CARTESIAN_POINT ( 'NONE',  ( -2.888061030901512893, 2.091444806125899891, -88.52261276243450538 ) ) ;
#12181 = ORIENTED_EDGE ( 'NONE', *, *, #23125, .F. ) ;
#12182 = CARTESIAN_POINT ( 'NONE',  ( 3.861721477338985409, 1.529807325115373207, -38.22530605780803370 ) ) ;
#12183 = APPLICATION_CONTEXT ( 'automotive_design' ) ;
#12184 = CARTESIAN_POINT ( 'NONE',  ( -5.167095691178253070, 1.703695954683749125, -69.54019511502499995 ) ) ;
#12185 = ORIENTED_EDGE ( 'NONE', *, *, #840, .F. ) ;
#12186 = CARTESIAN_POINT ( 'NONE',  ( -0.4514894588696777289, 4.335480228600245844, -25.88903409329999761 ) ) ;
#12187 = DIRECTION ( 'NONE',  ( 0.000000000000000000, 0.000000000000000000, -1.000000000000000000 ) ) ;
#12188 = CARTESIAN_POINT ( 'NONE',  ( 4.692739937114380311, 0.5303478879429834869, -55.01771407622499765 ) ) ;
#12189 = EDGE_CURVE ( 'NONE', #11066, #9001, #30637, .T. ) ;
#12190 = CARTESIAN_POINT ( 'NONE',  ( 8.700000000232341435, -25.77531388888509056, -25.66136093477824431 ) ) ;
#12191 = AXIS2_PLACEMENT_3D ( 'NONE', #1306, #17956, #27567 ) ;
#12192 = CARTESIAN_POINT ( 'NONE',  ( 17.47295178719334530, -10.06576768799940247, -0.6999999999999785283 ) ) ;
#12193 = B_SPLINE_SURFACE_WITH_KNOTS ( 'NONE', 5, 1, ( 
 ( #23893, #4987 ),
 ( #29202, #14598 ),
 ( #7040, #126 ),
 ( #286, #21829 ),
 ( #17246, #26853 ),
 ( #19466, #24187 ) ),
 .UNSPECIFIED., .F., .F., .F.,
 ( 6, 6 ),
 ( 2, 2 ),
 ( 0.000000000000000000, 2.000000000000000000 ),
 ( -2.345346139519999876E-15, 0.7000000000189999794 ),
 .UNSPECIFIED. ) ;
#12194 = DIRECTION ( 'NONE',  ( -9.228728892204885548E-13, -0.9128796883888958824, 0.4082287037029517784 ) ) ;
#12195 = PRODUCT_DEFINITION_CONTEXT ( 'detailed design', #4757, 'design' ) ;
#12196 = ADVANCED_FACE ( 'NONE', ( #9062 ), #13635, .T. ) ;
#12197 = CARTESIAN_POINT ( 'NONE',  ( -2.332928517029999895E-09, 3.208345589200000119E-09, 230.0000000000000000 ) ) ;
#12198 = ADVANCED_FACE ( 'NONE', ( #4190 ), #15993, .T. ) ;
#12199 = EDGE_CURVE ( 'NONE', #3580, #16174, #3541, .T. ) ;
#12200 = CARTESIAN_POINT ( 'NONE',  ( -17.48420900742436146, -22.00016259987420852, -28.84610937565356892 ) ) ;
#12201 = ORIENTED_EDGE ( 'NONE', *, *, #26945, .F. ) ;
#12202 = CARTESIAN_POINT ( 'NONE',  ( -26.80000000069999899, 3.281945028329999726E-15, 192.8898184869999852 ) ) ;
#12203 = DIRECTION ( 'NONE',  ( -1.224606353819999829E-16, -1.000000000000000000, 0.000000000000000000 ) ) ;
#12204 = CARTESIAN_POINT ( 'NONE',  ( -9.150307869779998882, 8.210980247390001097, 232.6627643349999914 ) ) ;
#12205 = DIRECTION ( 'NONE',  ( -1.000000000000000000, 0.000000000000000000, 0.000000000000000000 ) ) ;
#12206 = CARTESIAN_POINT ( 'NONE',  ( 19.80538212960000166, 19.50875458629999670, 229.0000000010000178 ) ) ;
#12207 = CARTESIAN_POINT ( 'NONE',  ( 10.69999999999596341, -130.0000000000000000, -40.61155403991316604 ) ) ;
#12208 = DIRECTION ( 'NONE',  ( -0.000000000000000000, -0.9396926207858126157, -0.3420201433259318913 ) ) ;
#12209 = CARTESIAN_POINT ( 'NONE',  ( 14.37503218006001049, -27.59354456826596191, -0.2432540810000105580 ) ) ;
#12210 = CARTESIAN_POINT ( 'NONE',  ( -0.09707459355099370968, -26.79999999950000955, 226.1000000000000512 ) ) ;
#12211 = DIRECTION ( 'NONE',  ( 0.000000000000000000, 0.000000000000000000, -1.000000000000000000 ) ) ;
#12212 = FACE_OUTER_BOUND ( 'NONE', #19547, .T. ) ;
#12213 = MECHANICAL_DESIGN_GEOMETRIC_PRESENTATION_REPRESENTATION (  '', ( #3182 ), #30330 ) ;
#12214 = CARTESIAN_POINT ( 'NONE',  ( -7.999999999730073696, -28.07052495761531219, -25.59750966829892960 ) ) ;
#12215 = CARTESIAN_POINT ( 'NONE',  ( -23.81569860410000317, -13.75000000000000000, 223.8999999999999773 ) ) ;
#12216 = CARTESIAN_POINT ( 'NONE',  ( 24.43659368183839931, 14.66646236428692340, 6.099998581000020792 ) ) ;
#12217 = CIRCLE ( 'NONE', #29797, 4.999999999999998224 ) ;
#12218 = ORIENTED_EDGE ( 'NONE', *, *, #10034, .F. ) ;
#12219 = CARTESIAN_POINT ( 'NONE',  ( 19.80526555972147307, 19.50877392102524155, 3.000000000000002665 ) ) ;
#12220 = SURFACE_STYLE_USAGE ( .BOTH. , #14599 ) ;
#12221 = ORIENTED_EDGE ( 'NONE', *, *, #8988, .F. ) ;
#12222 = CARTESIAN_POINT ( 'NONE',  ( 25.20859211119999799, -13.29584934979999922, 225.3105417090000060 ) ) ;
#12223 = ADVANCED_FACE ( 'NONE', ( #16609 ), #21951, .T. ) ;
#12224 = CARTESIAN_POINT ( 'NONE',  ( -4.072259770650454413, 2.021700601781299511, -56.79877225282499609 ) ) ;
#12225 = ORIENTED_EDGE ( 'NONE', *, *, #21114, .T. ) ;
#12226 = VERTEX_POINT ( 'NONE', #3328 ) ;
#12227 = DIRECTION ( 'NONE',  ( 0.9316362575375348731, -0.3633921898465292122, 0.000000000000000000 ) ) ;
#12228 = ORIENTED_EDGE ( 'NONE', *, *, #107, .T. ) ;
#12229 = ORIENTED_EDGE ( 'NONE', *, *, #21977, .T. ) ;
#12230 = DIRECTION ( 'NONE',  ( -0.2815395311429196301, -0.9595496299847262600, 0.000000000000000000 ) ) ;
#12231 = CONICAL_SURFACE ( 'NONE', #19273, 4.997501249379996402, 1.047197551199999799 ) ;
#12232 = CARTESIAN_POINT ( 'NONE',  ( -23.77947513073445407, 14.40125622634048774, 4.791564337000009388 ) ) ;
#12233 =( NAMED_UNIT ( * ) SI_UNIT ( $, .STERADIAN. ) SOLID_ANGLE_UNIT ( ) );
#12234 = VECTOR ( 'NONE', #8890, 1000.000000000000000 ) ;
#12235 = CARTESIAN_POINT ( 'NONE',  ( -10.00000000000000000, -55.00000000000000000, -42.39999999999999858 ) ) ;
#12236 = CARTESIAN_POINT ( 'NONE',  ( -20.30403093128963476, 20.00000000003735323, 3.000000106999994642 ) ) ;
#12237 = CARTESIAN_POINT ( 'NONE',  ( -4.484282906631563925, 1.269983465873031347, -6.810827254900003958 ) ) ;
#12238 = CARTESIAN_POINT ( 'NONE',  ( 28.49999999970000175, -7.466149220240000162, 229.0000000000000000 ) ) ;
#12239 = EDGE_LOOP ( 'NONE', ( #22182, #22219, #30284, #20713 ) ) ;
#12240 = PLANE ( 'NONE',  #19003 ) ;
#12241 = LINE ( 'NONE', #9887, #3226 ) ;
#12242 = CARTESIAN_POINT ( 'NONE',  ( -4.448701673712592175, 0.6187532242676700989, -19.75159460729999950 ) ) ;
#12243 = CARTESIAN_POINT ( 'NONE',  ( 0.6616560533698909730, 3.499999999999999112, 230.8013441257845102 ) ) ;
#12244 = DIRECTION ( 'NONE',  ( 1.000000000000000000, 0.000000000000000000, 0.000000000000000000 ) ) ;
#12245 = DIRECTION ( 'NONE',  ( 1.000000000000000000, -3.981000000000000101E-12, 1.940999999999999908E-12 ) ) ;
#12246 = CARTESIAN_POINT ( 'NONE',  ( -15.77518214703643729, -8.674270198554944855, 0.000000000000000000 ) ) ;
#12247 = CARTESIAN_POINT ( 'NONE',  ( 2.766343654246206984, -4.329863758072034940, -42.76966640442500989 ) ) ;
#12248 = CARTESIAN_POINT ( 'NONE',  ( 10.69999999999999929, -25.00000000000000000, -26.16393202249999916 ) ) ;
#12249 = CARTESIAN_POINT ( 'NONE',  ( 4.276011752472853367, -9.320059656523383751, -25.35190844153497380 ) ) ;
#12250 = DIRECTION ( 'NONE',  ( 1.000000000000000000, 0.000000000000000000, 0.000000000000000000 ) ) ;
#12251 = CARTESIAN_POINT ( 'NONE',  ( -18.50496050090000111, 20.74627092869999956, 229.0000000010000178 ) ) ;
#12252 = AXIS2_PLACEMENT_3D ( 'NONE', #9347, #16277, #14237 ) ;
#12253 = EDGE_CURVE ( 'NONE', #15738, #9398, #17035, .T. ) ;
#12254 = AXIS2_PLACEMENT_3D ( 'NONE', #5133, #14746, #24343 ) ;
#12255 = VECTOR ( 'NONE', #6496, 1000.000000000000000 ) ;
#12256 = DIRECTION ( 'NONE',  ( 0.000000000000000000, -1.000000000000000000, 0.000000000000000000 ) ) ;
#12257 = ORIENTED_EDGE ( 'NONE', *, *, #3864, .F. ) ;
#12258 = AXIS2_PLACEMENT_3D ( 'NONE', #8592, #20725, #27637 ) ;
#12259 = VECTOR ( 'NONE', #22184, 1000.000000000000000 ) ;
#12260 = CARTESIAN_POINT ( 'NONE',  ( 3.999349870826697018, -3.799712354642017509, -31.05126389020000133 ) ) ;
#12261 = CARTESIAN_POINT ( 'NONE',  ( -26.80000000000000071, -8.704148513059999178E-14, 230.6999999999999886 ) ) ;
#12262 = ORIENTED_EDGE ( 'NONE', *, *, #22228, .T. ) ;
#12263 = CARTESIAN_POINT ( 'NONE',  ( -9.999999999949999108, -30.49286765380000119, -21.04171673159999756 ) ) ;
#12264 = CARTESIAN_POINT ( 'NONE',  ( -4.251243323665415907, -4.132078999800212316, -47.20083066912499703 ) ) ;
#12265 = ORIENTED_EDGE ( 'NONE', *, *, #12332, .F. ) ;
#12266 = EDGE_CURVE ( 'NONE', #26442, #17734, #19130, .T. ) ;
#12267 = ORIENTED_EDGE ( 'NONE', *, *, #10355, .T. ) ;
#12268 = DIRECTION ( 'NONE',  ( 1.000000000000000000, 0.000000000000000000, 0.000000000000000000 ) ) ;
#12269 = ORIENTED_EDGE ( 'NONE', *, *, #13979, .F. ) ;
#12270 = CARTESIAN_POINT ( 'NONE',  ( -7.999999999729050515, -26.29567537037302927, -25.46710523971266582 ) ) ;
#12271 = EDGE_LOOP ( 'NONE', ( #601, #29097, #24843, #5485 ) ) ;
#12272 = CARTESIAN_POINT ( 'NONE',  ( -25.22658730140000216, -13.26242337740000110, 225.0000014190000002 ) ) ;
#12273 = DIRECTION ( 'NONE',  ( 0.8090169943751909232, 0.5877852522921378498, 0.000000000000000000 ) ) ;
#12274 = DIRECTION ( 'NONE',  ( -1.000000000000000000, 8.856532914347465582E-13, -1.659169102000414711E-12 ) ) ;
#12275 = CARTESIAN_POINT ( 'NONE',  ( 1.232334062959267840, 4.717565258337718781, -35.70000000000000284 ) ) ;
#12276 = CARTESIAN_POINT ( 'NONE',  ( 8.700000000285857737, -13.61366271048277277, -34.64064744186795508 ) ) ;
#12277 = CARTESIAN_POINT ( 'NONE',  ( 9.499999999936914463, -14.38471058642483769, -37.28629371922507119 ) ) ;
#12278 = CARTESIAN_POINT ( 'NONE',  ( -23.06380069493458862, -13.64989377471593279, 6.071490516014675265 ) ) ;
#12279 = AXIS2_PLACEMENT_3D ( 'NONE', #25966, #18406, #3939 ) ;
#12280 = CARTESIAN_POINT ( 'NONE',  ( -23.50695179570000093, -14.84192241259999889, 225.0000014190000002 ) ) ;
#12281 = MECHANICAL_DESIGN_GEOMETRIC_PRESENTATION_REPRESENTATION (  '', ( #5739 ), #28855 ) ;
#12282 = ORIENTED_EDGE ( 'NONE', *, *, #23155, .F. ) ;
#12283 = TOROIDAL_SURFACE ( 'NONE', #16301, 30.50000000000000000, 3.000000000000000000 ) ;
#12284 = AXIS2_PLACEMENT_3D ( 'NONE', #17007, #26609, #185 ) ;
#12285 = CARTESIAN_POINT ( 'NONE',  ( -5.530047734074942767, 3.478668956039820959, -10.44547590279999660 ) ) ;
#12286 = CARTESIAN_POINT ( 'NONE',  ( -1.151230282303593366, -4.494053275198268693, -27.54882611460000774 ) ) ;
#12287 = VECTOR ( 'NONE', #1655, 1000.000000000000000 ) ;
#12288 = CARTESIAN_POINT ( 'NONE',  ( 3.040504021322313122, 1.733590290792417887, 0.000000000000000000 ) ) ;
#12289 = EDGE_CURVE ( 'NONE', #17932, #10339, #25567, .T. ) ;
#12290 = CARTESIAN_POINT ( 'NONE',  ( 23.77307140678977504, -14.41181874416537134, 5.104215870000011535 ) ) ;
#12291 = CARTESIAN_POINT ( 'NONE',  ( 24.05769993097117876, 13.93129956312566620, 6.002748562000004284 ) ) ;
#12292 = CARTESIAN_POINT ( 'NONE',  ( -10.00000000000000000, 22.40709319595134730, -62.85117013414870257 ) ) ;
#12293 = CARTESIAN_POINT ( 'NONE',  ( 1.099998580829999906, -27.77839262550000043, 225.1040528159999781 ) ) ;
#12294 = CARTESIAN_POINT ( 'NONE',  ( 0.3624384587677526026, -4.645391411234340850, -9.393384211799999051 ) ) ;
#12295 = CARTESIAN_POINT ( 'NONE',  ( 0.000000000000000000, -1.776356839399999804E-15, 227.6412452697800006 ) ) ;
#12296 = CARTESIAN_POINT ( 'NONE',  ( -24.36724936496760918, -13.38201651699120021, 4.999998581000003384 ) ) ;
#12297 = LINE ( 'NONE', #14821, #29362 ) ;
#12298 = ORIENTED_EDGE ( 'NONE', *, *, #22370, .F. ) ;
#12299 = CARTESIAN_POINT ( 'NONE',  ( -1.058439502263211374, 6.005994971325610443, -19.83583244400000112 ) ) ;
#12300 = DIRECTION ( 'NONE',  ( 0.000000000000000000, 0.000000000000000000, 1.000000000000000000 ) ) ;
#12301 = CARTESIAN_POINT ( 'NONE',  ( 1.976074114793839431, -0.3084332875059760948, 229.1412452697749984 ) ) ;
#12302 = VERTEX_POINT ( 'NONE', #5692 ) ;
#12303 = B_SPLINE_SURFACE_WITH_KNOTS ( 'NONE', 5, 1, ( 
 ( #8810, #30061 ),
 ( #11029, #28011 ),
 ( #8491, #11178 ),
 ( #22672, #22988 ),
 ( #6305, #1434 ),
 ( #25507, #16056 ),
 ( #18412, #1118 ),
 ( #6454, #29908 ),
 ( #2936, #9119 ),
 ( #289, #444 ),
 ( #14747, #1898 ),
 ( #14903, #28906 ),
 ( #19620, #9274 ),
 ( #9867, #4988 ),
 ( #28320, #5134 ) ),
 .UNSPECIFIED., .F., .F., .F.,
 ( 6, 3, 3, 3, 6 ),
 ( 2, 2 ),
 ( 0.000000000000000000, 0.5239049114000000618, 1.047809822800000124, 1.571714734199999963, 1.746349704670000058 ),
 ( -0.7000000000009999335, 2.557517976399999938E-06 ),
 .UNSPECIFIED. ) ;
#12304 = CARTESIAN_POINT ( 'NONE',  ( 7.636616881710000193, 9.305349148710000406, 230.6412452697800006 ) ) ;
#12305 = DIRECTION ( 'NONE',  ( 0.000000000000000000, 0.3420201433259318913, -0.9396926207858126157 ) ) ;
#12306 = AXIS2_PLACEMENT_3D ( 'NONE', #1938, #11683, #11532 ) ;
#12307 = ORIENTED_EDGE ( 'NONE', *, *, #6151, .F. ) ;
#12308 = CARTESIAN_POINT ( 'NONE',  ( -4.789018076886207176, 0.4073481513306022039, -44.10000000002499831 ) ) ;
#12309 = ORIENTED_EDGE ( 'NONE', *, *, #10289, .F. ) ;
#12310 = EDGE_CURVE ( 'NONE', #974, #8453, #13693, .T. ) ;
#12311 = ORIENTED_EDGE ( 'NONE', *, *, #29602, .F. ) ;
#12312 = B_SPLINE_CURVE_WITH_KNOTS ( 'NONE', 3,
 ( #10956, #29984, #22921, #8417, #14947, #25442 ),
 .UNSPECIFIED., .F., .F.,
 ( 4, 2, 4 ),
 ( 0.000000000000000000, 0.5000000000000000000, 1.000000000000000000 ),
 .UNSPECIFIED. ) ;
#12313 = ORIENTED_EDGE ( 'NONE', *, *, #14303, .T. ) ;
#12314 = CARTESIAN_POINT ( 'NONE',  ( -17.49999999969999465, -26.60251055750184079, -31.40006728715443529 ) ) ;
#12315 = DIRECTION ( 'NONE',  ( 1.000000000000000000, 0.000000000000000000, 0.000000000000000000 ) ) ;
#12316 = CARTESIAN_POINT ( 'NONE',  ( -27.79999999999999716, -2.354383354940000152E-11, 222.0000000000000000 ) ) ;
#12317 = EDGE_LOOP ( 'NONE', ( #8772, #3747, #15364, #23439 ) ) ;
#12318 = CARTESIAN_POINT ( 'NONE',  ( 10.99999999979999998, 20.99999999999999645, -67.09999999999999432 ) ) ;
#12319 = CARTESIAN_POINT ( 'NONE',  ( -15.44356573478999906, -26.99999999999999289, -28.40000000003218972 ) ) ;
#12320 = CARTESIAN_POINT ( 'NONE',  ( -17.38918303935544074, -31.99979622920404054, -29.75246175266256898 ) ) ;
#12321 = CIRCLE ( 'NONE', #4284, 26.80000000340000099 ) ;
#12322 = DIRECTION ( 'NONE',  ( 0.000000000000000000, -2.256683728769999802E-12, -1.000000000000000000 ) ) ;
#12323 = EDGE_CURVE ( 'NONE', #14421, #13324, #27060, .T. ) ;
#12324 = ORIENTED_EDGE ( 'NONE', *, *, #17270, .T. ) ;
#12325 = EDGE_CURVE ( 'NONE', #15501, #22831, #15141, .T. ) ;
#12326 = CARTESIAN_POINT ( 'NONE',  ( -5.420006065778396831, -1.021773059489365032, -15.09949426530000238 ) ) ;
#12327 = DIRECTION ( 'NONE',  ( 0.000000000000000000, 0.000000000000000000, -1.000000000000000000 ) ) ;
#12328 = CYLINDRICAL_SURFACE ( 'NONE', #486, 26.80000000000002203 ) ;
#12329 = CARTESIAN_POINT ( 'NONE',  ( 4.638687372183706970, -17.80543024189401535, -28.79488058871456957 ) ) ;
#12330 = FACE_OUTER_BOUND ( 'NONE', #30461, .T. ) ;
#12331 = DIRECTION ( 'NONE',  ( 5.962915006522622422E-16, 0.4383711467890810676, 0.8987940462991651502 ) ) ;
#12332 = EDGE_CURVE ( 'NONE', #23086, #7730, #28686, .T. ) ;
#12333 = FACE_OUTER_BOUND ( 'NONE', #2804, .T. ) ;
#12334 = CARTESIAN_POINT ( 'NONE',  ( -10.69999999999999929, -25.55727021120000231, -31.05966627990000006 ) ) ;
#12335 = CARTESIAN_POINT ( 'NONE',  ( 18.50497803210000214, 20.74625852780000201, 229.0000000010000178 ) ) ;
#12336 = CARTESIAN_POINT ( 'NONE',  ( 5.114250173790000353, 17.43050733020000109, 230.6999999999999886 ) ) ;
#12337 = ORIENTED_EDGE ( 'NONE', *, *, #6445, .F. ) ;
#12338 = CARTESIAN_POINT ( 'NONE',  ( 5.655353257550568280, 0.6391371982588460732, -54.21771407622500050 ) ) ;
#12339 = CARTESIAN_POINT ( 'NONE',  ( -28.49530731802708416, -0.5184832703812605192, 8.000000000000007105 ) ) ;
#12340 = CARTESIAN_POINT ( 'NONE',  ( 2.457213513335546828, -4.104727644910624029, -68.10000000002501963 ) ) ;
#12341 = ADVANCED_FACE ( 'NONE', ( #8826 ), #6472, .T. ) ;
#12342 = CARTESIAN_POINT ( 'NONE',  ( -6.982632971260602339, 5.672256964453205264, -40.24571374340602148 ) ) ;
#12343 = AXIS2_PLACEMENT_3D ( 'NONE', #3126, #5801, #24852 ) ;
#12344 = VERTEX_POINT ( 'NONE', #11357 ) ;
#12345 = CARTESIAN_POINT ( 'NONE',  ( -3.373344672752120132, 1.082959996301855021, -88.52261276241732446 ) ) ;
#12346 =( NAMED_UNIT ( * ) SI_UNIT ( $, .STERADIAN. ) SOLID_ANGLE_UNIT ( ) );
#12347 = ORIENTED_EDGE ( 'NONE', *, *, #224, .T. ) ;
#12348 = CARTESIAN_POINT ( 'NONE',  ( 3.693725231361444816, 2.029077553930086708, -38.46881641890171011 ) ) ;
#12349 = CARTESIAN_POINT ( 'NONE',  ( 1.157672466085042151, -27.77645868488912484, 4.099089508000003157 ) ) ;
#12350 = ORIENTED_EDGE ( 'NONE', *, *, #15638, .F. ) ;
#12351 = CARTESIAN_POINT ( 'NONE',  ( 2.193772516446764076, 5.694542648089183423, -26.69462237479999800 ) ) ;
#12352 = EDGE_CURVE ( 'NONE', #22757, #20880, #23006, .T. ) ;
#12353 = DIRECTION ( 'NONE',  ( 0.000000000000000000, 0.9396926207858125046, 0.3420201433259318358 ) ) ;
#12354 = CARTESIAN_POINT ( 'NONE',  ( 2.994727039187461415, -3.426347720743794234, -64.49605006312501132 ) ) ;
#12355 = DIRECTION ( 'NONE',  ( -0.7071067811865475727, 0.6644630243886071597, 0.2418447626481610435 ) ) ;
#12356 =( NAMED_UNIT ( * ) SI_UNIT ( $, .STERADIAN. ) SOLID_ANGLE_UNIT ( ) );
#12357 = CARTESIAN_POINT ( 'NONE',  ( -15.75517453283980096, 10.73903380419648812, -1.400000000000001910 ) ) ;
#12358 = CARTESIAN_POINT ( 'NONE',  ( -7.999999999683975460, -16.77380904890792834, -33.17160705600048942 ) ) ;
#12359 = CARTESIAN_POINT ( 'NONE',  ( -17.39952085737127518, -22.00021057524676849, -29.68220823416547205 ) ) ;
#12360 = EDGE_LOOP ( 'NONE', ( #12416, #24936, #23483, #25309 ) ) ;
#12361 = CARTESIAN_POINT ( 'NONE',  ( 3.147559148823465769, 1.548267634410576132, 227.6488953029178219 ) ) ;
#12362 = DIRECTION ( 'NONE',  ( 0.000000000000000000, 0.000000000000000000, 1.000000000000000000 ) ) ;
#12363 = CARTESIAN_POINT ( 'NONE',  ( -2.808177005839999740, -11.72927066510000138, 231.9999989789999972 ) ) ;
#12364 = LINE ( 'NONE', #21973, #19290 ) ;
#12365 = CARTESIAN_POINT ( 'NONE',  ( -24.36375527493646942, -13.38839014155000129, 4.854229180514668229 ) ) ;
#12366 = CARTESIAN_POINT ( 'NONE',  ( -2.373469614669185379, -26.70001233586149070, 210.0000000000000568 ) ) ;
#12367 = CARTESIAN_POINT ( 'NONE',  ( -17.32140263436448890, -8.004506215797992041, 0.000000000000000000 ) ) ;
#12368 = CARTESIAN_POINT ( 'NONE',  ( -27.16361495901510636, -7.646758255380050606, -0.6577119969999878357 ) ) ;
#12369 = CARTESIAN_POINT ( 'NONE',  ( 0.8360625678816901996, -27.48733645973267770, 4.281332030192536386 ) ) ;
#12370 = CARTESIAN_POINT ( 'NONE',  ( -28.35945636601969611, -7.983396444588293228, 8.000000000000007105 ) ) ;
#12371 = CARTESIAN_POINT ( 'NONE',  ( 17.93011078763067090, 11.79183908526299085, 0.000000000000000000 ) ) ;
#12372 = CARTESIAN_POINT ( 'NONE',  ( -16.83342759559999635, 11.00000000000000355, -0.6999999999999992895 ) ) ;
#12373 = CARTESIAN_POINT ( 'NONE',  ( -0.6731456005949999488, -4.118494162357343669, -70.37733883405731206 ) ) ;
#12374 = EDGE_CURVE ( 'NONE', #22213, #18513, #14036, .T. ) ;
#12375 = ORIENTED_EDGE ( 'NONE', *, *, #27306, .F. ) ;
#12376 = CARTESIAN_POINT ( 'NONE',  ( 7.999999999994048316, -116.8591659214849159, 11.34031266730467813 ) ) ;
#12377 = EDGE_CURVE ( 'NONE', #26900, #24004, #13300, .T. ) ;
#12378 = FILL_AREA_STYLE ('',( #30691 ) ) ;
#12379 = EDGE_CURVE ( 'NONE', #6771, #16061, #3150, .T. ) ;
#12381 = DIRECTION ( 'NONE',  ( 1.000000000000000000, 0.000000000000000000, 0.000000000000000000 ) ) ;
#12380 = B_SPLINE_CURVE_WITH_KNOTS ( 'NONE', 5,
 ( #21559, #7233, #9592, #13855, #23463, #1897, #13328, #6557, #20411, #30493, #3892, #22770 ),
 .UNSPECIFIED., .F., .F.,
 ( 6, 3, 3, 6 ),
 ( 1.224410036190000106, 1.456395025189999970, 2.184590866520000230, 2.448622045610000075 ),
 .UNSPECIFIED. ) ;
#12382 = CARTESIAN_POINT ( 'NONE',  ( 0.8945918243927786229, -4.819150861182647461, -59.14125695792499471 ) ) ;
#12383 = VERTEX_POINT ( 'NONE', #4115 ) ;
#12384 = ORIENTED_EDGE ( 'NONE', *, *, #25559, .T. ) ;
#12385 = CARTESIAN_POINT ( 'NONE',  ( -9.000000000000000000, -130.0000000000000000, -42.39999999999999858 ) ) ;
#12386 = ORIENTED_EDGE ( 'NONE', *, *, #22930, .F. ) ;
#12387 = EDGE_LOOP ( 'NONE', ( #21986, #17445, #13825, #6172 ) ) ;
#12388 = CARTESIAN_POINT ( 'NONE',  ( 28.50000000000000000, 1.065814103639999922E-14, 229.0000000000000000 ) ) ;
#12389 = DIRECTION ( 'NONE',  ( 0.000000000000000000, 0.000000000000000000, -1.000000000000000000 ) ) ;
#12390 = DIRECTION ( 'NONE',  ( 0.000000000000000000, 0.000000000000000000, -1.000000000000000000 ) ) ;
#12391 = B_SPLINE_SURFACE_WITH_KNOTS ( 'NONE', 5, 1, ( 
 ( #19409, #1097 ),
 ( #5813, #15257 ),
 ( #24704, #3142 ),
 ( #22505, #28998 ),
 ( #5503, #28837 ),
 ( #27517, #8012 ) ),
 .UNSPECIFIED., .F., .F., .F.,
 ( 6, 6 ),
 ( 2, 2 ),
 ( 0.000000000000000000, 7.118283443510000197 ),
 ( -0.7000000000080000007, 0.0003775010496399999857 ),
 .UNSPECIFIED. ) ;
#12392 = CARTESIAN_POINT ( 'NONE',  ( 7.780396774639999791, 9.519126025529999424, 232.6627648150000027 ) ) ;
#12393 = FACE_OUTER_BOUND ( 'NONE', #17137, .T. ) ;
#12394 = CARTESIAN_POINT ( 'NONE',  ( 0.5074138422395748638, -6.503547975687064664, -8.793384211800002959 ) ) ;
#12395 = CARTESIAN_POINT ( 'NONE',  ( 8.699999999949442397, -116.5561065468441626, 18.74526241745003574 ) ) ;
#12396 = ORIENTED_EDGE ( 'NONE', *, *, #28404, .F. ) ;
#12397 = CARTESIAN_POINT ( 'NONE',  ( 2.805604715719960840, -3.444923010881604242, -44.10000000002499121 ) ) ;
#12398 = LINE ( 'NONE', #5620, #11282 ) ;
#12399 = CARTESIAN_POINT ( 'NONE',  ( 3.736517203680826515, 4.566916950137848374, -21.25622222230000347 ) ) ;
#12400 = CARTESIAN_POINT ( 'NONE',  ( 2.553512956640000223E-15, 3.378317624991660661, -69.77707803651591689 ) ) ;
#12401 = CARTESIAN_POINT ( 'NONE',  ( -8.699999999695283037, -25.56176843068484317, -31.06196806030030544 ) ) ;
#12402 = DIRECTION ( 'NONE',  ( 0.3633921898465273803, -0.9316362575375355393, -1.040834085586083783E-14 ) ) ;
#12403 = CARTESIAN_POINT ( 'NONE',  ( -16.06988964647317886, -8.208161364834239748, 0.000000000000000000 ) ) ;
#12404 = CARTESIAN_POINT ( 'NONE',  ( -1.760169390438194759, -5.172221906152406845, -46.19520033282500293 ) ) ;
#12405 = CARTESIAN_POINT ( 'NONE',  ( 4.000000000000000000, -29.96004123392021157, -79.78289277550334191 ) ) ;
#12406 = CARTESIAN_POINT ( 'NONE',  ( -15.73360964030186970, 11.02001161816959396, -1.000005633855494125E-09 ) ) ;
#12407 = CARTESIAN_POINT ( 'NONE',  ( 8.699999999957087837, -117.0726643325088645, 17.59013759100812280 ) ) ;
#12408 = CARTESIAN_POINT ( 'NONE',  ( -25.98395164609999952, 9.085482504939999870, 230.0000000000000000 ) ) ;
#12409 = CARTESIAN_POINT ( 'NONE',  ( -1.630907769230000026, -5.558498091359999727, 229.6412452697800006 ) ) ;
#12410 = EDGE_LOOP ( 'NONE', ( #15168, #1628, #30676, #25343 ) ) ;
#12411 = CARTESIAN_POINT ( 'NONE',  ( -3.052438874386679046, 3.509528713898351970, -29.08728588869999498 ) ) ;
#12412 = EDGE_CURVE ( 'NONE', #10989, #28017, #21557, .T. ) ;
#12413 = ORIENTED_EDGE ( 'NONE', *, *, #18793, .F. ) ;
#12414 = FACE_OUTER_BOUND ( 'NONE', #29312, .T. ) ;
#12415 = CARTESIAN_POINT ( 'NONE',  ( -2.571638601809290936, 3.775240214263654526, -48.05391720702499470 ) ) ;
#12416 = ORIENTED_EDGE ( 'NONE', *, *, #16777, .F. ) ;
#12417 = ORIENTED_EDGE ( 'NONE', *, *, #23946, .T. ) ;
#12418 = CARTESIAN_POINT ( 'NONE',  ( -32.04194418040925285, -22.56290441860536689, -0.05106179917585312866 ) ) ;
#12419 = B_SPLINE_CURVE_WITH_KNOTS ( 'NONE', 3,
 ( #6996, #18787, #1658, #11868 ),
 .UNSPECIFIED., .F., .F.,
 ( 4, 4 ),
 ( 0.000000000000000000, 1.000000000000000000 ),
 .UNSPECIFIED. ) ;
#12420 = ORIENTED_EDGE ( 'NONE', *, *, #28962, .T. ) ;
#12421 = AXIS2_PLACEMENT_3D ( 'NONE', #23243, #20405, #18511 ) ;
#12422 = CYLINDRICAL_SURFACE ( 'NONE', #27043, 1.100000000000002309 ) ;
#12423 = ORIENTED_EDGE ( 'NONE', *, *, #22411, .F. ) ;
#12424 = DIRECTION ( 'NONE',  ( 1.000000000000000000, 0.000000000000000000, 0.000000000000000000 ) ) ;
#12425 = LINE ( 'NONE', #26908, #19300 ) ;
#12426 = CARTESIAN_POINT ( 'NONE',  ( 9.999999999969219289, -29.99999999999982236, -28.05272263597640503 ) ) ;
#12427 = CARTESIAN_POINT ( 'NONE',  ( 0.5710670605986443160, 4.210710561773831628, -35.70000000000000284 ) ) ;
#12428 = DIRECTION ( 'NONE',  ( 0.000000000000000000, 0.000000000000000000, 1.000000000000000000 ) ) ;
#12429 = CARTESIAN_POINT ( 'NONE',  ( -24.70074544867652122, 14.21822122508601716, 6.002806299999996043 ) ) ;
#12430 = FACE_OUTER_BOUND ( 'NONE', #26665, .T. ) ;
#12431 = DIRECTION ( 'NONE',  ( -1.000000000000000000, -0.000000000000000000, 0.000000000000000000 ) ) ;
#12432 = CARTESIAN_POINT ( 'NONE',  ( 5.067327387632984959, 4.072231104569050686, -8.354586407999999409 ) ) ;
#12433 = CARTESIAN_POINT ( 'NONE',  ( -1.458225024262878255, -5.692467481908745519, -26.54882611460000419 ) ) ;
#12434 = CARTESIAN_POINT ( 'NONE',  ( 0.1441963505053185379, -27.80021098764100174, 226.1000014189999661 ) ) ;
#12435 = CARTESIAN_POINT ( 'NONE',  ( 24.39135169777336287, -14.74223403354865347, 5.310643619999999565 ) ) ;
#12436 = CARTESIAN_POINT ( 'NONE',  ( 24.92639507930385889, 13.81781707913292934, 5.506973475999988210 ) ) ;
#12437 = CARTESIAN_POINT ( 'NONE',  ( 1.087695520339999833, -27.77888045939999984, 225.2081038119999903 ) ) ;
#12438 = CARTESIAN_POINT ( 'NONE',  ( 4.310466091822805268, 1.786666325167808544, -11.49261350019999739 ) ) ;
#12439 = ADVANCED_FACE ( 'NONE', ( #11196 ), #20797, .T. ) ;
#12440 = AXIS2_PLACEMENT_3D ( 'NONE', #9709, #445, #16786 ) ;
#12441 = CARTESIAN_POINT ( 'NONE',  ( 16.15160659333890791, 10.55214128798958129, -1.400000000000001910 ) ) ;
#12442 = CARTESIAN_POINT ( 'NONE',  ( -24.36724936496760918, -13.38201651699120021, 4.895818166000015736 ) ) ;
#12443 = CARTESIAN_POINT ( 'NONE',  ( 16.06413493398061476, 11.12395421528300865, -4.336808689942017736E-16 ) ) ;
#12444 = VERTEX_POINT ( 'NONE', #1767 ) ;
#12445 = FACE_OUTER_BOUND ( 'NONE', #5796, .T. ) ;
#12446 = CARTESIAN_POINT ( 'NONE',  ( 13.62135916440115935, 20.99999999989658761, -68.61085694196312090 ) ) ;
#12447 = ORIENTED_EDGE ( 'NONE', *, *, #10118, .T. ) ;
#12448 = CARTESIAN_POINT ( 'NONE',  ( -23.20948082139999968, -13.40000000000000036, 223.8999999999999773 ) ) ;
#12449 = CARTESIAN_POINT ( 'NONE',  ( 14.94562240850000023, -8.628859120750000500, 225.0000000000000000 ) ) ;
#12450 = ORIENTED_EDGE ( 'NONE', *, *, #28078, .F. ) ;
#12451 = CARTESIAN_POINT ( 'NONE',  ( -4.892650201704735302, -0.5748897526526646207, -44.10000000002499121 ) ) ;
#12452 = ORIENTED_EDGE ( 'NONE', *, *, #20784, .T. ) ;
#12453 = B_SPLINE_SURFACE_WITH_KNOTS ( 'NONE', 5, 1, ( 
 ( #19613, #10018 ),
 ( #8099, #3382 ),
 ( #22443, #889 ),
 ( #29670, #17692 ),
 ( #27307, #5749 ),
 ( #29816, #5897 ),
 ( #15502, #1513 ),
 ( #30620, #11258 ),
 ( #4020, #25584 ) ),
 .UNSPECIFIED., .F., .F., .F.,
 ( 6, 3, 6 ),
 ( 2, 2 ),
 ( 0.000000000000000000, 55.31395511720000258, 94.75474465359999954 ),
 ( -3.500000000000000000, 3.500000000000000000 ),
 .UNSPECIFIED. ) ;
#12454 = VERTEX_POINT ( 'NONE', #17797 ) ;
#12455 = VECTOR ( 'NONE', #8461, 1000.000000000000000 ) ;
#12456 = APPLICATION_PROTOCOL_DEFINITION ( 'draft international standard', 'automotive_design', 1998, #1543 ) ;
#12457 = ORIENTED_EDGE ( 'NONE', *, *, #3090, .F. ) ;
#12458 = CARTESIAN_POINT ( 'NONE',  ( -17.49999999969999465, -24.07621958799680328, -29.18059818862752053 ) ) ;
#12459 = CARTESIAN_POINT ( 'NONE',  ( -10.69999999999999929, -82.23832021929999314, -29.25398675779999991 ) ) ;
#12460 = CARTESIAN_POINT ( 'NONE',  ( 18.26377084491840463, -8.836022547968246599, -4.336808689942018722E-16 ) ) ;
#12461 = ORIENTED_EDGE ( 'NONE', *, *, #643, .F. ) ;
#12462 = CARTESIAN_POINT ( 'NONE',  ( -24.63375100851393640, 12.88633854783081922, 5.901400367999992902 ) ) ;
#12463 = FACE_OUTER_BOUND ( 'NONE', #12533, .T. ) ;
#12464 = CONICAL_SURFACE ( 'NONE', #14974, 2.500000000105231823, 0.7853981633974348453 ) ;
#12465 = CARTESIAN_POINT ( 'NONE',  ( -17.44828348017973596, -31.99970846322542428, -27.51010410072800738 ) ) ;
#12466 = CARTESIAN_POINT ( 'NONE',  ( 13.99999999979999821, 20.99999999999999645, -63.10000000000000142 ) ) ;
#12467 = ORIENTED_EDGE ( 'NONE', *, *, #28647, .T. ) ;
#12468 = EDGE_CURVE ( 'NONE', #11841, #5428, #18931, .T. ) ;
#12469 = CARTESIAN_POINT ( 'NONE',  ( -10.69999999993204831, -25.59800645591167267, -12.29403537759453258 ) ) ;
#12470 = CARTESIAN_POINT ( 'NONE',  ( -2.970579505556664834, -5.081274235795743444, -14.68182079290001241 ) ) ;
#12471 = CARTESIAN_POINT ( 'NONE',  ( -7.534632680830988249, -6.582071621271182060, -34.26887834115397169 ) ) ;
#12472 = CARTESIAN_POINT ( 'NONE',  ( 1.019043873895764341, -27.48159911132826494, 5.420262664917122386 ) ) ;
#12473 = CARTESIAN_POINT ( 'NONE',  ( 4.023925869015616996, -19.44723706322411161, -27.99411789782213944 ) ) ;
#12474 = CARTESIAN_POINT ( 'NONE',  ( -8.881784197000000993E-16, 2.220446049249999755E-16, 230.8412452700000017 ) ) ;
#12475 = CARTESIAN_POINT ( 'NONE',  ( 18.28658402242479397, 10.97998838177520931, -1.452769935612311825 ) ) ;
#12476 = ADVANCED_FACE ( 'NONE', ( #16537 ), #4430, .T. ) ;
#12477 = TOROIDAL_SURFACE ( 'NONE', #27547, 24.50000000000000000, 4.000000000000000000 ) ;
#12478 = DIRECTION ( 'NONE',  ( -1.000000000000000000, 5.687698019339887572E-16, -6.771501495046482653E-12 ) ) ;
#12479 = DIRECTION ( 'NONE',  ( -0.5532886644841250590, -0.8329895880221872551, 0.000000000000000000 ) ) ;
#12480 = CARTESIAN_POINT ( 'NONE',  ( 27.09307779329999732, 4.575104118570000544, 229.9751247039999953 ) ) ;
#12481 = CARTESIAN_POINT ( 'NONE',  ( -8.999999999710000864, 21.70000000000000284, -57.60000000000000142 ) ) ;
#12482 = ORIENTED_EDGE ( 'NONE', *, *, #20624, .F. ) ;
#12483 = CARTESIAN_POINT ( 'NONE',  ( 2.964344385318878228, 3.936232207889206247, -53.87619010302499589 ) ) ;
#12484 = AXIS2_PLACEMENT_3D ( 'NONE', #31000, #9122, #21411 ) ;
#12485 = CARTESIAN_POINT ( 'NONE',  ( -12.31092893605833538, -24.78820930377925791, -23.90347526215919416 ) ) ;
#12486 = CARTESIAN_POINT ( 'NONE',  ( -18.44984504927483471, 20.68447211616248893, 0.5514271140000248650 ) ) ;
#12487 = VECTOR ( 'NONE', #14539, 1000.000000000000000 ) ;
#12488 = CARTESIAN_POINT ( 'NONE',  ( -4.605309145015588079, 0.8848923369832152330, -68.10000000002499121 ) ) ;
#12489 = ADVANCED_FACE ( 'NONE', ( #30709 ), #10142, .T. ) ;
#12490 = ORIENTED_EDGE ( 'NONE', *, *, #30591, .T. ) ;
#12491 = EDGE_CURVE ( 'NONE', #10036, #4792, #20521, .T. ) ;
#12492 = CARTESIAN_POINT ( 'NONE',  ( 3.521042344302120153, 0.5632927345595589719, -88.52261276242234089 ) ) ;
#12493 = ORIENTED_EDGE ( 'NONE', *, *, #6721, .T. ) ;
#12494 = CARTESIAN_POINT ( 'NONE',  ( 24.34246741410084880, 14.82285105323827779, 6.099998581000033226 ) ) ;
#12495 = CARTESIAN_POINT ( 'NONE',  ( -8.903108651239966420, -22.82508830966961000, 40.00000000000000000 ) ) ;
#12496 = ORIENTED_EDGE ( 'NONE', *, *, #27071, .T. ) ;
#12497 = CARTESIAN_POINT ( 'NONE',  ( 4.801822465207213675, -2.670409256638542672, -27.93037294500000201 ) ) ;
#12498 = DIRECTION ( 'NONE',  ( 0.3633921898465276024, -0.9316362575375355393, 0.000000000000000000 ) ) ;
#12499 = CIRCLE ( 'NONE', #28091, 10.00000000000000178 ) ;
#12500 = PRODUCT_RELATED_PRODUCT_CATEGORY ( 'part', '', ( #20959 ) ) ;
#12501 = CARTESIAN_POINT ( 'NONE',  ( 3.874396413951479268, -2.399869827310083803, -49.33324460762499797 ) ) ;
#12502 = CARTESIAN_POINT ( 'NONE',  ( 8.000000000875953532, -24.10104989775918938, -29.26619909572536926 ) ) ;
#12503 = CARTESIAN_POINT ( 'NONE',  ( 10.32522729140000095, -24.79836099970000163, -1.399999999999998579 ) ) ;
#12504 = UNCERTAINTY_MEASURE_WITH_UNIT (LENGTH_MEASURE( 1.000000000000000082E-05 ), #5904, 'distance_accuracy_value', 'NONE');
#12505 = CARTESIAN_POINT ( 'NONE',  ( 8.700000000284758173, -13.44093381510830909, -35.27466467713743015 ) ) ;
#12507 = EDGE_CURVE ( 'NONE', #24264, #3826, #159, .T. ) ;
#12506 = CIRCLE ( 'NONE', #7962, 2.999999999999999112 ) ;
#12508 = LINE ( 'NONE', #7175, #23580 ) ;
#12509 = ORIENTED_EDGE ( 'NONE', *, *, #9865, .T. ) ;
#12510 = CARTESIAN_POINT ( 'NONE',  ( 26.80000000000000071, -1.776356839399999804E-15, 143.2171415880000040 ) ) ;
#12511 = CARTESIAN_POINT ( 'NONE',  ( -24.98081131316241255, -13.71897606304888662, 5.104178996000019453 ) ) ;
#12512 = CARTESIAN_POINT ( 'NONE',  ( -23.23955040174346465, -15.25661106733265981, 5.208368890000008911 ) ) ;
#12513 = CARTESIAN_POINT ( 'NONE',  ( -3.823204249305973690, -1.799205776751950703, -96.01609449157885479 ) ) ;
#12514 = CARTESIAN_POINT ( 'NONE',  ( -4.885731407867048404, -11.07235429843764507, 232.0000000000045191 ) ) ;
#12515 = CARTESIAN_POINT ( 'NONE',  ( -3.918707624292968372, -26.51317744985242442, 209.7461278024016735 ) ) ;
#12516 = CARTESIAN_POINT ( 'NONE',  ( 2.418887229898759816, -3.215241712391042839, -0.6999999999999992895 ) ) ;
#12517 = DIRECTION ( 'NONE',  ( 0.000000000000000000, 0.000000000000000000, 1.000000000000000000 ) ) ;
#12518 = LINE ( 'NONE', #19922, #17760 ) ;
#12519 = SURFACE_STYLE_FILL_AREA ( #29354 ) ;
#12520 = DIRECTION ( 'NONE',  ( -1.000000000000000000, 0.000000000000000000, -6.771000000000000128E-12 ) ) ;
#12521 = EDGE_CURVE ( 'NONE', #4471, #18763, #11413, .T. ) ;
#12522 = CARTESIAN_POINT ( 'NONE',  ( -24.77829191970622702, -10.21159038398081087, 93.21714158839905906 ) ) ;
#12523 = CARTESIAN_POINT ( 'NONE',  ( -1.278635117706684587, -3.697671176787224567, -68.10000000002499121 ) ) ;
#12524 = ADVANCED_BREP_SHAPE_REPRESENTATION ( '', ( #836, #17722 ), #14795 ) ;
#12525 = ORIENTED_EDGE ( 'NONE', *, *, #12089, .F. ) ;
#12526 = ADVANCED_FACE ( 'NONE', ( #19057 ), #1936, .T. ) ;
#12527 = CARTESIAN_POINT ( 'NONE',  ( -9.130012207994363749, 21.69999999998125162, -52.40811918958280557 ) ) ;
#12528 =( LENGTH_UNIT ( ) NAMED_UNIT ( * ) SI_UNIT ( .MILLI., .METRE. ) );
#12529 = TOROIDAL_SURFACE ( 'NONE', #30122, 29.80000000000000071, 3.000000000000000000 ) ;
#12530 = CARTESIAN_POINT ( 'NONE',  ( 24.39498713390000262, -13.33204241790000033, 225.9012973829999851 ) ) ;
#12531 = ADVANCED_FACE ( 'NONE', ( #28653 ), #4897, .F. ) ;
#12532 = CARTESIAN_POINT ( 'NONE',  ( -5.182433330280534989, 2.850054831770709285, -60.61908057272500372 ) ) ;
#12533 = EDGE_LOOP ( 'NONE', ( #10960, #16986, #13501, #22571 ) ) ;
#12534 = PRODUCT_RELATED_PRODUCT_CATEGORY ( 'part', '', ( #10831 ) ) ;
#12535 = ORIENTED_EDGE ( 'NONE', *, *, #4704, .F. ) ;
#12536 = DIRECTION ( 'NONE',  ( 2.764840495839172514E-12, 0.9128796883888952163, -0.4082287037029530552 ) ) ;
#12537 = ORIENTED_EDGE ( 'NONE', *, *, #17662, .F. ) ;
#12538 = ORIENTED_EDGE ( 'NONE', *, *, #4200, .T. ) ;
#12539 = CARTESIAN_POINT ( 'NONE',  ( -4.084346732781016343, 0.2146938847797513761, -40.92168819672095736 ) ) ;
#12540 = CARTESIAN_POINT ( 'NONE',  ( -24.88589369081283920, 13.89120818323882922, 3.904029272000009154 ) ) ;
#12541 = CARTESIAN_POINT ( 'NONE',  ( -3.552713678799999608E-15, 0.000000000000000000, 143.2171415880000040 ) ) ;
#12542 = UNCERTAINTY_MEASURE_WITH_UNIT (LENGTH_MEASURE( 1.000000000000000082E-05 ), #21407, 'distance_accuracy_value', 'NONE');
#12543 = CARTESIAN_POINT ( 'NONE',  ( 18.11354342366337988, 11.57790908577752376, -1.400000000000001910 ) ) ;
#12544 = ADVANCED_FACE ( 'NONE', ( #23482 ), #1918, .F. ) ;
#12545 = DIRECTION ( 'NONE',  ( 1.000000000000000000, -1.224606353819999829E-16, 0.000000000000000000 ) ) ;
#12546 = CARTESIAN_POINT ( 'NONE',  ( -3.925562765917044228, -3.929887376319241898, -8.813991631000002158 ) ) ;
#12547 = CARTESIAN_POINT ( 'NONE',  ( 28.50000000000000000, 1.065814103639999922E-14, 229.0000000000000000 ) ) ;
#12548 = VERTEX_POINT ( 'NONE', #24403 ) ;
#12549 = CARTESIAN_POINT ( 'NONE',  ( 2.604942178515098128, -3.963434524254012548, -44.10000000002500542 ) ) ;
#12550 = CARTESIAN_POINT ( 'NONE',  ( 17.18658402238548533, 9.900182044515950963, -0.6999999999999784173 ) ) ;
#12551 = EDGE_CURVE ( 'NONE', #2707, #27598, #15109, .T. ) ;
#12552 = CARTESIAN_POINT ( 'NONE',  ( -3.679974273075529823, -2.251605409995534490, -21.90799200640000777 ) ) ;
#12553 = CARTESIAN_POINT ( 'NONE',  ( -12.40457278470412206, -23.36520658321533617, -32.07470739609649968 ) ) ;
#12554 = CARTESIAN_POINT ( 'NONE',  ( 0.6425564541914388084, -27.49266737062501065, 225.9130852755266403 ) ) ;
#12555 = FILL_AREA_STYLE ('',( #7979 ) ) ;
#12556 = PLANE ( 'NONE',  #15673 ) ;
#12557 = CARTESIAN_POINT ( 'NONE',  ( -2.769456955792640951, 4.065643307668772799, -47.30391720702499470 ) ) ;
#12558 = EDGE_CURVE ( 'NONE', #24996, #23898, #24568, .T. ) ;
#12559 = B_SPLINE_CURVE_WITH_KNOTS ( 'NONE', 5,
 ( #19401, #11852, #531, #23975, #5075, #7589, #21927, #7435, #2717 ),
 .UNSPECIFIED., .F., .F.,
 ( 6, 3, 6 ),
 ( 0.000000000000000000, 1.646696146380000059, 2.782752057460000206 ),
 .UNSPECIFIED. ) ;
#12560 = CARTESIAN_POINT ( 'NONE',  ( 4.560781034842324999, -19.82596349573488581, -31.14720649596092628 ) ) ;
#12561 = CARTESIAN_POINT ( 'NONE',  ( -26.93395386830000149, 3.298349104069999855E-15, 142.2432411360000231 ) ) ;
#12562 = CARTESIAN_POINT ( 'NONE',  ( -17.87606967260930446, 20.00000012015441087, 230.7000000000000171 ) ) ;
#12563 = CARTESIAN_POINT ( 'NONE',  ( -18.13790635940000229, 20.33475721459999974, 229.9172021029999939 ) ) ;
#12564 = CARTESIAN_POINT ( 'NONE',  ( 9.000000000000000000, 21.70000000000000284, -56.10000000020000499 ) ) ;
#12565 = ORIENTED_EDGE ( 'NONE', *, *, #6373, .T. ) ;
#12566 = CARTESIAN_POINT ( 'NONE',  ( -4.781258647701263520, -0.007971864669480827059, -29.10606466010000304 ) ) ;
#12567 = ORIENTED_EDGE ( 'NONE', *, *, #11187, .T. ) ;
#12568 = CARTESIAN_POINT ( 'NONE',  ( 12.77819780750000156, 20.99999999999999645, -56.09999999999999432 ) ) ;
#12569 = CARTESIAN_POINT ( 'NONE',  ( 5.943504367937093136, -0.4395870339238064362, -49.12442242802499948 ) ) ;
#12570 = ORIENTED_EDGE ( 'NONE', *, *, #22587, .F. ) ;
#12571 = EDGE_LOOP ( 'NONE', ( #21763, #9959, #12324, #17215 ) ) ;
#12572 = DIRECTION ( 'NONE',  ( -1.570874681152831116E-17, 5.324211852125039574E-17, 1.000000000000000000 ) ) ;
#12573 = ORIENTED_EDGE ( 'NONE', *, *, #10851, .F. ) ;
#12574 = VERTEX_POINT ( 'NONE', #5352 ) ;
#12575 = CIRCLE ( 'NONE', #16669, 2.999999999999999556 ) ;
#12576 = CARTESIAN_POINT ( 'NONE',  ( 24.55806919409999978, -14.46257963250000067, 226.0798541909999813 ) ) ;
#12577 = CARTESIAN_POINT ( 'NONE',  ( 24.98081130624543889, 13.71897605842228529, 4.895818164000031558 ) ) ;
#12578 = CARTESIAN_POINT ( 'NONE',  ( 27.75695160380879045, 2.618790587931635994, 1.000000000000000888 ) ) ;
#12579 = CARTESIAN_POINT ( 'NONE',  ( -27.76135143630000002, 3.399672735959999724E-15, 87.66141409829998565 ) ) ;
#12580 = DIRECTION ( 'NONE',  ( 0.8090169943751909232, 0.5877852522921378498, 0.000000000000000000 ) ) ;
#12581 = ADVANCED_FACE ( 'NONE', ( #343 ), #499, .F. ) ;
#12582 = CARTESIAN_POINT ( 'NONE',  ( -5.076643603551637796, -0.7187466731379940077, -0.6999999999999992895 ) ) ;
#12583 = CARTESIAN_POINT ( 'NONE',  ( 3.436082050571401147, -2.282315740991585962, 0.9787452697999995399 ) ) ;
#12584 = LINE ( 'NONE', #19526, #30601 ) ;
#12585 = ORIENTED_EDGE ( 'NONE', *, *, #7104, .T. ) ;
#12586 = CARTESIAN_POINT ( 'NONE',  ( -0.8919388126321509125, 6.008950160842678301, -10.86772091660000150 ) ) ;
#12587 = CARTESIAN_POINT ( 'NONE',  ( 5.771960588457029750, -1.304678385547908492, -31.78377053309999312 ) ) ;
#12588 = CARTESIAN_POINT ( 'NONE',  ( -6.585786437629999490, -16.41511111490214603, -74.85294138696069410 ) ) ;
#12589 = EDGE_CURVE ( 'NONE', #25831, #27584, #9171, .T. ) ;
#12590 = EDGE_CURVE ( 'NONE', #27980, #21635, #10388, .T. ) ;
#12591 = LINE ( 'NONE', #21902, #17678 ) ;
#12592 = CARTESIAN_POINT ( 'NONE',  ( 20.15233751852803579, 20.00000015395470498, 0.3716988990000169579 ) ) ;
#12593 = CARTESIAN_POINT ( 'NONE',  ( -23.25354871331287043, -14.68148953535444790, 225.2179249493744635 ) ) ;
#12594 = CARTESIAN_POINT ( 'NONE',  ( 0.1059454459490000028, -28.50005195860000029, 226.0959520840000039 ) ) ;
#12595 = CARTESIAN_POINT ( 'NONE',  ( -0.7188231668698794596, 4.425078454789642457, -34.84333403589999278 ) ) ;
#12596 = LINE ( 'NONE', #22204, #12705 ) ;
#12597 = APPLICATION_CONTEXT ( 'automotive_design' ) ;
#12598 = CARTESIAN_POINT ( 'NONE',  ( -5.414213562369999622, -31.28896728272270877, -80.26658230080884948 ) ) ;
#12599 = CARTESIAN_POINT ( 'NONE',  ( 1.645798001284060064, -3.500000000000228706, 230.6318310357691814 ) ) ;
#12600 = VERTEX_POINT ( 'NONE', #19679 ) ;
#12601 = CARTESIAN_POINT ( 'NONE',  ( -15.73360964030186970, 11.02001161816959396, -0.6999999989999727834 ) ) ;
#12602 = CARTESIAN_POINT ( 'NONE',  ( -3.889411361886101481, -19.79584274981791125, -27.82409154391096351 ) ) ;
#12603 = VERTEX_POINT ( 'NONE', #5502 ) ;
#12604 = CARTESIAN_POINT ( 'NONE',  ( 6.999999999942878581, -114.8328013981175673, 22.59891173924912877 ) ) ;
#12605 = CARTESIAN_POINT ( 'NONE',  ( 0.000000000000000000, 0.000000000000000000, 40.00000000000000000 ) ) ;
#12606 = ORIENTED_EDGE ( 'NONE', *, *, #3059, .T. ) ;
#12607 = CARTESIAN_POINT ( 'NONE',  ( -5.066079940368577006, -16.24646118435289566, -109.8342699011357126 ) ) ;
#12608 = ORIENTED_EDGE ( 'NONE', *, *, #14825, .F. ) ;
#12609 = ORIENTED_EDGE ( 'NONE', *, *, #21227, .T. ) ;
#12610 = EDGE_LOOP ( 'NONE', ( #28821, #11826, #8780, #6025, #6143, #23972, #5344, #19319 ) ) ;
#12611 = CARTESIAN_POINT ( 'NONE',  ( 25.45460661299999927, 14.13620899649999885, 229.2404163060000144 ) ) ;
#12612 = CARTESIAN_POINT ( 'NONE',  ( -17.79876841389999598, 11.52736809249999617, -0.7999999992999995424 ) ) ;
#12613 = CARTESIAN_POINT ( 'NONE',  ( -7.999999999659028305, -18.20005812739434958, -36.62389201141883177 ) ) ;
#12614 = EDGE_CURVE ( 'NONE', #19704, #26138, #17414, .T. ) ;
#12615 = ORIENTED_EDGE ( 'NONE', *, *, #17550, .F. ) ;
#12616 = CARTESIAN_POINT ( 'NONE',  ( -24.36725163763869162, -13.38201776504303986, 4.999998581000003384 ) ) ;
#12617 = B_SPLINE_CURVE_WITH_KNOTS ( 'NONE', 3,
 ( #3818, #13405, #23019, #27887, #23175, #20807 ),
 .UNSPECIFIED., .F., .F.,
 ( 4, 2, 4 ),
 ( 0.000000000000000000, 0.5000000000000000000, 1.000000000000000000 ),
 .UNSPECIFIED. ) ;
#12618 = CARTESIAN_POINT ( 'NONE',  ( 0.03635086293632015797, -28.50041301604635180, 6.002517553000020101 ) ) ;
#12619 = CARTESIAN_POINT ( 'NONE',  ( -17.39542721470322917, -31.99978666472101096, -27.08953026176062195 ) ) ;
#12620 = CARTESIAN_POINT ( 'NONE',  ( -19.80535357367646654, 19.50875577052770993, 1.800000043000016259 ) ) ;
#12621 = PRESENTATION_LAYER_ASSIGNMENT (  '', '', ( #25184 ) ) ;
#12622 = DIRECTION ( 'NONE',  ( -4.250489863289427893E-14, -6.005940811918155400E-13, -1.000000000000000000 ) ) ;
#12623 = CARTESIAN_POINT ( 'NONE',  ( 4.790228392454985773, 0.1193559191107074896, -19.73911200060000937 ) ) ;
#12624 = CARTESIAN_POINT ( 'NONE',  ( -8.903108651239966420, -22.82508830966961000, 90.00000000000000000 ) ) ;
#12625 = CARTESIAN_POINT ( 'NONE',  ( -0.9565336352369326889, -27.48338672414943318, 5.548095501889124925 ) ) ;
#12626 = CARTESIAN_POINT ( 'NONE',  ( -24.50000001620000134, 3.000285568850000245E-15, 139.9999999960000139 ) ) ;
#12627 = CARTESIAN_POINT ( 'NONE',  ( -4.041451884329999800, 1.776356839399999804E-15, 230.8412452700000017 ) ) ;
#12628 = LINE ( 'NONE', #5396, #16740 ) ;
#12629 = B_SPLINE_CURVE_WITH_KNOTS ( 'NONE', 3,
 ( #24817, #29374, #22304, #8273, #22616, #3252, #5918, #7817, #27021, #17413 ),
 .UNSPECIFIED., .F., .F.,
 ( 4, 2, 2, 2, 4 ),
 ( 0.000000000000000000, 0.2500000000000000000, 0.5000000000000000000, 0.7500000000000000000, 1.000000000000000000 ),
 .UNSPECIFIED. ) ;
#12630 = CARTESIAN_POINT ( 'NONE',  ( -8.699999999628362346, -14.95623164695839513, -40.37561726986208299 ) ) ;
#12631 = CARTESIAN_POINT ( 'NONE',  ( 26.72922997839999582, 9.361173623819999179, 229.4485730460000070 ) ) ;
#12632 = CARTESIAN_POINT ( 'NONE',  ( -6.449395896350000434, -17.03876312330000076, 230.6999999999999886 ) ) ;
#12633 = VERTEX_POINT ( 'NONE', #22192 ) ;
#12634 = CARTESIAN_POINT ( 'NONE',  ( 0.8668428795416116550, 5.445660658778139762, -53.61500058692499238 ) ) ;
#12635 = LINE ( 'NONE', #14866, #260 ) ;
#12636 = CARTESIAN_POINT ( 'NONE',  ( -18.50495978126638619, 20.74626080822700658, 0.8585787019999846503 ) ) ;
#12637 = CARTESIAN_POINT ( 'NONE',  ( -4.204138849208283624, 0.5415514259779574679, -68.10000000002501963 ) ) ;
#12638 = EDGE_CURVE ( 'NONE', #7936, #28636, #12584, .T. ) ;
#12639 = ORIENTED_EDGE ( 'NONE', *, *, #26804, .F. ) ;
#12640 = EDGE_CURVE ( 'NONE', #16404, #27663, #10237, .T. ) ;
#12641 = CARTESIAN_POINT ( 'NONE',  ( 24.05715877174375095, -13.32261293489436227, 5.994883228945302456 ) ) ;
#12642 = CIRCLE ( 'NONE', #26730, 27.50000000000000000 ) ;
#12643 = VERTEX_POINT ( 'NONE', #3141 ) ;
#12645 = DIRECTION ( 'NONE',  ( 0.4999999999969509945, 0.4151946956549595336, 0.7600087925169251024 ) ) ;
#12644 = B_SPLINE_CURVE_WITH_KNOTS ( 'NONE', 3,
 ( #18443, #16397, #28041, #11210, #30880, #6956, #23802, #9311, #20812, #18910, #28510, #16549, #4591, #30419, #14199, #2247 ),
 .UNSPECIFIED., .F., .F.,
 ( 4, 2, 2, 2, 2, 2, 2, 4 ),
 ( 0.000000000000000000, 0.1249999999999999167, 0.2499999999999998335, 0.4999999999999998890, 0.6249999999999998890, 0.7499999999999998890, 0.8750000000000000000, 1.000000000000000000 ),
 .UNSPECIFIED. ) ;
#12646 = AXIS2_PLACEMENT_3D ( 'NONE', #19557, #17341, #24433 ) ;
#12647 = CARTESIAN_POINT ( 'NONE',  ( 23.69427943123108093, 14.54081805611945910, 6.079851352999988023 ) ) ;
#12648 = CIRCLE ( 'NONE', #30245, 1.699999999999999289 ) ;
#12649 = ORIENTED_EDGE ( 'NONE', *, *, #19427, .F. ) ;
#12650 = CARTESIAN_POINT ( 'NONE',  ( 6.118976883090258667, 2.212479739890888197, -27.11249766020000607 ) ) ;
#12651 = EDGE_CURVE ( 'NONE', #26737, #3218, #20045, .T. ) ;
#12652 = DIRECTION ( 'NONE',  ( -1.000000000000000000, -7.807837518030243978E-13, -2.626330150303133688E-12 ) ) ;
#12653 = CARTESIAN_POINT ( 'NONE',  ( -26.44963151265186241, 8.939294038675827281, -0.6577119969999878357 ) ) ;
#12654 = CARTESIAN_POINT ( 'NONE',  ( 24.83827260360999389, -12.48687744688666967, 4.999998581000003384 ) ) ;
#12655 = CARTESIAN_POINT ( 'NONE',  ( -28.49530731802708416, -0.5184832703812605192, 8.000000000000007105 ) ) ;
#12656 = CARTESIAN_POINT ( 'NONE',  ( -27.87609112763790975, 3.928995115430390150, 1.000000000000000888 ) ) ;
#12657 = ORIENTED_EDGE ( 'NONE', *, *, #2234, .F. ) ;
#12658 = CARTESIAN_POINT ( 'NONE',  ( 9.707106781189999367, -130.0000000000000000, -43.10710678118599759 ) ) ;
#12659 = MECHANICAL_DESIGN_GEOMETRIC_PRESENTATION_REPRESENTATION (  '', ( #23328 ), #5632 ) ;
#12660 = DIRECTION ( 'NONE',  ( 0.000000000000000000, -0.5000000000001900702, 0.8660254037843290176 ) ) ;
#12661 = AXIS2_PLACEMENT_3D ( 'NONE', #959, #25017, #29892 ) ;
#12662 = ORIENTED_EDGE ( 'NONE', *, *, #4072, .T. ) ;
#12663 = CARTESIAN_POINT ( 'NONE',  ( 16.20306687547020630, -21.42689369263764831, 36.78285841147714308 ) ) ;
#12664 = ADVANCED_FACE ( 'NONE', ( #26606 ), #5045, .F. ) ;
#12665 = CARTESIAN_POINT ( 'NONE',  ( -27.92857142820000149, 1.776356839399999804E-15, 187.9396849849999853 ) ) ;
#12666 = CARTESIAN_POINT ( 'NONE',  ( -6.760206787919999627, 10.32311405969999996, 232.6627643349999914 ) ) ;
#12667 = CARTESIAN_POINT ( 'NONE',  ( 10.82908725742651512, -27.76276047461856322, 43.21714158840000408 ) ) ;
#12668 = CARTESIAN_POINT ( 'NONE',  ( 9.999999999962223995, -25.75869229542447769, -25.66275671166319583 ) ) ;
#12669 = CARTESIAN_POINT ( 'NONE',  ( 10.69999999999173390, -129.7008471317687395, -38.73679577504942273 ) ) ;
#12670 = CARTESIAN_POINT ( 'NONE',  ( 3.555845164255195368, -2.474081261589745839, -0.6999999999999992895 ) ) ;
#12671 = CARTESIAN_POINT ( 'NONE',  ( -20.09263842094486208, -20.97086228454488932, -0.5592437529999827461 ) ) ;
#12672 = CARTESIAN_POINT ( 'NONE',  ( 1.099928585400369085, -27.47799405182496457, 4.854498941781074883 ) ) ;
#12673 = EDGE_CURVE ( 'NONE', #7731, #53, #24173, .T. ) ;
#12674 = CARTESIAN_POINT ( 'NONE',  ( -10.69999999969999926, -20.99999999999999645, -28.39999999999999858 ) ) ;
#12675 = CARTESIAN_POINT ( 'NONE',  ( 10.69999999930000101, -29.30501631380000305, -26.47986985000000004 ) ) ;
#12676 = CARTESIAN_POINT ( 'NONE',  ( -21.27344192715451499, -16.32329153680506195, 93.21714158846666010 ) ) ;
#12677 = CARTESIAN_POINT ( 'NONE',  ( -0.5968465743326634154, -28.49391676915515603, 5.208100973000007627 ) ) ;
#12678 = ORIENTED_EDGE ( 'NONE', *, *, #6449, .T. ) ;
#12679 = FACE_OUTER_BOUND ( 'NONE', #23338, .T. ) ;
#12680 =( NAMED_UNIT ( * ) SI_UNIT ( $, .STERADIAN. ) SOLID_ANGLE_UNIT ( ) );
#12681 = CARTESIAN_POINT ( 'NONE',  ( 24.11470756272141713, -15.18997277214834440, 224.7094697646042505 ) ) ;
#12682 = AXIS2_PLACEMENT_3D ( 'NONE', #17198, #550, #5090 ) ;
#12683 = CARTESIAN_POINT ( 'NONE',  ( 4.009291712408949770, -2.091746824018178685, -61.31790713612500099 ) ) ;
#12684 = ORIENTED_EDGE ( 'NONE', *, *, #3370, .T. ) ;
#12685 = EDGE_CURVE ( 'NONE', #29610, #29523, #24952, .T. ) ;
#12686 = B_SPLINE_CURVE_WITH_KNOTS ( 'NONE', 3,
 ( #13146, #6069, #14793, #24394, #17296, #23081, #25275, #30308, #29252, #27623, #24545, #10072, #2828, #15666, #10642, #3553, #11114, #1523, #3710, #18347, #20234, #20550, #13310, #20710, #3393, #22037, #1205, #8739, #20396, #1362, #10802, #8577, #17861, #1049, #488, #5909, #18178, #12998, #27782, #22610, #29828, #6227, #8266, #27467, #15511, #25118, #23232 ),
 .UNSPECIFIED., .F., .F.,
 ( 4, 2, 2, 2, 1, 1, 2, 2, 2, 2, 1, 1, 1, 2, 2, 2, 2, 1, 1, 1, 2, 2, 2, 2, 1, 2, 2, 4 ),
 ( 0.000000000000000000, 0.06250000000000112410, 0.1250000000000022482, 0.1875000000000033862, 0.2187499999999920897, 0.2343749999999864553, 0.2421874999999937272, 0.2500000000000009992, 0.3750000000001675882, 0.4375000000002438050, 0.4687500000002819411, 0.4843750000003009815, 0.4921875000003093081, 0.4960937500003123612, 0.5000000000003153033, 0.6250000000002886580, 0.6875000000002722267, 0.7187500000002626788, 0.7343750000002537970, 0.7421875000002519096, 0.7460937500002510214, 0.7500000000002501332, 0.8125000000001764144, 0.8437500000001433298, 0.8593750000001281197, 0.8671875000001204592, 0.8750000000001129097, 1.000000000000000000 ),
 .UNSPECIFIED. ) ;
#12687 = EDGE_LOOP ( 'NONE', ( #6706, #1123, #15365, #11997 ) ) ;
#12688 = CARTESIAN_POINT ( 'NONE',  ( 8.700000000301640668, -14.95611408989196711, -40.37595097046296644 ) ) ;
#12689 = ORIENTED_EDGE ( 'NONE', *, *, #22013, .F. ) ;
#12690 = VERTEX_POINT ( 'NONE', #8626 ) ;
#12691 = CARTESIAN_POINT ( 'NONE',  ( -1.010644225189164080, 2.923099265969618443, -42.24266576417440433 ) ) ;
#12692 = CARTESIAN_POINT ( 'NONE',  ( 25.16696686177720821, -13.37570800343109312, 3.997190761000024573 ) ) ;
#12693 = CARTESIAN_POINT ( 'NONE',  ( -24.95819290936903911, -13.76152695242329216, 224.0343809112593476 ) ) ;
#12694 = CARTESIAN_POINT ( 'NONE',  ( -27.79539923451739014, -0.5057481688648817197, 8.000000000000007105 ) ) ;
#12695 = CARTESIAN_POINT ( 'NONE',  ( 24.78870453580057998, -12.58522324566301620, 5.507123706999989210 ) ) ;
#12696 = CARTESIAN_POINT ( 'NONE',  ( 14.25032083441342934, -27.35421241409322946, 8.000000000000007105 ) ) ;
#12697 = ORIENTED_EDGE ( 'NONE', *, *, #1482, .T. ) ;
#12698 = CARTESIAN_POINT ( 'NONE',  ( 2.679732294349358668, -3.453994421436008988, -44.10000000002499121 ) ) ;
#12699 = EDGE_CURVE ( 'NONE', #25829, #22642, #29789, .T. ) ;
#12700 = DIRECTION ( 'NONE',  ( 4.428977494234582379E-12, 0.8987940462991651502, -0.4383711467890810676 ) ) ;
#12701 = EDGE_CURVE ( 'NONE', #3589, #11176, #4278, .T. ) ;
#12702 = CARTESIAN_POINT ( 'NONE',  ( -4.661300745825158742, -2.852033519363592173, -22.90799200640000777 ) ) ;
#12703 = CARTESIAN_POINT ( 'NONE',  ( -12.49647831262057451, -26.09796281691805575, -33.65229867019547072 ) ) ;
#12704 = CARTESIAN_POINT ( 'NONE',  ( -16.66945014389299828, 9.902801559243821217, -4.336808689942018722E-16 ) ) ;
#12705 = VECTOR ( 'NONE', #7417, 1000.000000000000000 ) ;
#12706 = DIRECTION ( 'NONE',  ( -1.000000000000000000, 0.000000000000000000, 0.000000000000000000 ) ) ;
#12707 = CARTESIAN_POINT ( 'NONE',  ( 8.700000000272996914, -17.90486156772228554, -33.94152562884548985 ) ) ;
#12708 = CARTESIAN_POINT ( 'NONE',  ( 1.634888019277630278, 4.633891277622259608, -45.09079303332500643 ) ) ;
#12709 = EDGE_CURVE ( 'NONE', #4812, #28386, #29729, .T. ) ;
#12710 = DIRECTION ( 'NONE',  ( 0.000000000000000000, -0.4794255386042043932, -0.8775825618903719816 ) ) ;
#12711 = CARTESIAN_POINT ( 'NONE',  ( 9.738910687886871642, -24.96785170200599069, 202.5331693087865403 ) ) ;
#12712 = CARTESIAN_POINT ( 'NONE',  ( -19.95189713873627468, 20.00011557594780243, 229.8872997436589003 ) ) ;
#12713 = CARTESIAN_POINT ( 'NONE',  ( -24.77829191970622347, -10.21159038398080376, 43.21714158839912301 ) ) ;
#12714 = CARTESIAN_POINT ( 'NONE',  ( -1.670464374220244963, 1.280497938789454837, 226.6412452697800290 ) ) ;
#12715 = ORIENTED_EDGE ( 'NONE', *, *, #21844, .T. ) ;
#12716 =( BOUNDED_SURFACE ( )  B_SPLINE_SURFACE ( 5, 5, ( 
 ( #27216, #29574, #12583, #17752, #5656, #15255 ),
 ( #10083, #29418, #5811, #26914, #3442, #19678 ),
 ( #5351, #14956, #24554, #13045, #22191, #22652 ),
 ( #7854, #1095, #29882, #27515, #1876, #5961 ),
 ( #21077, #1413, #27989, #30036, #4079, #15711 ),
 ( #11475, #23279, #25801, #18066, #6434, #30195 ),
 ( #25324, #16033, #25649, #15883, #30361, #13675 ),
 ( #17908, #1256, #25486, #15555, #18547, #6589 ),
 ( #8469, #18223, #18393, #8948, #20919, #8313 ),
 ( #13191, #25165, #3597, #16187, #3766, #10853 ),
 ( #8625, #1722, #22805, #27671, #20439, #6117 ),
 ( #3922, #13358, #22966, #11007, #20597, #23131 ),
 ( #4235, #20754, #13516, #27831, #6282, #1572 ),
 ( #11160, #28149, #8789, #11321, #30521, #13835 ),
 ( #23447, #18860, #30674, #16647, #28923, #14613 ),
 ( #18700, #19173, #9575, #16802, #4696, #9100 ),
 ( #23912, #28299, #28617, #6743, #14147, #2497 ),
 ( #28759, #4544, #16344, #12085, #25952, #7367 ),
 ( #26416, #4389, #13994, #7056, #14459, #9723 ),
 ( #23752, #5005, #24202, #11625, #24058, #9251 ),
 ( #21386, #26107, #21694, #26258, #2191, #142 ),
 ( #14305, #21223, #11781, #16959, #23601, #2643 ),
 ( #19330, #12237, #30978, #7213, #30823, #4858 ),
 ( #2347, #6892, #2037, #9410, #26564, #19014 ),
 ( #28458, #16320, #16495, #11931, #21539, #9883 ),
 ( #25250, #460, #7662, #8389, #6201, #17988 ),
 ( #22152, #17265, #26872, #8551, #10042, #10929 ),
 ( #5149, #19636, #5315, #29221, #14919, #10767 ),
 ( #24515, #608, #6040, #26713, #12394, #7517 ),
 ( #10195, #2952, #17418, #12546, #25093, #15803 ),
 ( #19795, #29378, #18149, #5882, #15489, #7820 ),
 ( #27754, #27026, #20368, #3524, #27600, #13121 ),
 ( #29960, #22728, #1177, #15639, #3682, #305 ),
 ( #13281, #29072, #1335, #20522, #22892, #22004 ),
 ( #30123, #25416, #3848, #21854, #14762, #19485 ),
 ( #17112, #24360, #2802, #30279, #28071, #13754 ),
 ( #18317, #4005, #8711, #1497, #23371, #18473 ),
 ( #20845, #30448, #1810, #8868, #11239, #20998 ),
 ( #28224, #27921, #30603, #11089, #21152, #11399 ),
 ( #26184, #6988, #6363, #9177, #20684, #4319 ),
 ( #6517, #13437, #16114, #16424, #25726, #4161 ),
 ( #30749, #18627, #23053, #18779, #6667, #15960 ),
 ( #25568, #9029, #26034, #30909, #23527, #16265 ),
 ( #4474, #13601, #11705, #23207, #28388, #1649 ),
 ( #25883, #6826, #23678, #13916, #1963, #18938 ),
 ( #11556, #14075, #2113, #21307, #9337, #28539 ),
 ( #16576, #19253, #19567, #12470, #2276, #2424 ),
 ( #21772, #382, #24280, #12326, #4932, #226 ),
 ( #29302, #31060, #9968, #11861, #26644, #19410 ),
 ( #17350, #7297, #7598, #28839, #73, #7745 ),
 ( #4620, #5083, #7447, #29151, #16885, #19723 ),
 ( #14542, #2729, #23832, #14225, #29000, #21464 ),
 ( #26489, #24135, #26341, #9498, #14691, #2574 ),
 ( #17191, #12163, #21933, #19099, #28694, #9812 ),
 ( #16721, #26794, #7139, #17042, #4789, #14386 ),
 ( #5238, #9651, #14853, #24444, #23985, #2878 ),
 ( #12015, #21620, #22085, #542, #10123, #20022 ),
 ( #17502, #22693, #3181, #6004, #30085, #10728 ),
 ( #5541, #25054, #17646, #1136, #12785, #3486 ),
 ( #3331, #17799, #13082, #27410, #5391, #19878 ),
 ( #3030, #15603, #25206, #12938, #27559, #838 ),
 ( #15146, #3640, #5848, #10278, #24746, #10430 ),
 ( #29619, #15452, #12623, #8051, #27258, #20328 ),
 ( #27107, #22234, #14998, #5695, #15302, #22548 ),
 ( #22394, #24906, #991, #10582, #20176, #29927 ),
 ( #29461, #29766, #24597, #8198, #8510, #8353 ),
 ( #17948, #13235, #26954, #22851, #690, #1299 ),
 ( #10893, #20484, #7896, #23325, #30871, #18434 ),
 ( #6159, #21267, #1770, #27713, #25844, #1610 ),
 ( #8671, #13399, #8991, #28031, #3964, #23485 ),
 ( #18591, #18111, #15761, #11199, #13717, #30238 ),
 ( #8829, #13562, #21117, #4120, #20801, #1923 ),
 ( #25373, #15920, #3812, #11360, #13878, #6630 ),
 ( #20957, #2077, #28187, #6476, #23169, #4434 ),
 ( #30563, #16229, #25528, #23010, #16077, #11515 ),
 ( #4281, #11051, #30713, #30408, #20642, #25689 ),
 ( #14038, #9140, #27880, #18743, #28344, #11669 ),
 ( #1458, #18269, #6790, #16386, #25994, #6325 ),
 ( #23640, #14189, #2838, #16540, #7561, #16688 ),
 ( #23954, #28797, #9456, #28655, #31020, #12126 ),
 ( #4581, #7260, #16850, #4747, #26299, #14353 ),
 ( #26149, #26758, #21732, #26456, #7102, #23791 ),
 ( #12286, #21586, #19529, #12433, #2389, #11974 ),
 ( #5194, #4899, #33, #9301, #9615, #14656 ),
 ( #17006, #7407, #14503, #184, #26608, #9772 ),
 ( #2237, #24100, #11828, #29117, #17152, #2538 ),
 ( #19215, #28499, #24244, #21899, #22051, #346 ),
 ( #18902, #21429, #14810, #19375, #19060, #28965 ),
 ( #5048, #2686, #9928, #24406, #6944, #26918 ),
 ( #8014, #27067, #7857, #17461, #19983, #5505 ),
 ( #17612, #8161, #15260, #14960, #27220, #19681 ),
 ( #5661, #13197, #25170, #5355, #27377, #7706 ),
 ( #24870, #15112, #501, #3144, #3447, #24706 ),
 ( #3602, #12742, #10087, #957, #3298, #5816 ),
 ( #15561, #12902, #29266, #802, #29733, #17312 ),
 ( #22510, #24559, #17757, #22355, #10392, #22195 ),
 ( #10547, #29578, #20142, #15414, #25014, #13049 ),
 ( #2997, #22656, #1099, #12587, #10692, #652 ),
 ( #10239, #19841, #29423, #20286, #29889, #8317 ),
 ( #17912, #27520, #5966, #10859, #16349, #20444 ),
 ( #4394, #15887, #11327, #13363, #18553, #30199 ),
 ( #8630, #18071, #1577, #6595, #25490, #25808 ),
 ( #18227, #25958, #6287, #22809, #23285, #25654 ),
 ( #3928, #6750, #27994, #1262, #23135, #20924 ),
 ( #30042, #6439, #8475, #30526, #13522, #11163 ),
 ( #27676, #6122, #20760, #16192, #1882, #20602 ),
 ( #28305, #15716, #3772, #4240, #1418, #27835 ),
 ( #30365, #13842, #8794, #18397, #23452, #30679 ) ),
 .UNSPECIFIED., .F., .F., .T. ) 
 B_SPLINE_SURFACE_WITH_KNOTS ( ( 6, 3, 3, 3, 3, 3, 3, 3, 3, 3, 3, 3, 3, 3, 3, 3, 3, 3, 3, 3, 3, 3, 3, 3, 3, 3, 3, 3, 3, 3, 3, 3, 3, 3, 3, 6 ),
 ( 6, 6 ),
 ( 0.000000000000000000, 11.38862009670000042, 23.17260734259999921, 34.79167593860000096, 46.25425528950000142, 57.87229377410000097, 69.67120816000000616, 81.20502170430000888, 92.80704244429999505, 104.1208912059999960, 115.9269080290000034, 127.3307717769999954, 139.1306782750000082, 150.7654282180000109, 162.2434640489999822, 173.6637378899999931, 185.2020570420000070, 194.1769840820000184, 203.3038760180000111, 212.5853790139999830, 224.1393301889999918, 235.6932813650000185, 246.8715721779999797, 258.4996770380000157, 270.1277818960000445, 281.7035649139999691, 293.2822232819999613, 304.6732510989999696, 316.1434960830000023, 327.6894369340000139, 339.2353777880000507, 350.7813186390000055, 362.5843219139999860, 374.0573691039999744, 385.8560256170000002, 397.5961180479999939 ),
 ( 0.000000000000000000, 8.337129679329999377 ),
 .UNSPECIFIED. ) 
 GEOMETRIC_REPRESENTATION_ITEM ( )  RATIONAL_B_SPLINE_SURFACE ( (
 ( 1.000000000000000000, 0.5999999999999999778, 0.4000000000000000222, 0.2999999999999999889, 0.2500000000000000000, 0.2500000000000000000),
 ( 1.000000000000000000, 0.5999999999999999778, 0.4000000000000000222, 0.2999999999999999889, 0.2500000000000000000, 0.2500000000000000000),
 ( 1.000000000000000000, 0.5999999999999999778, 0.4000000000000000222, 0.2999999999999999889, 0.2500000000000000000, 0.2500000000000000000),
 ( 1.000000000000000000, 0.5999999999999999778, 0.4000000000000000222, 0.2999999999999999889, 0.2500000000000000000, 0.2500000000000000000),
 ( 1.000000000000000000, 0.5999999999999999778, 0.4000000000000000222, 0.2999999999999999889, 0.2500000000000000000, 0.2500000000000000000),
 ( 1.000000000000000000, 0.5999999999999999778, 0.4000000000000000222, 0.2999999999999999889, 0.2500000000000000000, 0.2500000000000000000),
 ( 1.000000000000000000, 0.5999999999999999778, 0.4000000000000000222, 0.2999999999999999889, 0.2500000000000000000, 0.2500000000000000000),
 ( 1.000000000000000000, 0.5999999999999999778, 0.4000000000000000222, 0.2999999999999999889, 0.2500000000000000000, 0.2500000000000000000),
 ( 1.000000000000000000, 0.5999999999999999778, 0.4000000000000000222, 0.2999999999999999889, 0.2500000000000000000, 0.2500000000000000000),
 ( 1.000000000000000000, 0.5999999999999999778, 0.4000000000000000222, 0.2999999999999999889, 0.2500000000000000000, 0.2500000000000000000),
 ( 1.000000000000000000, 0.5999999999999999778, 0.4000000000000000222, 0.2999999999999999889, 0.2500000000000000000, 0.2500000000000000000),
 ( 1.000000000000000000, 0.5999999999999999778, 0.4000000000000000222, 0.2999999999999999889, 0.2500000000000000000, 0.2500000000000000000),
 ( 1.000000000000000000, 0.5999999999999999778, 0.4000000000000000222, 0.2999999999999999889, 0.2500000000000000000, 0.2500000000000000000),
 ( 1.000000000000000000, 0.5999999999999999778, 0.4000000000000000222, 0.2999999999999999889, 0.2500000000000000000, 0.2500000000000000000),
 ( 1.000000000000000000, 0.5999999999999999778, 0.4000000000000000222, 0.2999999999999999889, 0.2500000000000000000, 0.2500000000000000000),
 ( 1.000000000000000000, 0.5999999999999999778, 0.4000000000000000222, 0.2999999999999999889, 0.2500000000000000000, 0.2500000000000000000),
 ( 1.000000000000000000, 0.5999999999999999778, 0.4000000000000000222, 0.2999999999999999889, 0.2500000000000000000, 0.2500000000000000000),
 ( 1.000000000000000000, 0.5999999999999999778, 0.4000000000000000222, 0.2999999999999999889, 0.2500000000000000000, 0.2500000000000000000),
 ( 1.000000000000000000, 0.5999999999999999778, 0.4000000000000000222, 0.2999999999999999889, 0.2500000000000000000, 0.2500000000000000000),
 ( 1.000000000000000000, 0.5999999999999999778, 0.4000000000000000222, 0.2999999999999999889, 0.2500000000000000000, 0.2500000000000000000),
 ( 1.000000000000000000, 0.5999999999999999778, 0.4000000000000000222, 0.2999999999999999889, 0.2500000000000000000, 0.2500000000000000000),
 ( 1.000000000000000000, 0.5999999999999999778, 0.4000000000000000222, 0.2999999999999999889, 0.2500000000000000000, 0.2500000000000000000),
 ( 1.000000000000000000, 0.5999999999999999778, 0.4000000000000000222, 0.2999999999999999889, 0.2500000000000000000, 0.2500000000000000000),
 ( 1.000000000000000000, 0.5999999999999999778, 0.4000000000000000222, 0.2999999999999999889, 0.2500000000000000000, 0.2500000000000000000),
 ( 1.000000000000000000, 0.5999999999999999778, 0.4000000000000000222, 0.2999999999999999889, 0.2500000000000000000, 0.2500000000000000000),
 ( 1.000000000000000000, 0.5999999999999999778, 0.4000000000000000222, 0.2999999999999999889, 0.2500000000000000000, 0.2500000000000000000),
 ( 1.000000000000000000, 0.5999999999999999778, 0.4000000000000000222, 0.2999999999999999889, 0.2500000000000000000, 0.2500000000000000000),
 ( 1.000000000000000000, 0.5999999999999999778, 0.4000000000000000222, 0.2999999999999999889, 0.2500000000000000000, 0.2500000000000000000),
 ( 1.000000000000000000, 0.5999999999999999778, 0.4000000000000000222, 0.2999999999999999889, 0.2500000000000000000, 0.2500000000000000000),
 ( 1.000000000000000000, 0.5999999999999999778, 0.4000000000000000222, 0.2999999999999999889, 0.2500000000000000000, 0.2500000000000000000),
 ( 1.000000000000000000, 0.5999999999999999778, 0.4000000000000000222, 0.2999999999999999889, 0.2500000000000000000, 0.2500000000000000000),
 ( 1.000000000000000000, 0.5999999999999999778, 0.4000000000000000222, 0.2999999999999999889, 0.2500000000000000000, 0.2500000000000000000),
 ( 1.000000000000000000, 0.5999999999999999778, 0.4000000000000000222, 0.2999999999999999889, 0.2500000000000000000, 0.2500000000000000000),
 ( 1.000000000000000000, 0.5999999999999999778, 0.4000000000000000222, 0.2999999999999999889, 0.2500000000000000000, 0.2500000000000000000),
 ( 1.000000000000000000, 0.5999999999999999778, 0.4000000000000000222, 0.2999999999999999889, 0.2500000000000000000, 0.2500000000000000000),
 ( 1.000000000000000000, 0.5999999999999999778, 0.4000000000000000222, 0.2999999999999999889, 0.2500000000000000000, 0.2500000000000000000),
 ( 1.000000000000000000, 0.5999999999999999778, 0.4000000000000000222, 0.2999999999999999889, 0.2500000000000000000, 0.2500000000000000000),
 ( 1.000000000000000000, 0.5999999999999999778, 0.4000000000000000222, 0.2999999999999999889, 0.2500000000000000000, 0.2500000000000000000),
 ( 1.000000000000000000, 0.5999999999999999778, 0.4000000000000000222, 0.2999999999999999889, 0.2500000000000000000, 0.2500000000000000000),
 ( 1.000000000000000000, 0.5999999999999999778, 0.4000000000000000222, 0.2999999999999999889, 0.2500000000000000000, 0.2500000000000000000),
 ( 1.000000000000000000, 0.5999999999999999778, 0.4000000000000000222, 0.2999999999999999889, 0.2500000000000000000, 0.2500000000000000000),
 ( 1.000000000000000000, 0.5999999999999999778, 0.4000000000000000222, 0.2999999999999999889, 0.2500000000000000000, 0.2500000000000000000),
 ( 1.000000000000000000, 0.5999999999999999778, 0.4000000000000000222, 0.2999999999999999889, 0.2500000000000000000, 0.2500000000000000000),
 ( 1.000000000000000000, 0.5999999999999999778, 0.4000000000000000222, 0.2999999999999999889, 0.2500000000000000000, 0.2500000000000000000),
 ( 1.000000000000000000, 0.5999999999999999778, 0.4000000000000000222, 0.2999999999999999889, 0.2500000000000000000, 0.2500000000000000000),
 ( 1.000000000000000000, 0.5999999999999999778, 0.4000000000000000222, 0.2999999999999999889, 0.2500000000000000000, 0.2500000000000000000),
 ( 1.000000000000000000, 0.5999999999999999778, 0.4000000000000000222, 0.2999999999999999889, 0.2500000000000000000, 0.2500000000000000000),
 ( 1.000000000000000000, 0.5999999999999999778, 0.4000000000000000222, 0.2999999999999999889, 0.2500000000000000000, 0.2500000000000000000),
 ( 1.000000000000000000, 0.5999999999999999778, 0.4000000000000000222, 0.2999999999999999889, 0.2500000000000000000, 0.2500000000000000000),
 ( 1.000000000000000000, 0.5999999999999999778, 0.4000000000000000222, 0.2999999999999999889, 0.2500000000000000000, 0.2500000000000000000),
 ( 1.000000000000000000, 0.5999999999999999778, 0.4000000000000000222, 0.2999999999999999889, 0.2500000000000000000, 0.2500000000000000000),
 ( 1.000000000000000000, 0.5999999999999999778, 0.4000000000000000222, 0.2999999999999999889, 0.2500000000000000000, 0.2500000000000000000),
 ( 1.000000000000000000, 0.5999999999999999778, 0.4000000000000000222, 0.2999999999999999889, 0.2500000000000000000, 0.2500000000000000000),
 ( 1.000000000000000000, 0.5999999999999999778, 0.4000000000000000222, 0.2999999999999999889, 0.2500000000000000000, 0.2500000000000000000),
 ( 1.000000000000000000, 0.5999999999999999778, 0.4000000000000000222, 0.2999999999999999889, 0.2500000000000000000, 0.2500000000000000000),
 ( 1.000000000000000000, 0.5999999999999999778, 0.4000000000000000222, 0.2999999999999999889, 0.2500000000000000000, 0.2500000000000000000),
 ( 1.000000000000000000, 0.5999999999999999778, 0.4000000000000000222, 0.2999999999999999889, 0.2500000000000000000, 0.2500000000000000000),
 ( 1.000000000000000000, 0.5999999999999999778, 0.4000000000000000222, 0.2999999999999999889, 0.2500000000000000000, 0.2500000000000000000),
 ( 1.000000000000000000, 0.5999999999999999778, 0.4000000000000000222, 0.2999999999999999889, 0.2500000000000000000, 0.2500000000000000000),
 ( 1.000000000000000000, 0.5999999999999999778, 0.4000000000000000222, 0.2999999999999999889, 0.2500000000000000000, 0.2500000000000000000),
 ( 1.000000000000000000, 0.5999999999999999778, 0.4000000000000000222, 0.2999999999999999889, 0.2500000000000000000, 0.2500000000000000000),
 ( 1.000000000000000000, 0.5999999999999999778, 0.4000000000000000222, 0.2999999999999999889, 0.2500000000000000000, 0.2500000000000000000),
 ( 1.000000000000000000, 0.5999999999999999778, 0.4000000000000000222, 0.2999999999999999889, 0.2500000000000000000, 0.2500000000000000000),
 ( 1.000000000000000000, 0.5999999999999999778, 0.4000000000000000222, 0.2999999999999999889, 0.2500000000000000000, 0.2500000000000000000),
 ( 1.000000000000000000, 0.5999999999999999778, 0.4000000000000000222, 0.2999999999999999889, 0.2500000000000000000, 0.2500000000000000000),
 ( 1.000000000000000000, 0.5999999999999999778, 0.4000000000000000222, 0.2999999999999999889, 0.2500000000000000000, 0.2500000000000000000),
 ( 1.000000000000000000, 0.5999999999999999778, 0.4000000000000000222, 0.2999999999999999889, 0.2500000000000000000, 0.2500000000000000000),
 ( 1.000000000000000000, 0.5999999999999999778, 0.4000000000000000222, 0.2999999999999999889, 0.2500000000000000000, 0.2500000000000000000),
 ( 1.000000000000000000, 0.5999999999999999778, 0.4000000000000000222, 0.2999999999999999889, 0.2500000000000000000, 0.2500000000000000000),
 ( 1.000000000000000000, 0.5999999999999999778, 0.4000000000000000222, 0.2999999999999999889, 0.2500000000000000000, 0.2500000000000000000),
 ( 1.000000000000000000, 0.5999999999999999778, 0.4000000000000000222, 0.2999999999999999889, 0.2500000000000000000, 0.2500000000000000000),
 ( 1.000000000000000000, 0.5999999999999999778, 0.4000000000000000222, 0.2999999999999999889, 0.2500000000000000000, 0.2500000000000000000),
 ( 1.000000000000000000, 0.5999999999999999778, 0.4000000000000000222, 0.2999999999999999889, 0.2500000000000000000, 0.2500000000000000000),
 ( 1.000000000000000000, 0.5999999999999999778, 0.4000000000000000222, 0.2999999999999999889, 0.2500000000000000000, 0.2500000000000000000),
 ( 1.000000000000000000, 0.5999999999999999778, 0.4000000000000000222, 0.2999999999999999889, 0.2500000000000000000, 0.2500000000000000000),
 ( 1.000000000000000000, 0.5999999999999999778, 0.4000000000000000222, 0.2999999999999999889, 0.2500000000000000000, 0.2500000000000000000),
 ( 1.000000000000000000, 0.5999999999999999778, 0.4000000000000000222, 0.2999999999999999889, 0.2500000000000000000, 0.2500000000000000000),
 ( 1.000000000000000000, 0.5999999999999999778, 0.4000000000000000222, 0.2999999999999999889, 0.2500000000000000000, 0.2500000000000000000),
 ( 1.000000000000000000, 0.5999999999999999778, 0.4000000000000000222, 0.2999999999999999889, 0.2500000000000000000, 0.2500000000000000000),
 ( 1.000000000000000000, 0.5999999999999999778, 0.4000000000000000222, 0.2999999999999999889, 0.2500000000000000000, 0.2500000000000000000),
 ( 1.000000000000000000, 0.5999999999999999778, 0.4000000000000000222, 0.2999999999999999889, 0.2500000000000000000, 0.2500000000000000000),
 ( 1.000000000000000000, 0.5999999999999999778, 0.4000000000000000222, 0.2999999999999999889, 0.2500000000000000000, 0.2500000000000000000),
 ( 1.000000000000000000, 0.5999999999999999778, 0.4000000000000000222, 0.2999999999999999889, 0.2500000000000000000, 0.2500000000000000000),
 ( 1.000000000000000000, 0.5999999999999999778, 0.4000000000000000222, 0.2999999999999999889, 0.2500000000000000000, 0.2500000000000000000),
 ( 1.000000000000000000, 0.5999999999999999778, 0.4000000000000000222, 0.2999999999999999889, 0.2500000000000000000, 0.2500000000000000000),
 ( 1.000000000000000000, 0.5999999999999999778, 0.4000000000000000222, 0.2999999999999999889, 0.2500000000000000000, 0.2500000000000000000),
 ( 1.000000000000000000, 0.5999999999999999778, 0.4000000000000000222, 0.2999999999999999889, 0.2500000000000000000, 0.2500000000000000000),
 ( 1.000000000000000000, 0.5999999999999999778, 0.4000000000000000222, 0.2999999999999999889, 0.2500000000000000000, 0.2500000000000000000),
 ( 1.000000000000000000, 0.5999999999999999778, 0.4000000000000000222, 0.2999999999999999889, 0.2500000000000000000, 0.2500000000000000000),
 ( 1.000000000000000000, 0.5999999999999999778, 0.4000000000000000222, 0.2999999999999999889, 0.2500000000000000000, 0.2500000000000000000),
 ( 1.000000000000000000, 0.5999999999999999778, 0.4000000000000000222, 0.2999999999999999889, 0.2500000000000000000, 0.2500000000000000000),
 ( 1.000000000000000000, 0.5999999999999999778, 0.4000000000000000222, 0.2999999999999999889, 0.2500000000000000000, 0.2500000000000000000),
 ( 1.000000000000000000, 0.5999999999999999778, 0.4000000000000000222, 0.2999999999999999889, 0.2500000000000000000, 0.2500000000000000000),
 ( 1.000000000000000000, 0.5999999999999999778, 0.4000000000000000222, 0.2999999999999999889, 0.2500000000000000000, 0.2500000000000000000),
 ( 1.000000000000000000, 0.5999999999999999778, 0.4000000000000000222, 0.2999999999999999889, 0.2500000000000000000, 0.2500000000000000000),
 ( 1.000000000000000000, 0.5999999999999999778, 0.4000000000000000222, 0.2999999999999999889, 0.2500000000000000000, 0.2500000000000000000),
 ( 1.000000000000000000, 0.5999999999999999778, 0.4000000000000000222, 0.2999999999999999889, 0.2500000000000000000, 0.2500000000000000000),
 ( 1.000000000000000000, 0.5999999999999999778, 0.4000000000000000222, 0.2999999999999999889, 0.2500000000000000000, 0.2500000000000000000),
 ( 1.000000000000000000, 0.5999999999999999778, 0.4000000000000000222, 0.2999999999999999889, 0.2500000000000000000, 0.2500000000000000000),
 ( 1.000000000000000000, 0.5999999999999999778, 0.4000000000000000222, 0.2999999999999999889, 0.2500000000000000000, 0.2500000000000000000),
 ( 1.000000000000000000, 0.5999999999999999778, 0.4000000000000000222, 0.2999999999999999889, 0.2500000000000000000, 0.2500000000000000000),
 ( 1.000000000000000000, 0.5999999999999999778, 0.4000000000000000222, 0.2999999999999999889, 0.2500000000000000000, 0.2500000000000000000),
 ( 1.000000000000000000, 0.5999999999999999778, 0.4000000000000000222, 0.2999999999999999889, 0.2500000000000000000, 0.2500000000000000000),
 ( 1.000000000000000000, 0.5999999999999999778, 0.4000000000000000222, 0.2999999999999999889, 0.2500000000000000000, 0.2500000000000000000),
 ( 1.000000000000000000, 0.5999999999999999778, 0.4000000000000000222, 0.2999999999999999889, 0.2500000000000000000, 0.2500000000000000000),
 ( 1.000000000000000000, 0.5999999999999999778, 0.4000000000000000222, 0.2999999999999999889, 0.2500000000000000000, 0.2500000000000000000),
 ( 1.000000000000000000, 0.5999999999999999778, 0.4000000000000000222, 0.2999999999999999889, 0.2500000000000000000, 0.2500000000000000000),
 ( 1.000000000000000000, 0.5999999999999999778, 0.4000000000000000222, 0.2999999999999999889, 0.2500000000000000000, 0.2500000000000000000) ) ) 
 REPRESENTATION_ITEM ( '' )  SURFACE ( )  );
#12717 = CARTESIAN_POINT ( 'NONE',  ( -2.308365619037861638, -4.044857084274060988, -31.17642233979999844 ) ) ;
#12718 = EDGE_CURVE ( 'NONE', #19512, #30177, #18224, .T. ) ;
#12719 = ORIENTED_EDGE ( 'NONE', *, *, #3105, .F. ) ;
#12720 = CIRCLE ( 'NONE', #30324, 3.200000000000002398 ) ;
#12721 = CARTESIAN_POINT ( 'NONE',  ( -8.699999999673119433, -13.73066623916353102, -34.33432129195676197 ) ) ;
#12722 = CARTESIAN_POINT ( 'NONE',  ( 2.776548632478545553, -3.583402058917904753, -52.50430438132499233 ) ) ;
#12723 = ORIENTED_EDGE ( 'NONE', *, *, #11363, .F. ) ;
#12724 = AXIS2_PLACEMENT_3D ( 'NONE', #12627, #696, #19884 ) ;
#12725 = VERTEX_POINT ( 'NONE', #20441 ) ;
#12726 = CARTESIAN_POINT ( 'NONE',  ( -34.00000000000000000, 0.02001161822479287367, -0.05106179917585312866 ) ) ;
#12727 = ORIENTED_EDGE ( 'NONE', *, *, #22408, .T. ) ;
#12728 = ORIENTED_EDGE ( 'NONE', *, *, #8713, .T. ) ;
#12729 = AXIS2_PLACEMENT_3D ( 'NONE', #17148, #22347, #25008 ) ;
#12730 = B_SPLINE_CURVE_WITH_KNOTS ( 'NONE', 3,
 ( #26395, #28739, #7188, #9702, #14434, #19149 ),
 .UNSPECIFIED., .F., .F.,
 ( 4, 2, 4 ),
 ( 0.000000000000000000, 0.5000000000000000000, 1.000000000000000000 ),
 .UNSPECIFIED. ) ;
#12731 = LINE ( 'NONE', #5345, #26620 ) ;
#12732 = CARTESIAN_POINT ( 'NONE',  ( 23.94167923218795124, 14.12976891115827627, 3.920144559000027229 ) ) ;
#12733 = EDGE_CURVE ( 'NONE', #18457, #26221, #30595, .T. ) ;
#12734 = DIRECTION ( 'NONE',  ( 0.000000000000000000, 0.000000000000000000, 1.000000000000000000 ) ) ;
#12735 = CARTESIAN_POINT ( 'NONE',  ( 0.000000000000000000, 0.000000000000000000, 88.33953982530000815 ) ) ;
#12736 = CARTESIAN_POINT ( 'NONE',  ( 1.814857447021396585E-10, -114.8436363890427856, 0.6950649351682707255 ) ) ;
#12737 = CARTESIAN_POINT ( 'NONE',  ( -3.777365892340432296, 2.405994524213964425, -0.6999999999999989564 ) ) ;
#12738 = CARTESIAN_POINT ( 'NONE',  ( 7.105427357599999217E-15, 8.881784197000000993E-16, 228.3912452697800006 ) ) ;
#12739 = CARTESIAN_POINT ( 'NONE',  ( -26.79556473285982321, -0.4875557887251183442, -0.6999999999999784173 ) ) ;
#12740 = DIRECTION ( 'NONE',  ( 0.7071067811868604336, -0.6896931279344806764, 0.1559595757865139820 ) ) ;
#12741 = CARTESIAN_POINT ( 'NONE',  ( -3.711147652395973662, 4.588201686596787177, -14.60352819870001007 ) ) ;
#12742 = CARTESIAN_POINT ( 'NONE',  ( -4.188726303739424672, 1.192588472141205891, -30.80158078970000091 ) ) ;
#12743 = CARTESIAN_POINT ( 'NONE',  ( 2.131628207279999844E-14, 1.421085471519999843E-14, 231.6999999999999886 ) ) ;
#12744 = CARTESIAN_POINT ( 'NONE',  ( -0.1113126276967109224, 6.462009008202359794, -40.63090155202897336 ) ) ;
#12745 = CARTESIAN_POINT ( 'NONE',  ( 8.000000000264140709, -18.27877680372071723, -30.94409471150577318 ) ) ;
#12746 = CARTESIAN_POINT ( 'NONE',  ( -2.871635305848837305, -2.026181749455575609, 227.6510696331287420 ) ) ;
#12747 = CARTESIAN_POINT ( 'NONE',  ( 0.06886553587799999765, -27.80016486610000115, 226.0986540789999992 ) ) ;
#12748 = CARTESIAN_POINT ( 'NONE',  ( 3.503437880484509659, 2.636891074944046398, -32.36032172559999509 ) ) ;
#12749 = AXIS2_PLACEMENT_3D ( 'NONE', #5475, #5789, #22780 ) ;
#12750 = B_SPLINE_CURVE_WITH_KNOTS ( 'NONE', 3,
 ( #18105, #28024, #26144, #3959, #11194, #11355, #30707, #20951, #11509, #14032, #15913, #8985, #8824, #13712, #18585, #11662, #4113, #9134, #23786, #9295 ),
 .UNSPECIFIED., .F., .F.,
 ( 4, 1, 1, 1, 2, 2, 2, 1, 1, 1, 2, 2, 4 ),
 ( 0.000000000000000000, 0.1249999999999973910, 0.1874999999999968081, 0.2187499999999964195, 0.2343749999999971689, 0.2499999999999978906, 0.4999999999999924505, 0.6249999999999906741, 0.6874999999999898970, 0.7187499999999884537, 0.7343749999999886757, 0.7499999999999888978, 1.000000000000000000 ),
 .UNSPECIFIED. ) ;
#12751 = CIRCLE ( 'NONE', #7716, 0.9999999999999981126 ) ;
#12752 = CARTESIAN_POINT ( 'NONE',  ( 16.13219926443963814, 11.40100527538031905, -1.400000000000001910 ) ) ;
#12753 = LINE ( 'NONE', #3781, #3179 ) ;
#12754 = CARTESIAN_POINT ( 'NONE',  ( 1.115119965759999943, -28.47834310740000063, 224.7918990269999995 ) ) ;
#12755 = EDGE_LOOP ( 'NONE', ( #12146, #16252, #29408, #28819 ) ) ;
#12756 = CARTESIAN_POINT ( 'NONE',  ( 10.99999999979999998, 20.99999999999999645, -58.51619795479999908 ) ) ;
#12757 = CARTESIAN_POINT ( 'NONE',  ( -4.265551103502377650, -31.83942647549183746, -80.46693306215522057 ) ) ;
#12758 = ORIENTED_EDGE ( 'NONE', *, *, #8406, .T. ) ;
#12759 = DIRECTION ( 'NONE',  ( 0.3633921898465274913, -0.9316362575375355393, -0.000000000000000000 ) ) ;
#12760 = CYLINDRICAL_SURFACE ( 'NONE', #241, 1.099999999999998979 ) ;
#12761 = ADVANCED_FACE ( 'NONE', ( #23132 ), #12477, .T. ) ;
#12762 = ORIENTED_EDGE ( 'NONE', *, *, #26063, .T. ) ;
#12763 = DIRECTION ( 'NONE',  ( 0.000000000000000000, -1.000000000000000000, 0.000000000000000000 ) ) ;
#12764 = ORIENTED_EDGE ( 'NONE', *, *, #17166, .T. ) ;
#12765 = ORIENTED_EDGE ( 'NONE', *, *, #11427, .T. ) ;
#12766 = ADVANCED_FACE ( 'NONE', ( #30362 ), #26709, .F. ) ;
#12767 = ORIENTED_EDGE ( 'NONE', *, *, #25683, .F. ) ;
#12768 = DIRECTION ( 'NONE',  ( 0.2665630446479613780, 0.9085064176298685013, -0.3218077568259533061 ) ) ;
#12769 = ADVANCED_FACE ( 'NONE', ( #9884 ), #14614, .T. ) ;
#12770 = EDGE_CURVE ( 'NONE', #19970, #725, #11479, .T. ) ;
#12771 = AXIS2_PLACEMENT_3D ( 'NONE', #1661, #30920, #9042 ) ;
#12772 = LINE ( 'NONE', #12459, #22209 ) ;
#12774 = LINE ( 'NONE', #20168, #22353 ) ;
#12773 = CIRCLE ( 'NONE', #4245, 2.999999999999999556 ) ;
#12775 = AXIS2_PLACEMENT_3D ( 'NONE', #15427, #8487, #10704 ) ;
#12776 = CARTESIAN_POINT ( 'NONE',  ( -10.00000000000000000, 19.99999999999999645, -42.39999999999999858 ) ) ;
#12777 = CARTESIAN_POINT ( 'NONE',  ( -24.93720648713954446, 13.79881813474513486, 6.099998581000020792 ) ) ;
#12778 = AXIS2_PLACEMENT_3D ( 'NONE', #24245, #18903, #21430 ) ;
#12779 = CIRCLE ( 'NONE', #12258, 4.000000004070001225 ) ;
#12780 = CARTESIAN_POINT ( 'NONE',  ( 8.700000000244115128, -26.99999999999395328, -28.39999999994493862 ) ) ;
#12781 = B_SPLINE_CURVE_WITH_KNOTS ( 'NONE', 3,
 ( #27151, #10477, #29663, #8093, #15346, #15969, #16123, #27931, #4329, #14084 ),
 .UNSPECIFIED., .F., .F.,
 ( 4, 2, 2, 2, 4 ),
 ( 0.000000000000000000, 0.2500000000000000000, 0.5000000000000000000, 0.7500000000000000000, 1.000000000000000000 ),
 .UNSPECIFIED. ) ;
#12782 = CARTESIAN_POINT ( 'NONE',  ( -7.572771919371899862, -5.645290041039670470, -27.18920573570797217 ) ) ;
#12783 = DIRECTION ( 'NONE',  ( -1.000000000000000000, 0.000000000000000000, -2.253435535809999718E-12 ) ) ;
#12784 = CARTESIAN_POINT ( 'NONE',  ( -3.885731905334990799, 2.027028853511393613, -1.418764356299999418 ) ) ;
#12785 = CARTESIAN_POINT ( 'NONE',  ( -6.228182343209494043, 0.8662545139425728014, -18.65159460730000873 ) ) ;
#12786 = CARTESIAN_POINT ( 'NONE',  ( -26.80000000069999899, 3.281945028329999726E-15, 193.2171415869999862 ) ) ;
#12787 = CARTESIAN_POINT ( 'NONE',  ( -2.962149026499999369E-14, -27.50000000069999828, 6.100000000000000533 ) ) ;
#12788 = CARTESIAN_POINT ( 'NONE',  ( 1.952618749817809141, -10.18528401336400435, -102.7632020892250040 ) ) ;
#12789 = CARTESIAN_POINT ( 'NONE',  ( -28.49999999979999998, 4.805538726630000923, 229.0000000000000000 ) ) ;
#12790 = CIRCLE ( 'NONE', #14570, 6.000000000000001776 ) ;
#12791 = CARTESIAN_POINT ( 'NONE',  ( -10.06596365874885812, -25.80632433378972124, 190.0000000000000000 ) ) ;
#12792 = CARTESIAN_POINT ( 'NONE',  ( 18.95046173579999760, -18.95046173579999760, 193.2171415880000040 ) ) ;
#12793 = FACE_OUTER_BOUND ( 'NONE', #10643, .T. ) ;
#12794 = CARTESIAN_POINT ( 'NONE',  ( 10.14902473071748545, -26.01926976409366077, 37.93968498539999956 ) ) ;
#12795 = VECTOR ( 'NONE', #22402, 1000.000000000000000 ) ;
#12796 = B_SPLINE_CURVE_WITH_KNOTS ( 'NONE', 3,
 ( #13649, #11135, #23420, #23577, #11450, #22940 ),
 .UNSPECIFIED., .F., .F.,
 ( 4, 2, 4 ),
 ( 0.000000000000000000, 0.5000000000000000000, 1.000000000000000000 ),
 .UNSPECIFIED. ) ;
#12797 = VERTEX_POINT ( 'NONE', #610 ) ;
#12798 = CARTESIAN_POINT ( 'NONE',  ( 5.235465350887244185, -2.882605534178610984, -57.82843849682499382 ) ) ;
#12799 = DIRECTION ( 'NONE',  ( -2.256480420250000087E-12, 0.000000000000000000, -1.000000000000000000 ) ) ;
#12800 = AXIS2_PLACEMENT_3D ( 'NONE', #9388, #10022, #2624 ) ;
#12801 = VECTOR ( 'NONE', #28000, 1000.000000000000000 ) ;
#12802 = CARTESIAN_POINT ( 'NONE',  ( -16.60222294797364029, -7.918137930465035446, 0.000000000000000000 ) ) ;
#12803 = CARTESIAN_POINT ( 'NONE',  ( -3.795860071007379766, 2.267560867935308977, -38.58513250297124131 ) ) ;
#12804 = CARTESIAN_POINT ( 'NONE',  ( -4.163090791897414711, 0.1733432904813641262, -68.10000000002503384 ) ) ;
#12805 = VERTEX_POINT ( 'NONE', #760 ) ;
#12806 = VERTEX_POINT ( 'NONE', #5463 ) ;
#12807 = B_SPLINE_CURVE_WITH_KNOTS ( 'NONE', 3,
 ( #2603, #2308, #12192, #11735, #21963, #103 ),
 .UNSPECIFIED., .F., .F.,
 ( 4, 2, 4 ),
 ( 0.000000000000000000, 0.5000000000000000000, 1.000000000000000000 ),
 .UNSPECIFIED. ) ;
#12808 = CARTESIAN_POINT ( 'NONE',  ( -3.167970009343080484, 1.698775369061893636, -91.50574204942923018 ) ) ;
#12809 = PRODUCT_CONTEXT ( 'NONE', #28456, 'mechanical' ) ;
#12810 = ORIENTED_EDGE ( 'NONE', *, *, #22230, .T. ) ;
#12811 = DIRECTION ( 'NONE',  ( -0.7198537139083028835, 0.6941258031311204890, 0.000000000000000000 ) ) ;
#12812 = ADVANCED_FACE ( 'NONE', ( #5316 ), #17266, .T. ) ;
#12813 = VECTOR ( 'NONE', #13602, 1000.000000000000000 ) ;
#12814 = STYLED_ITEM ( 'NONE', ( #8539 ), #172 ) ;
#12815 = DIRECTION ( 'NONE',  ( -0.9316362575375349842, 0.3633921898465292122, -0.000000000000000000 ) ) ;
#12816 = VERTEX_POINT ( 'NONE', #12395 ) ;
#12817 = CARTESIAN_POINT ( 'NONE',  ( 3.225090657556859419, -3.689912930009636938, -63.74605006312501132 ) ) ;
#12818 = CARTESIAN_POINT ( 'NONE',  ( -13.70937177049999889, -27.52670431439999987, 229.4485705059999816 ) ) ;
#12819 = CARTESIAN_POINT ( 'NONE',  ( -27.47766015528786454, 9.286741218802717412, 0.2374258030000131470 ) ) ;
#12820 = DIRECTION ( 'NONE',  ( -0.3090169943750401549, -0.9510565162951233331, -1.149808922022230860E-31 ) ) ;
#12821 = CIRCLE ( 'NONE', #3263, 3.500000000000002220 ) ;
#12822 = CARTESIAN_POINT ( 'NONE',  ( 0.1455402980897219090, -27.50000000000000711, 223.8999999999999773 ) ) ;
#12823 = FACE_OUTER_BOUND ( 'NONE', #2306, .T. ) ;
#12824 = ORIENTED_EDGE ( 'NONE', *, *, #1777, .F. ) ;
#12825 = UNCERTAINTY_MEASURE_WITH_UNIT (LENGTH_MEASURE( 1.000000000000000082E-05 ), #3705, 'distance_accuracy_value', 'NONE');
#12826 = CARTESIAN_POINT ( 'NONE',  ( 24.93720649360215802, -13.79881813812812297, 3.899998581000013509 ) ) ;
#12827 = CARTESIAN_POINT ( 'NONE',  ( 18.62327035899999572, 19.80375215579999804, 229.9327584799999897 ) ) ;
#12828 = ORIENTED_EDGE ( 'NONE', *, *, #8593, .T. ) ;
#12829 = CARTESIAN_POINT ( 'NONE',  ( 0.000000000000000000, 0.000000000000000000, 90.00000000000000000 ) ) ;
#12830 = ADVANCED_FACE ( 'NONE', ( #24666, #28924 ), #461, .F. ) ;
#12831 = CARTESIAN_POINT ( 'NONE',  ( -24.25742564193969031, -13.58028021372842531, 5.680679499000030219 ) ) ;
#12832 = DIRECTION ( 'NONE',  ( -0.8090169943751909232, 0.5877852522921378498, 0.000000000000000000 ) ) ;
#12833 = CARTESIAN_POINT ( 'NONE',  ( 27.23548386990000125, -3.335274659639999982E-15, 141.6604601740000078 ) ) ;
#12834 = DIRECTION ( 'NONE',  ( 0.000000000000000000, 0.000000000000000000, 1.000000000000000000 ) ) ;
#12835 = CARTESIAN_POINT ( 'NONE',  ( 1.158713442569508478, -3.699378802302395908, -0.6999999999999992895 ) ) ;
#12836 = CARTESIAN_POINT ( 'NONE',  ( -28.35945636591989683, -7.983396444576476902, 1.000000000000000888 ) ) ;
#12837 = CARTESIAN_POINT ( 'NONE',  ( -9.500000000000000000, 21.70000000000000284, -64.10000000019999788 ) ) ;
#12838 = VECTOR ( 'NONE', #28695, 999.9999999999998863 ) ;
#12839 = COLOUR_RGB ( '', 0.66274510, 0.83137255, 0.94901961) ;
#12840 = DIRECTION ( 'NONE',  ( 0.000000000000000000, -0.8660254037590263687, -0.5000000000440152359 ) ) ;
#12841 = FACE_OUTER_BOUND ( 'NONE', #8695, .T. ) ;
#12842 = ADVANCED_FACE ( 'NONE', ( #24203 ), #5006, .F. ) ;
#12843 = CARTESIAN_POINT ( 'NONE',  ( -26.80000000069999899, 3.281945028329999726E-15, 87.11018146770000214 ) ) ;
#12844 = CARTESIAN_POINT ( 'NONE',  ( -0.6094664100040195764, -28.49364619262437870, 5.104049977999985721 ) ) ;
#12845 = ORIENTED_EDGE ( 'NONE', *, *, #12323, .T. ) ;
#12846 = CARTESIAN_POINT ( 'NONE',  ( 10.49243769669999971, -24.66097101770000322, -1.192453590699998900 ) ) ;
#12847 = CARTESIAN_POINT ( 'NONE',  ( -10.89131017139999891, -25.00000000000000000, -1.811764705899998606 ) ) ;
#12848 = DIRECTION ( 'NONE',  ( 0.000000000000000000, -1.000000000000000000, 0.000000000000000000 ) ) ;
#12849 = CARTESIAN_POINT ( 'NONE',  ( -4.631110635561381805, 2.546857509239208728, -60.56908057272499235 ) ) ;
#12850 = ORIENTED_EDGE ( 'NONE', *, *, #27103, .T. ) ;
#12851 = ORIENTED_EDGE ( 'NONE', *, *, #12893, .F. ) ;
#12852 = CARTESIAN_POINT ( 'NONE',  ( 23.25025823367671407, -19.81038070381301353, 0.2686784570000155803 ) ) ;
#12853 = VERTEX_POINT ( 'NONE', #2644 ) ;
#12854 = EDGE_CURVE ( 'NONE', #19996, #14172, #24362, .T. ) ;
#12855 = ORIENTED_EDGE ( 'NONE', *, *, #23724, .T. ) ;
#12856 = CARTESIAN_POINT ( 'NONE',  ( 9.999999999969999109, -29.12127062269999911, -30.52127062070000107 ) ) ;
#12857 = CARTESIAN_POINT ( 'NONE',  ( -23.52368442185878195, -12.84078897091760929, 225.9137588022049385 ) ) ;
#12858 = CARTESIAN_POINT ( 'NONE',  ( 9.414213562409999625, -14.63015244271202420, -76.33162510583964888 ) ) ;
#12859 = CARTESIAN_POINT ( 'NONE',  ( -25.24918301675066346, 13.28546534817111180, 8.000000000000007105 ) ) ;
#12860 = FACE_OUTER_BOUND ( 'NONE', #19239, .T. ) ;
#12861 = CARTESIAN_POINT ( 'NONE',  ( -2.664535259099999568E-14, -26.80000000000000071, 115.0000000000000000 ) ) ;
#12862 = ORIENTED_EDGE ( 'NONE', *, *, #20435, .F. ) ;
#12863 = CARTESIAN_POINT ( 'NONE',  ( 2.463209041803821275, -4.101496315139196547, -44.10000000002499121 ) ) ;
#12864 = CARTESIAN_POINT ( 'NONE',  ( -9.993285220779545952, -25.61999708228220740, 143.6055512749999821 ) ) ;
#12865 = CARTESIAN_POINT ( 'NONE',  ( 5.195105410215491659, 3.969764343816663210, -23.96727430110000157 ) ) ;
#12866 = DIRECTION ( 'NONE',  ( 0.000000000000000000, 0.000000000000000000, -1.000000000000000000 ) ) ;
#12867 = LINE ( 'NONE', #5322, #23064 ) ;
#12868 = B_SPLINE_CURVE_WITH_KNOTS ( 'NONE', 3,
 ( #10474, #27605, #8717, #25573, #6206, #29660, #30128, #1031, #8090, #1182, #13606, #3852, #3688, #17681 ),
 .UNSPECIFIED., .F., .F.,
 ( 4, 2, 2, 2, 2, 2, 4 ),
 ( 0.000000000000000000, 0.2500000000000015543, 0.3750000000000019984, 0.4375000000000020539, 0.5000000000000021094, 0.7500000000000011102, 1.000000000000000000 ),
 .UNSPECIFIED. ) ;
#12869 = DIRECTION ( 'NONE',  ( 0.6343890248118320141, 0.7730139489027949562, 0.000000000000000000 ) ) ;
#12870 = CARTESIAN_POINT ( 'NONE',  ( -8.999999998369998977, 20.99999999999999645, -60.10000000000000142 ) ) ;
#12871 = CARTESIAN_POINT ( 'NONE',  ( -2.571638601809289160, 3.775240214263653193, -47.65391720702500322 ) ) ;
#12872 = EDGE_CURVE ( 'NONE', #16829, #3809, #3479, .T. ) ;
#12873 = DIRECTION ( 'NONE',  ( -1.000000000000000000, 0.000000000000000000, 0.000000000000000000 ) ) ;
#12874 = CARTESIAN_POINT ( 'NONE',  ( 5.159343048259787068, -26.29982486972313183, 209.3149099368865791 ) ) ;
#12875 = CARTESIAN_POINT ( 'NONE',  ( -19.67993405796693196, 20.00031463343183447, 230.1485629155865240 ) ) ;
#12876 = CARTESIAN_POINT ( 'NONE',  ( -27.79999999999999716, -2.360422968200000068E-11, 229.0000000000000000 ) ) ;
#12877 = DIRECTION ( 'NONE',  ( 0.000000000000000000, 1.000000000000000000, 0.000000000000000000 ) ) ;
#12878 = ORIENTED_EDGE ( 'NONE', *, *, #18704, .T. ) ;
#12879 = CARTESIAN_POINT ( 'NONE',  ( -0.4593365651765490831, 6.553622599173768215, -35.49518930509999848 ) ) ;
#12880 = ORIENTED_EDGE ( 'NONE', *, *, #13840, .F. ) ;
#12881 = EDGE_CURVE ( 'NONE', #24088, #29870, #19796, .T. ) ;
#12882 = CARTESIAN_POINT ( 'NONE',  ( 13.92209366199456255, 21.69999999994632489, -67.88485145451890901 ) ) ;
#12883 = CARTESIAN_POINT ( 'NONE',  ( 5.477347162681518000, -0.4051096195737657335, -49.92442242802499663 ) ) ;
#12884 = ORIENTED_EDGE ( 'NONE', *, *, #20600, .F. ) ;
#12885 = ORIENTED_EDGE ( 'NONE', *, *, #1679, .F. ) ;
#12886 = EDGE_CURVE ( 'NONE', #27858, #4970, #10351, .T. ) ;
#12887 = VERTEX_POINT ( 'NONE', #29993 ) ;
#12888 = ORIENTED_EDGE ( 'NONE', *, *, #9351, .F. ) ;
#12889 = CARTESIAN_POINT ( 'NONE',  ( 16.27478637889808510, -8.340113109526685164, -4.336808689942018722E-16 ) ) ;
#12890 = CARTESIAN_POINT ( 'NONE',  ( 24.75645985066740806, 14.12045945716145390, 4.098702612000016288 ) ) ;
#12891 = CARTESIAN_POINT ( 'NONE',  ( 10.69999999999999929, -27.00000000000000000, -28.40000000000000213 ) ) ;
#12892 = CARTESIAN_POINT ( 'NONE',  ( 2.327075022089611256, 4.449294111946768382, -35.69999999999998863 ) ) ;
#12893 = EDGE_CURVE ( 'NONE', #125, #14489, #9496, .T. ) ;
#12894 = DIRECTION ( 'NONE',  ( 0.000000000000000000, 0.000000000000000000, -1.000000000000000000 ) ) ;
#12895 = CARTESIAN_POINT ( 'NONE',  ( -12.31579099197323934, -29.88626075205729293, -24.29306848462797319 ) ) ;
#12896 = CARTESIAN_POINT ( 'NONE',  ( -4.724067226770716665, 1.405641512842028762, -0.6999999999999991784 ) ) ;
#12897 = DIRECTION ( 'NONE',  ( 0.000000000000000000, 0.3420201433259318358, -0.9396926207858125046 ) ) ;
#12898 = CARTESIAN_POINT ( 'NONE',  ( 10.69999999999999929, -27.00000000000000000, -31.39999999999999858 ) ) ;
#12899 = CARTESIAN_POINT ( 'NONE',  ( -18.25755939615993739, 19.99998186964045743, -0.6768317722208874176 ) ) ;
#12900 = ORIENTED_EDGE ( 'NONE', *, *, #16530, .F. ) ;
#12901 = CARTESIAN_POINT ( 'NONE',  ( 0.8539377161337347033, 4.705374660993639324, -14.96150681849999842 ) ) ;
#12902 = CARTESIAN_POINT ( 'NONE',  ( -1.932773295258167545, 4.259541830411040841, -31.22635571289999845 ) ) ;
#12903 = ADVANCED_FACE ( 'NONE', ( #22932 ), #25128, .T. ) ;
#12904 = CARTESIAN_POINT ( 'NONE',  ( 16.89916710617796625, 9.923792022417691427, -0.000000000000000000 ) ) ;
#12905 = CARTESIAN_POINT ( 'NONE',  ( -24.60699806910000120, -12.93667933180000063, 225.0000014190000002 ) ) ;
#12906 = DIRECTION ( 'NONE',  ( 1.000000000000000000, 0.000000000000000000, 0.000000000000000000 ) ) ;
#12907 = CARTESIAN_POINT ( 'NONE',  ( 0.1033071333810000048, -27.80005613150000343, 226.0959520840000039 ) ) ;
#12908 = CARTESIAN_POINT ( 'NONE',  ( -8.699999999724179034, -29.73863906514459643, -27.17531388891805477 ) ) ;
#12909 = CARTESIAN_POINT ( 'NONE',  ( -27.23548387100000312, 3.552713678799999608E-15, 38.33953982530000104 ) ) ;
#12910 = DIRECTION ( 'NONE',  ( 0.3633921898465276024, -0.9316362575375355393, 2.168404344971008868E-14 ) ) ;
#12911 = CARTESIAN_POINT ( 'NONE',  ( -27.50000000000000000, 3.552713678799999608E-15, 93.60555127549999099 ) ) ;
#12912 = VERTEX_POINT ( 'NONE', #18027 ) ;
#12913 = EDGE_CURVE ( 'NONE', #16560, #29420, #22765, .T. ) ;
#12914 = DIRECTION ( 'NONE',  ( 1.000000000000000000, -1.843431230200084908E-12, 2.650498504963248473E-12 ) ) ;
#12915 = DIRECTION ( 'NONE',  ( 0.3633921898465274913, -0.9316362575375355393, -0.000000000000000000 ) ) ;
#12916 = VERTEX_POINT ( 'NONE', #25452 ) ;
#12917 = CARTESIAN_POINT ( 'NONE',  ( -7.999999999691694619, -25.92947359974649046, -31.20249410826873415 ) ) ;
#12918 = CARTESIAN_POINT ( 'NONE',  ( -1.100001419170000050, -27.77850706310000106, 225.0000014190000002 ) ) ;
#12919 = PRESENTATION_LAYER_ASSIGNMENT (  '', '', ( #869 ) ) ;
#12920 = ORIENTED_EDGE ( 'NONE', *, *, #16435, .F. ) ;
#12921 = CARTESIAN_POINT ( 'NONE',  ( 17.93011078765611543, -8.208160914697428368, -0.6999999989999727834 ) ) ;
#12922 = ORIENTED_EDGE ( 'NONE', *, *, #24808, .F. ) ;
#12923 = ORIENTED_EDGE ( 'NONE', *, *, #24895, .T. ) ;
#12924 = SHAPE_REPRESENTATION_RELATIONSHIP ( 'NONE' , 'NONE' ,  #527, #21175 ) ;
#12925 = ORIENTED_EDGE ( 'NONE', *, *, #23939, .F. ) ;
#12926 = CARTESIAN_POINT ( 'NONE',  ( 0.000000000000000000, 0.000000000000000000, 0.000000000000000000 ) ) ;
#12927 = CYLINDRICAL_SURFACE ( 'NONE', #23725, 2.999999999999999556 ) ;
#12928 = CARTESIAN_POINT ( 'NONE',  ( -7.999999999654106908, -17.47950540273041753, -37.52766237889763801 ) ) ;
#12929 = ORIENTED_EDGE ( 'NONE', *, *, #7016, .T. ) ;
#12930 = CARTESIAN_POINT ( 'NONE',  ( -24.44015551247796836, 13.24969167840070483, 6.079865069000017996 ) ) ;
#12931 = PRODUCT_DEFINITION_SHAPE ( 'NONE', 'NONE',  #31127 ) ;
#12932 = CARTESIAN_POINT ( 'NONE',  ( 20.77600629932058851, 21.68409807857665683, 8.000000000000007105 ) ) ;
#12933 = CARTESIAN_POINT ( 'NONE',  ( -7.195957063952547195, -5.577897551235623474, -27.03850287102680738 ) ) ;
#12934 = CARTESIAN_POINT ( 'NONE',  ( 23.95489023949999918, -14.10735628980000023, 223.9201486480000085 ) ) ;
#12935 = VERTEX_POINT ( 'NONE', #22621 ) ;
#12936 = AXIS2_PLACEMENT_3D ( 'NONE', #7052, #2641, #7515 ) ;
#12937 = CARTESIAN_POINT ( 'NONE',  ( -5.440024667461782037, 2.837840394948672351, -2.018764356300002838 ) ) ;
#12938 = CARTESIAN_POINT ( 'NONE',  ( -0.9576357401321299312, 5.433995450232204760, -18.83583244400000112 ) ) ;
#12939 = DIRECTION ( 'NONE',  ( 0.000000000000000000, 1.000000000000000000, 0.000000000000000000 ) ) ;
#12940 = TOROIDAL_SURFACE ( 'NONE', #13430, 24.50000000000000000, 4.000000000000000000 ) ;
#12941 = ADVANCED_FACE ( 'NONE', ( #1373 ), #1218, .F. ) ;
#12942 = CARTESIAN_POINT ( 'NONE',  ( 24.35364645778183146, 13.40687562030597135, 5.286753706817813203 ) ) ;
#12943 = CARTESIAN_POINT ( 'NONE',  ( -1.871333206045247888, -4.859327160240900056, -93.29359154310911606 ) ) ;
#12944 = CARTESIAN_POINT ( 'NONE',  ( -27.35138618339999894, 9.563610239860000917, 229.7625741969999922 ) ) ;
#12945 = CARTESIAN_POINT ( 'NONE',  ( 10.69999999999999929, -30.49251257979999963, -21.04205368479999905 ) ) ;
#12946 = EDGE_CURVE ( 'NONE', #29443, #21756, #27122, .T. ) ;
#12947 = CARTESIAN_POINT ( 'NONE',  ( -2.131591337306473655, 2.813577582285920364, -0.6999999999999784173 ) ) ;
#12948 = CARTESIAN_POINT ( 'NONE',  ( -5.114260856059999583, -17.43050419540000107, 230.6999999999999886 ) ) ;
#12949 = CARTESIAN_POINT ( 'NONE',  ( 23.70578532235928648, -13.93854223105014967, 223.9122931966472834 ) ) ;
#12950 = ORIENTED_EDGE ( 'NONE', *, *, #25582, .F. ) ;
#12951 = CARTESIAN_POINT ( 'NONE',  ( -2.948077164825084306, -3.495793300896363753, -59.17407541852499975 ) ) ;
#12952 = CARTESIAN_POINT ( 'NONE',  ( 16.40303402075260308, 10.20816091466531716, -0.6999999989999727834 ) ) ;
#12953 = CARTESIAN_POINT ( 'NONE',  ( -1.657635364023947400, -6.345118362804027079, -12.55022317840000312 ) ) ;
#12954 = CARTESIAN_POINT ( 'NONE',  ( -18.13789968716447731, 20.33475262164161279, 0.08279786600001726171 ) ) ;
#12955 = CARTESIAN_POINT ( 'NONE',  ( -4.246009911492877542, 0.8938096538029302041, -68.10000000002499121 ) ) ;
#12956 = ORIENTED_EDGE ( 'NONE', *, *, #8289, .F. ) ;
#12957 = VERTEX_POINT ( 'NONE', #8589 ) ;
#12958 = AXIS2_PLACEMENT_3D ( 'NONE', #17668, #29950, #22418 ) ;
#12959 = CARTESIAN_POINT ( 'NONE',  ( 2.928055646114741783, 2.216507990467923683, -91.89588846697527913 ) ) ;
#12960 = PRESENTATION_STYLE_ASSIGNMENT (( #17367 ) ) ;
#12961 = ORIENTED_EDGE ( 'NONE', *, *, #12946, .T. ) ;
#12962 = AXIS2_PLACEMENT_3D ( 'NONE', #26044, #21314, #30917 ) ;
#12963 = CARTESIAN_POINT ( 'NONE',  ( 23.57322167201318663, 14.73624931494496693, 6.002747145999992817 ) ) ;
#12964 = CARTESIAN_POINT ( 'NONE',  ( -5.941465883516308999, 0.03012783874251079297, -62.09122063482499243 ) ) ;
#12965 = CARTESIAN_POINT ( 'NONE',  ( -10.69999999999999929, -29.30501631370000482, -26.47986984990000181 ) ) ;
#12966 = B_SPLINE_CURVE_WITH_KNOTS ( 'NONE', 3,
 ( #14141, #4073, #23746, #2183, #11775, #23907, #21381, #30972, #28613, #7051 ),
 .UNSPECIFIED., .F., .F.,
 ( 4, 2, 2, 2, 4 ),
 ( 0.000000000000000000, 0.2500000000000000000, 0.5000000000000000000, 0.7500000000000000000, 1.000000000000000000 ),
 .UNSPECIFIED. ) ;
#12967 = CARTESIAN_POINT ( 'NONE',  ( -26.87967798701711786, 4.135222155429991275, -0.6999999999999784173 ) ) ;
#12968 = DIRECTION ( 'NONE',  ( 0.7198537139083028835, -0.6941258031311204890, 0.000000000000000000 ) ) ;
#12969 = SURFACE_SIDE_STYLE ('',( #10764 ) ) ;
#12970 = FACE_OUTER_BOUND ( 'NONE', #20495, .T. ) ;
#12971 = CONICAL_SURFACE ( 'NONE', #925, 0.9999999999991020516, 0.7853981633970000820 ) ;
#12972 = ORIENTED_EDGE ( 'NONE', *, *, #8126, .F. ) ;
#12973 = CARTESIAN_POINT ( 'NONE',  ( 0.5612683727491727392, -26.79446734626967341, 5.957452581394321101 ) ) ;
#12974 = DIRECTION ( 'NONE',  ( -1.000000000000000000, 5.687697999151106851E-16, -6.771501495036750356E-12 ) ) ;
#12975 = ORIENTED_EDGE ( 'NONE', *, *, #16901, .F. ) ;
#12976 = CARTESIAN_POINT ( 'NONE',  ( 24.60666743799999878, -12.93650359530000138, 224.8958210039999983 ) ) ;
#12977 = CARTESIAN_POINT ( 'NONE',  ( -24.41841039498785193, -14.69667350221323865, 6.099998581000020792 ) ) ;
#12978 = DIRECTION ( 'NONE',  ( -0.7071067811865475727, -0.7071067811865475727, 0.000000000000000000 ) ) ;
#12979 = EDGE_CURVE ( 'NONE', #15367, #17295, #27634, .T. ) ;
#12980 = CARTESIAN_POINT ( 'NONE',  ( 27.06563794070000029, -3.314475219239999417E-15, 141.9402686260000053 ) ) ;
#12981 = CARTESIAN_POINT ( 'NONE',  ( -9.481612630793593510, -25.06681236668577739, 204.0987691141152709 ) ) ;
#12982 = CARTESIAN_POINT ( 'NONE',  ( -16.95618186250884563, -7.902051487308459521, 0.000000000000000000 ) ) ;
#12983 = CARTESIAN_POINT ( 'NONE',  ( -23.57322167415998138, -14.73624932338542060, 6.002747143000003227 ) ) ;
#12985 = EDGE_CURVE ( 'NONE', #13797, #11464, #13323, .T. ) ;
#12984 = DIRECTION ( 'NONE',  ( -7.759996349202911684E-13, -0.9341647027306021478, -0.3568421334038983650 ) ) ;
#12986 = ORIENTED_EDGE ( 'NONE', *, *, #29676, .T. ) ;
#12987 = FACE_OUTER_BOUND ( 'NONE', #13876, .T. ) ;
#12988 = DIRECTION ( 'NONE',  ( 0.000000000000000000, -1.000000000000000000, 0.000000000000000000 ) ) ;
#12989 = CARTESIAN_POINT ( 'NONE',  ( -27.06563796540000411, 3.314475222269999560E-15, 88.05973140640000452 ) ) ;
#12990 = CARTESIAN_POINT ( 'NONE',  ( 0.4024591535012043697, -27.79733476277325721, 6.095949245000009675 ) ) ;
#12991 = AXIS2_PLACEMENT_3D ( 'NONE', #18507, #28109, #4350 ) ;
#12992 = DIRECTION ( 'NONE',  ( 0.000000000000000000, 0.000000000000000000, 1.000000000000000000 ) ) ;
#12993 = FILL_AREA_STYLE_COLOUR ( '', #28805 ) ;
#12994 = CYLINDRICAL_SURFACE ( 'NONE', #24748, 26.80000000000002203 ) ;
#12995 = CARTESIAN_POINT ( 'NONE',  ( -26.38304356803462625, 5.185566697915457546, -0.6999999999999992895 ) ) ;
#12996 = CARTESIAN_POINT ( 'NONE',  ( 5.242919931573567283, -2.735361231296036699, -61.31790713612500099 ) ) ;
#12997 = ORIENTED_EDGE ( 'NONE', *, *, #8643, .F. ) ;
#12998 = CARTESIAN_POINT ( 'NONE',  ( 18.43657771686843816, 20.00006074167432857, 230.6521199318109154 ) ) ;
#12999 = VERTEX_POINT ( 'NONE', #6246 ) ;
#13001 = CARTESIAN_POINT ( 'NONE',  ( 23.01145998759524858, -19.60693125301565232, 0.08279965200003180925 ) ) ;
#13000 = AXIS2_PLACEMENT_3D ( 'NONE', #27483, #29700, #11134 ) ;
#13002 = EDGE_LOOP ( 'NONE', ( #9322, #12608, #18918, #29972 ) ) ;
#13003 = DIRECTION ( 'NONE',  ( 0.9690327085511358796, -0.2219413702090850260, 0.1082480390019309596 ) ) ;
#13004 = EDGE_CURVE ( 'NONE', #29282, #8301, #8120, .T. ) ;
#13005 = CARTESIAN_POINT ( 'NONE',  ( -12.29999999996208437, -25.15635984007525749, -30.79900052739454708 ) ) ;
#13006 = CYLINDRICAL_SURFACE ( 'NONE', #9404, 10.00000000000000355 ) ;
#13007 = DIRECTION ( 'NONE',  ( -0.7071067811865466846, -1.595945597898659700E-12, -0.7071067811865484609 ) ) ;
#13008 = CARTESIAN_POINT ( 'NONE',  ( 25.35851007746311581, -13.00862288856444238, 5.680831396999986183 ) ) ;
#13009 = FACE_OUTER_BOUND ( 'NONE', #30295, .T. ) ;
#13010 = EDGE_LOOP ( 'NONE', ( #29599, #3162, #26936, #5747 ) ) ;
#13011 = CARTESIAN_POINT ( 'NONE',  ( 1.995566471097224959, -3.675172130346584964, -44.10000000002499121 ) ) ;
#13012 = DIRECTION ( 'NONE',  ( 1.331100139797737888E-15, 1.000000000000000000, 0.000000000000000000 ) ) ;
#13013 = AXIS2_PLACEMENT_3D ( 'NONE', #28263, #4355, #11285 ) ;
#13014 = CARTESIAN_POINT ( 'NONE',  ( -2.258375515285932167, 5.046176096966566327, -23.73780126170000315 ) ) ;
#13015 = CARTESIAN_POINT ( 'NONE',  ( 23.64677485494184950, -12.61282738993112140, 4.366512952121566649 ) ) ;
#13016 = DIRECTION ( 'NONE',  ( 0.000000000000000000, -0.3420201433259318913, 0.9396926207858126157 ) ) ;
#13017 = DIRECTION ( 'NONE',  ( -9.220055274816719609E-13, -0.9128796883888953273, 0.4082287037029531662 ) ) ;
#13018 = CARTESIAN_POINT ( 'NONE',  ( 4.315256771988541296, 1.538274589489400990, -45.52627377572500933 ) ) ;
#13019 = AXIS2_PLACEMENT_3D ( 'NONE', #28688, #5386, #24592 ) ;
#13020 = CARTESIAN_POINT ( 'NONE',  ( 3.466821295769682159E-14, -2.890242878314739659E-13, 231.6412452697749984 ) ) ;
#13021 = CARTESIAN_POINT ( 'NONE',  ( 8.730899654840385438, -25.33966640892203159, 206.0387695587929215 ) ) ;
#13022 = CARTESIAN_POINT ( 'NONE',  ( -10.69999999999999929, -27.00000000000000000, -25.39999999999999858 ) ) ;
#13023 = CARTESIAN_POINT ( 'NONE',  ( -20.77057278543776420, -16.95162108973865855, 43.21714158846112497 ) ) ;
#13024 = CIRCLE ( 'NONE', #25604, 1.119823175164191165 ) ;
#13025 = CARTESIAN_POINT ( 'NONE',  ( 9.251510797979356937, -25.15273151106422844, 25.14734585054994653 ) ) ;
#13026 = ORIENTED_EDGE ( 'NONE', *, *, #25405, .F. ) ;
#13027 = CARTESIAN_POINT ( 'NONE',  ( 2.831388952324535691, -5.386915550550475551, -33.20721934060000535 ) ) ;
#13028 = ORIENTED_EDGE ( 'NONE', *, *, #10851, .T. ) ;
#13029 = CYLINDRICAL_SURFACE ( 'NONE', #18303, 3.000000000000001776 ) ;
#13030 = CARTESIAN_POINT ( 'NONE',  ( -5.044271480141131470, 2.992596682328089841, -51.63267869292499768 ) ) ;
#13031 = EDGE_LOOP ( 'NONE', ( #26677, #19276, #7608, #17656, #30695 ) ) ;
#13032 = ORIENTED_EDGE ( 'NONE', *, *, #106, .F. ) ;
#13033 = EDGE_CURVE ( 'NONE', #5307, #21098, #15522, .T. ) ;
#13034 =( NAMED_UNIT ( * ) SI_UNIT ( $, .STERADIAN. ) SOLID_ANGLE_UNIT ( ) );
#13035 = ORIENTED_EDGE ( 'NONE', *, *, #23125, .T. ) ;
#13036 = ORIENTED_EDGE ( 'NONE', *, *, #3135, .F. ) ;
#13037 = CARTESIAN_POINT ( 'NONE',  ( 24.54452541844319668, 14.48555669908156851, 3.920144559000027229 ) ) ;
#13038 = ADVANCED_FACE ( 'NONE', ( #13158 ), #5772, .F. ) ;
#13039 = CARTESIAN_POINT ( 'NONE',  ( -0.4442473836104618434, -27.79664838810757743, 5.558326393341954663 ) ) ;
#13040 = CARTESIAN_POINT ( 'NONE',  ( 2.506562108457635940, 4.370859049088616111, -35.69999999999999574 ) ) ;
#13041 = VECTOR ( 'NONE', #642, 1000.000000000000000 ) ;
#13042 = CARTESIAN_POINT ( 'NONE',  ( 25.41516571979999739, -14.56554165020000013, 222.0000000000000000 ) ) ;
#13043 = CARTESIAN_POINT ( 'NONE',  ( -12.41345480022817860, -28.31353721119876354, -23.38510924739736652 ) ) ;
#13044 = CARTESIAN_POINT ( 'NONE',  ( -3.813730490650353744, 1.734508981506462710, -0.6999999999999992895 ) ) ;
#13045 = CARTESIAN_POINT ( 'NONE',  ( 0.7444716670016126026, -5.443307122690507427, 0.6268759519999975716 ) ) ;
#13046 = CARTESIAN_POINT ( 'NONE',  ( -3.072394438959999974, -1.678456730820000020, 227.6468472915199754 ) ) ;
#13047 = CARTESIAN_POINT ( 'NONE',  ( -26.80000000069999899, 3.281945028329999726E-15, 93.21714158910000947 ) ) ;
#13048 = CARTESIAN_POINT ( 'NONE',  ( 2.536150288113637963, -3.576595042060325635, -12.12388893670000201 ) ) ;
#13049 = CARTESIAN_POINT ( 'NONE',  ( 4.904813032679735230, 3.691647504909488564, -32.36032172560000930 ) ) ;
#13050 = FACE_OUTER_BOUND ( 'NONE', #25129, .T. ) ;
#13051 = EDGE_CURVE ( 'NONE', #26103, #25785, #3256, .T. ) ;
#13052 = DIRECTION ( 'NONE',  ( 0.000000000000000000, 0.000000000000000000, 1.000000000000000000 ) ) ;
#13053 = CARTESIAN_POINT ( 'NONE',  ( -25.77914833258148164, -15.40383343755785361, 1.000000000000000888 ) ) ;
#13054 = CARTESIAN_POINT ( 'NONE',  ( -7.872160508897946052, -115.3203316365707849, 21.50869821882927724 ) ) ;
#13055 = FACE_OUTER_BOUND ( 'NONE', #5383, .T. ) ;
#13056 = CARTESIAN_POINT ( 'NONE',  ( 20.30405755279999980, 20.00000000000000000, 229.0000000000000000 ) ) ;
#13057 = FACE_OUTER_BOUND ( 'NONE', #28068, .T. ) ;
#13058 = CARTESIAN_POINT ( 'NONE',  ( -17.49999999969999820, -27.00000000000002487, -22.62649730830000294 ) ) ;
#13059 = ORIENTED_EDGE ( 'NONE', *, *, #20977, .T. ) ;
#13060 = ORIENTED_EDGE ( 'NONE', *, *, #14494, .F. ) ;
#13061 = VECTOR ( 'NONE', #1899, 1000.000000000000000 ) ;
#13062 = LINE ( 'NONE', #27537, #21813 ) ;
#13063 = LINE ( 'NONE', #3311, #29320 ) ;
#13064 = ORIENTED_EDGE ( 'NONE', *, *, #21142, .F. ) ;
#13065 = CYLINDRICAL_SURFACE ( 'NONE', #9289, 1.000000000000001332 ) ;
#13066 = DIRECTION ( 'NONE',  ( 1.000000000000000000, 0.000000000000000000, 0.000000000000000000 ) ) ;
#13067 = ORIENTED_EDGE ( 'NONE', *, *, #22554, .T. ) ;
#13068 = CARTESIAN_POINT ( 'NONE',  ( -8.982833346883255743, -25.99322455654492359, 23.95590625169068133 ) ) ;
#13069 = EDGE_LOOP ( 'NONE', ( #12307, #16701, #8251, #9335 ) ) ;
#13070 = EDGE_LOOP ( 'NONE', ( #5865, #11041, #1834, #10766 ) ) ;
#13071 = ORIENTED_EDGE ( 'NONE', *, *, #29887, .T. ) ;
#13072 = DIRECTION ( 'NONE',  ( -1.000000000000000000, 5.665498452320000818E-16, 0.000000000000000000 ) ) ;
#13073 = CARTESIAN_POINT ( 'NONE',  ( -17.32507820271158039, -31.06130891780428271, -31.82860708177667064 ) ) ;
#13074 = FACE_OUTER_BOUND ( 'NONE', #10074, .T. ) ;
#13075 = VERTEX_POINT ( 'NONE', #23093 ) ;
#13076 = ADVANCED_FACE ( 'NONE', ( #1534 ), #22463, .F. ) ;
#13077 = DIRECTION ( 'NONE',  ( 1.000000000000000000, -1.843431230198065828E-12, 2.650498504953516580E-12 ) ) ;
#13078 = DIRECTION ( 'NONE',  ( 0.000000000000000000, 0.3420201433259318913, -0.9396926207858126157 ) ) ;
#13079 = DIRECTION ( 'NONE',  ( 0.000000000000000000, -1.000000000000000000, 0.000000000000000000 ) ) ;
#13080 = ORIENTED_EDGE ( 'NONE', *, *, #19559, .T. ) ;
#13081 = CARTESIAN_POINT ( 'NONE',  ( -3.510061880997908279, 5.032561185093348044, -2.227651354100003367 ) ) ;
#13082 = CARTESIAN_POINT ( 'NONE',  ( -2.879958020435939847, 3.829670441253783864, -18.69314294429999634 ) ) ;
#13083 = CARTESIAN_POINT ( 'NONE',  ( -17.62526668104891314, 11.76353838341477953, -0.6999999989999727834 ) ) ;
#13084 = CARTESIAN_POINT ( 'NONE',  ( -8.699999999703575071, -29.66205794074117819, -29.83816939507471133 ) ) ;
#13085 = CARTESIAN_POINT ( 'NONE',  ( 25.00924755590000004, -13.66774366000000107, 224.0987054560000047 ) ) ;
#13086 = ADVANCED_FACE ( 'NONE', ( #13009 ), #14266, .T. ) ;
#13087 = CARTESIAN_POINT ( 'NONE',  ( -26.07942841480000240, 9.118861015040000240, 230.6999999999999886 ) ) ;
#13088 = DIRECTION ( 'NONE',  ( -0.3633921898465291567, -0.9316362575375348731, 0.000000000000000000 ) ) ;
#13089 = VECTOR ( 'NONE', #13932, 1000.000000000000000 ) ;
#13091 = DIRECTION ( 'NONE',  ( -0.9316362575375349842, 0.3633921898465292122, -0.000000000000000000 ) ) ;
#13090 = B_SPLINE_CURVE_WITH_KNOTS ( 'NONE', 1,
 ( #732, #7635 ),
 .UNSPECIFIED., .F., .F.,
 ( 2, 2 ),
 ( -3.500000000000000000, 3.500000000000000000 ),
 .UNSPECIFIED. ) ;
#13092 = EDGE_CURVE ( 'NONE', #6267, #9824, #26018, .T. ) ;
#13093 = CARTESIAN_POINT ( 'NONE',  ( 23.15117696689999960, -13.85641134509999972, 230.6999999999999886 ) ) ;
#13094 = CARTESIAN_POINT ( 'NONE',  ( 3.217281813909021349, -2.884757478452711688, -39.40998476019758812 ) ) ;
#13095 = ORIENTED_EDGE ( 'NONE', *, *, #21350, .T. ) ;
#13096 = CARTESIAN_POINT ( 'NONE',  ( 5.506968775199813315, -0.09733528975458538568, -57.29793411332500597 ) ) ;
#13097 = DIRECTION ( 'NONE',  ( 4.428977494234582379E-12, 0.8987940462991651502, -0.4383711467890810676 ) ) ;
#13098 = EDGE_CURVE ( 'NONE', #12806, #16634, #15865, .T. ) ;
#13099 = ORIENTED_EDGE ( 'NONE', *, *, #18735, .T. ) ;
#13100 = CARTESIAN_POINT ( 'NONE',  ( -26.25085564088219670, 8.872172082313914743, 0.02487529700001545052 ) ) ;
#13101 = CARTESIAN_POINT ( 'NONE',  ( -4.220714658002963304, 0.7024586621993844648, -68.10000000002501963 ) ) ;
#13102 = ORIENTED_EDGE ( 'NONE', *, *, #23764, .T. ) ;
#13103 = B_SPLINE_CURVE_WITH_KNOTS ( 'NONE', 3,
 ( #20679, #13749, #13274, #22886, #1329, #18621 ),
 .UNSPECIFIED., .F., .F.,
 ( 4, 2, 4 ),
 ( 0.000000000000000000, 0.5000000000000000000, 1.000000000000000000 ),
 .UNSPECIFIED. ) ;
#13104 = ORIENTED_EDGE ( 'NONE', *, *, #6563, .F. ) ;
#13105 = ORIENTED_EDGE ( 'NONE', *, *, #11389, .F. ) ;
#13106 = CARTESIAN_POINT ( 'NONE',  ( 3.534974566707796306, 0.6525538654836177122, -91.50574204942923018 ) ) ;
#13107 = ORIENTED_EDGE ( 'NONE', *, *, #25408, .T. ) ;
#13108 = CARTESIAN_POINT ( 'NONE',  ( -24.92013865347427171, 13.82966157970119525, 3.899998581000013509 ) ) ;
#13109 = ADVANCED_FACE ( 'NONE', ( #6398 ), #26074, .F. ) ;
#13110 = DIRECTION ( 'NONE',  ( 0.000000000000000000, 0.000000000000000000, -1.000000000000000000 ) ) ;
#13111 = CARTESIAN_POINT ( 'NONE',  ( 3.609030021535462041, -4.129188278801706247, -63.69605006312499995 ) ) ;
#13112 = CARTESIAN_POINT ( 'NONE',  ( 1.407377285053368787, -28.46552657486722637, 5.679668080906079553 ) ) ;
#13113 = ADVANCED_FACE ( 'NONE', ( #25764 ), #25588, .T. ) ;
#13114 = AXIS2_PLACEMENT_3D ( 'NONE', #18438, #25693, #2081 ) ;
#13115 = CARTESIAN_POINT ( 'NONE',  ( -24.05392374927932053, 13.13253365033636477, -0.6999999999999784173 ) ) ;
#13116 = CARTESIAN_POINT ( 'NONE',  ( 0.000000000000000000, -1.776356839399999804E-15, 227.6412452697800006 ) ) ;
#13117 =( NAMED_UNIT ( * ) SI_UNIT ( $, .STERADIAN. ) SOLID_ANGLE_UNIT ( ) );
#13118 = ADVANCED_FACE ( 'NONE', ( #4042 ), #1842, .F. ) ;
#13119 = CARTESIAN_POINT ( 'NONE',  ( -24.97129468253034545, 13.73710443232325495, 3.901342130000013064 ) ) ;
#13120 = VERTEX_POINT ( 'NONE', #18662 ) ;
#13121 = CARTESIAN_POINT ( 'NONE',  ( -5.530047734074942767, 3.478668956039820959, -10.44547590279999660 ) ) ;
#13122 = CARTESIAN_POINT ( 'NONE',  ( -3.982632971385690279, -21.02717377734789039, -30.56133709589786207 ) ) ;
#13123 = CARTESIAN_POINT ( 'NONE',  ( 14.78339330455285960, -30.42684276135835830, -32.19501410105780081 ) ) ;
#13124 = ORIENTED_EDGE ( 'NONE', *, *, #17384, .T. ) ;
#13125 = CARTESIAN_POINT ( 'NONE',  ( 24.58943550720000104, -12.96928235400000062, 224.6894611300000122 ) ) ;
#13126 = CARTESIAN_POINT ( 'NONE',  ( 16.37473331892315542, -8.236461616552139375, -0.6999999999999784173 ) ) ;
#13127 = CARTESIAN_POINT ( 'NONE',  ( 21.16705260759999874, -21.30254494060000070, 229.0000000000000000 ) ) ;
#13128 = B_SPLINE_CURVE_WITH_KNOTS ( 'NONE', 3,
 ( #27859, #6142, #27543, #27393, #975, #10565, #20622, #24888, #17629, #6308, #8335, #5988, #25037, #8182, #22830, #13068, #15582, #24727, #3467, #25189, #11033, #3161, #29910, #10878 ),
 .UNSPECIFIED., .F., .F.,
 ( 4, 2, 2, 2, 2, 2, 2, 2, 2, 2, 2, 4 ),
 ( 8.673617379884035472E-19, 0.001576261392767898308, 0.002364392089151846378, 0.003152522785535794448, 0.004728784178303689287, 0.005516914874687638658, 0.006305045571071588896, 0.007881306963839485036, 0.009457568356607382043, 0.01024569905299133402, 0.01103382974937528599, 0.01261009114214319340 ),
 .UNSPECIFIED. ) ;
#13129 = CARTESIAN_POINT ( 'NONE',  ( 21.90431914205521124, 17.68079901892130579, 0.7069222299999899928 ) ) ;
#13130 = CARTESIAN_POINT ( 'NONE',  ( 1.482055586095336386, -0.2313249656297586831, 231.6412452697749984 ) ) ;
#13131 = CARTESIAN_POINT ( 'NONE',  ( 4.332295931058598448, 4.388630459628991787, -57.70805965152499795 ) ) ;
#13132 = CARTESIAN_POINT ( 'NONE',  ( -12.47330046629999956, 20.99999999999999645, -55.90292611659999977 ) ) ;
#13133 = CARTESIAN_POINT ( 'NONE',  ( 27.63177371740000154, -3.383804566150000094E-15, 142.6394760449999808 ) ) ;
#13134 = ORIENTED_EDGE ( 'NONE', *, *, #9548, .F. ) ;
#13135 = CARTESIAN_POINT ( 'NONE',  ( -10.69999999997517115, -27.39453140544401322, -31.40000000000000568 ) ) ;
#13136 = CARTESIAN_POINT ( 'NONE',  ( 19.80538173169999894, 19.50875421069999760, 227.5999999999999943 ) ) ;
#13137 = VECTOR ( 'NONE', #17616, 999.9999999999998863 ) ;
#13138 = B_SPLINE_CURVE_WITH_KNOTS ( 'NONE', 1,
 ( #6281, #13515 ),
 .UNSPECIFIED., .F., .F.,
 ( 2, 2 ),
 ( -2.556331299420000144E-06, 0.7000000000009999335 ),
 .UNSPECIFIED. ) ;
#13139 = CARTESIAN_POINT ( 'NONE',  ( 0.03635086293632015797, -28.50041301604635180, 6.002517553000020101 ) ) ;
#13140 = CARTESIAN_POINT ( 'NONE',  ( 8.999999999770000869, 21.70000000000000284, -45.10000000000000142 ) ) ;
#13141 = CARTESIAN_POINT ( 'NONE',  ( 7.973778855661143083, -5.874736698510242938, -27.70229359854242190 ) ) ;
#13142 = CARTESIAN_POINT ( 'NONE',  ( -10.99289321870000080, -24.65831413349999934, -1.692893218799999877 ) ) ;
#13143 = ADVANCED_FACE ( 'NONE', ( #14111 ), #7496, .T. ) ;
#13144 = CARTESIAN_POINT ( 'NONE',  ( -4.543473910928012671, 0.02303893552233621245, -62.57122063472500884 ) ) ;
#13145 = ORIENTED_EDGE ( 'NONE', *, *, #4647, .F. ) ;
#13146 = CARTESIAN_POINT ( 'NONE',  ( 20.30405755279999980, 20.00000000000000000, 229.0000000000000000 ) ) ;
#13147 = EDGE_CURVE ( 'NONE', #8037, #14716, #30925, .T. ) ;
#13148 = ORIENTED_EDGE ( 'NONE', *, *, #22641, .T. ) ;
#13149 = EDGE_CURVE ( 'NONE', #7951, #4165, #18872, .T. ) ;
#13150 = CARTESIAN_POINT ( 'NONE',  ( 27.77052805885498898, 0.5052956280874429940, 0.7069222069999991920 ) ) ;
#13151 = ADVANCED_FACE ( 'NONE', ( #18974 ), #8910, .F. ) ;
#13152 = VERTEX_POINT ( 'NONE', #16149 ) ;
#13153 = CARTESIAN_POINT ( 'NONE',  ( 16.86019302162820921, 12.06576768788192489, -0.6999999999999785283 ) ) ;
#13154 = CARTESIAN_POINT ( 'NONE',  ( 25.25401215818320821, -13.21081861402980273, 4.098596794000014754 ) ) ;
#13155 = CYLINDRICAL_SURFACE ( 'NONE', #6911, 3.000000000000003997 ) ;
#13156 = CARTESIAN_POINT ( 'NONE',  ( -17.44301831181765650, -23.68168661394991759, -32.25767356540747244 ) ) ;
#13157 = DIRECTION ( 'NONE',  ( -2.415891560877031462E-12, 0.9341647027306021478, 0.3568421334038983650 ) ) ;
#13158 = FACE_OUTER_BOUND ( 'NONE', #20162, .T. ) ;
#13159 = VERTEX_POINT ( 'NONE', #11439 ) ;
#13160 = CARTESIAN_POINT ( 'NONE',  ( -14.60916135985672071, 28.04296594682689658, 1.000000000000000888 ) ) ;
#13161 = CARTESIAN_POINT ( 'NONE',  ( -8.699999999707589637, -24.26136093481122558, -29.62468611113576955 ) ) ;
#13162 = LINE ( 'NONE', #6404, #20796 ) ;
#13163 = CARTESIAN_POINT ( 'NONE',  ( 1.265035515811502309, -4.453021097817297047, -21.29535708919999593 ) ) ;
#13164 = DIRECTION ( 'NONE',  ( -0.000000000000000000, -0.000000000000000000, -1.000000000000000000 ) ) ;
#13165 = LINE ( 'NONE', #10512, #5967 ) ;
#13166 = CARTESIAN_POINT ( 'NONE',  ( 21.30888436558567633, -16.34772642260384856, 86.78285841148333191 ) ) ;
#13167 = CARTESIAN_POINT ( 'NONE',  ( 0.6677280494740716055, -27.79235729091802654, 224.1133967326756249 ) ) ;
#13168 = CARTESIAN_POINT ( 'NONE',  ( 3.650437977654107602, 3.794428519304413605, -47.94426496242498814 ) ) ;
#13169 = CARTESIAN_POINT ( 'NONE',  ( -17.41133668179312721, 11.94697101933574324, -1.400000000000001688 ) ) ;
#13170 = CARTESIAN_POINT ( 'NONE',  ( -11.69999999989999928, -25.00000000000000000, -1.399999999999998579 ) ) ;
#13171 = CARTESIAN_POINT ( 'NONE',  ( -19.40755098202004802, 19.99999817177441841, 230.3222639546364405 ) ) ;
#13172 = DIRECTION ( 'NONE',  ( -1.000000000000000000, 0.000000000000000000, -6.771000000000000128E-12 ) ) ;
#13173 = CONICAL_SURFACE ( 'NONE', #9664, 0.9999999999991022737, 0.7853981633970000820 ) ;
#13174 = CARTESIAN_POINT ( 'NONE',  ( 6.760007715859396527, 4.357143524031256376, -42.94209588227683128 ) ) ;
#13175 = EDGE_LOOP ( 'NONE', ( #14187, #4216, #23524, #524 ) ) ;
#13176 = CARTESIAN_POINT ( 'NONE',  ( -0.4155902256269943806, 5.929468065910143082, -35.89518930509999706 ) ) ;
#13177 = ORIENTED_EDGE ( 'NONE', *, *, #28804, .T. ) ;
#13178 = CARTESIAN_POINT ( 'NONE',  ( 18.95046173579999760, -18.95046173579999760, 115.0000000000000000 ) ) ;
#13179 = CARTESIAN_POINT ( 'NONE',  ( 5.066518387468507356, -3.138291312573631586, -49.81324460762500195 ) ) ;
#13180 = VERTEX_POINT ( 'NONE', #4513 ) ;
#13181 = APPLICATION_PROTOCOL_DEFINITION ( 'draft international standard', 'automotive_design', 1998, #16418 ) ;
#13182 = VERTEX_POINT ( 'NONE', #21041 ) ;
#13183 =( REPRESENTATION_RELATIONSHIP ('NONE','NONE', #2712, #6935 ) REPRESENTATION_RELATIONSHIP_WITH_TRANSFORMATION ( #14135 )SHAPE_REPRESENTATION_RELATIONSHIP( ) );
#13184 = ORIENTED_EDGE ( 'NONE', *, *, #30800, .F. ) ;
#13185 = LINE ( 'NONE', #15103, #9744 ) ;
#13186 = DIRECTION ( 'NONE',  ( 1.595945597898660305E-12, 0.7071067811865475727, -0.7071067811865475727 ) ) ;
#13187 = DIRECTION ( 'NONE',  ( 2.764840495839172918E-12, 0.9128796883888953273, -0.4082287037029530552 ) ) ;
#13188 = CARTESIAN_POINT ( 'NONE',  ( -6.661312627754254478, -7.245008774417666331, -33.94554228739334434 ) ) ;
#13189 = CARTESIAN_POINT ( 'NONE',  ( -16.29518228631965826, -8.030294604068396680, -0.6999999999999785283 ) ) ;
#13190 = CARTESIAN_POINT ( 'NONE',  ( -3.788551368745695314, 2.416708791688973790, -0.6999999999999992895 ) ) ;
#13191 = CARTESIAN_POINT ( 'NONE',  ( 4.360957369889326252, -0.1505632777267507105, -2.685409721200002320 ) ) ;
#13192 = VECTOR ( 'NONE', #29044, 1000.000000000000114 ) ;
#13193 = CARTESIAN_POINT ( 'NONE',  ( -8.000000000040557779, -116.5561065465021784, 18.74526241810166027 ) ) ;
#13194 = CARTESIAN_POINT ( 'NONE',  ( 24.49999999589999788, -3.000285566359999846E-15, 140.0000000000000000 ) ) ;
#13195 = EDGE_LOOP ( 'NONE', ( #487, #17481, #4029, #27051 ) ) ;
#13196 = CARTESIAN_POINT ( 'NONE',  ( -5.517889265940039145, -2.627421812126006451, -13.57655742009999855 ) ) ;
#13197 = CARTESIAN_POINT ( 'NONE',  ( -2.308365619037861638, -4.044857084274060988, -30.17642233980000910 ) ) ;
#13198 = CARTESIAN_POINT ( 'NONE',  ( 17.18658402238548533, 9.900182044515950963, -1.000005633855494125E-09 ) ) ;
#13199 = EDGE_CURVE ( 'NONE', #1607, #23118, #30641, .T. ) ;
#13200 = PLANE ( 'NONE',  #25365 ) ;
#13201 = SURFACE_STYLE_USAGE ( .BOTH. , #808 ) ;
#13202 = DIRECTION ( 'NONE',  ( -0.7198537139083028835, 0.6941258031311204890, 0.000000000000000000 ) ) ;
#13203 = CARTESIAN_POINT ( 'NONE',  ( -4.346598770676703083, -0.007247149673123010061, -28.16856466009999593 ) ) ;
#13204 = CARTESIAN_POINT ( 'NONE',  ( 17.83931306984926835, 20.00000000000176570, -0.6999999999999784173 ) ) ;
#13205 = CARTESIAN_POINT ( 'NONE',  ( -9.414213562409999625, -15.31419272936388687, -74.45223986426802298 ) ) ;
#13206 = CARTESIAN_POINT ( 'NONE',  ( 21.28666574344908469, 18.00484885041732142, 1.000000000000000888 ) ) ;
#13207 = ORIENTED_EDGE ( 'NONE', *, *, #19248, .F. ) ;
#13209 = EDGE_CURVE ( 'NONE', #9398, #22920, #28582, .T. ) ;
#13208 = CIRCLE ( 'NONE', #13292, 3.491271820589999741 ) ;
#13210 = CARTESIAN_POINT ( 'NONE',  ( 23.57322167201318663, 14.73624931494496693, 6.002747145999992817 ) ) ;
#13211 = CARTESIAN_POINT ( 'NONE',  ( 2.656431219450670067, 2.398832595345626650, 230.7906780664011706 ) ) ;
#13212 = ORIENTED_EDGE ( 'NONE', *, *, #22467, .F. ) ;
#13213 =( GEOMETRIC_REPRESENTATION_CONTEXT ( 3 ) GLOBAL_UNCERTAINTY_ASSIGNED_CONTEXT ( ( #12504 ) ) GLOBAL_UNIT_ASSIGNED_CONTEXT ( ( #5904, #3547, #24803 ) ) REPRESENTATION_CONTEXT ( 'NONE', 'WORKASPACE' ) );
#13214 = CARTESIAN_POINT ( 'NONE',  ( 0.000000000000000000, 0.000000000000000000, 140.0000000000000000 ) ) ;
#13215 = DIRECTION ( 'NONE',  ( 0.000000000000000000, -1.000000000000000000, 2.257145581549999994E-12 ) ) ;
#13217 = ORIENTED_EDGE ( 'NONE', *, *, #24259, .F. ) ;
#13216 = AXIS2_PLACEMENT_3D ( 'NONE', #16200, #2204, #11942 ) ;
#13218 = DIRECTION ( 'NONE',  ( 0.000000000000000000, 0.000000000000000000, -1.000000000000000000 ) ) ;
#13219 = ORIENTED_EDGE ( 'NONE', *, *, #17643, .T. ) ;
#13220 = EDGE_LOOP ( 'NONE', ( #22330, #5764, #25581, #1716 ) ) ;
#13221 = ORIENTED_EDGE ( 'NONE', *, *, #3522, .T. ) ;
#13222 = CARTESIAN_POINT ( 'NONE',  ( 16.40303402077768169, -9.791839085275103827, 0.000000000000000000 ) ) ;
#13223 = CARTESIAN_POINT ( 'NONE',  ( 0.000000000000000000, 0.000000000000000000, 20.00000000000000000 ) ) ;
#13224 = CARTESIAN_POINT ( 'NONE',  ( -9.999999999959999997, -24.87868334570000073, -26.27868334529999927 ) ) ;
#13225 = FACE_OUTER_BOUND ( 'NONE', #23589, .T. ) ;
#13226 = CARTESIAN_POINT ( 'NONE',  ( -24.37450209798932477, 13.36961646417070249, 6.095967861000000987 ) ) ;
#13227 = CARTESIAN_POINT ( 'NONE',  ( 2.993135038577686036, -3.518891676577371896, -95.36817406306990108 ) ) ;
#13228 = ORIENTED_EDGE ( 'NONE', *, *, #13252, .T. ) ;
#13229 = DIRECTION ( 'NONE',  ( 0.000000000000000000, 0.000000000000000000, 1.000000000000000000 ) ) ;
#13230 = CARTESIAN_POINT ( 'NONE',  ( -20.19490051663601093, -17.70600380938601148, 0.000000000000000000 ) ) ;
#13231 = EDGE_CURVE ( 'NONE', #18256, #13982, #1961, .T. ) ;
#13232 = CARTESIAN_POINT ( 'NONE',  ( -0.07056952541309999272, -28.50017087330000010, 226.0986539140000104 ) ) ;
#13233 = AXIS2_PLACEMENT_3D ( 'NONE', #6484, #18442, #30722 ) ;
#13234 = CARTESIAN_POINT ( 'NONE',  ( 2.223383862040885450, -3.430296892840217993, -0.1659393883000001568 ) ) ;
#13235 = CARTESIAN_POINT ( 'NONE',  ( -3.679974273075534708, -2.251605409995533602, -21.40799200640000066 ) ) ;
#13236 = CIRCLE ( 'NONE', #27330, 26.80000000000000071 ) ;
#13237 = CARTESIAN_POINT ( 'NONE',  ( -10.69999999999999929, -130.0000000000000000, -22.39999999999999858 ) ) ;
#13238 = CARTESIAN_POINT ( 'NONE',  ( -1.100000000000000089, -27.47799119230000287, 5.000000000000000000 ) ) ;
#13239 = CARTESIAN_POINT ( 'NONE',  ( 0.5772249557075271875, -3.431781221450775909, -90.29857220542305640 ) ) ;
#13240 = CARTESIAN_POINT ( 'NONE',  ( -26.80000000000000071, -7.731961996110000454E-14, 230.6999999999999886 ) ) ;
#13241 = CARTESIAN_POINT ( 'NONE',  ( 1.660040334269103246, -0.7942402406998696485, -97.85464525912325939 ) ) ;
#13242 = CARTESIAN_POINT ( 'NONE',  ( -23.32129337769715960, -14.57293380285341655, 224.4438356449677485 ) ) ;
#13243 = B_SPLINE_CURVE_WITH_KNOTS ( 'NONE', 3,
 ( #7701, #7555, #10385, #29572, #5349, #22344, #15253, #29258, #796, #13043, #25006, #3440, #3290, #17145, #12895, #17455, #24400, #14954, #340, #646, #9923, #15106, #14801, #24552, #19523, #22045 ),
 .UNSPECIFIED., .F., .F.,
 ( 4, 2, 2, 1, 1, 2, 2, 2, 2, 2, 1, 1, 2, 2, 4 ),
 ( 0.000000000000000000, 0.1249999999999981959, 0.1874999999999982792, 0.2187499999999980016, 0.2343749999999985012, 0.2421874999999975575, 0.2499999999999966138, 0.4999999999999827915, 0.6249999999999750200, 0.6874999999999706901, 0.7187499999999685807, 0.7343749999999680256, 0.7421874999999686917, 0.7499999999999693578, 1.000000000000000000 ),
 .UNSPECIFIED. ) ;
#13244 = B_SPLINE_CURVE_WITH_KNOTS ( 'NONE', 1,
 ( #29270, #7711 ),
 .UNSPECIFIED., .F., .F.,
 ( 2, 2 ),
 ( -3.500000000000000000, 3.500000000000000000 ),
 .UNSPECIFIED. ) ;
#13245 = DIRECTION ( 'NONE',  ( 0.000000000000000000, 2.259525899719999991E-12, 1.000000000000000000 ) ) ;
#13246 = CARTESIAN_POINT ( 'NONE',  ( -26.80000000000000071, -8.704148513059999178E-14, 230.6999999999999886 ) ) ;
#13247 = CARTESIAN_POINT ( 'NONE',  ( -2.664535259099999568E-14, -26.80000000000000071, 210.0000000000000284 ) ) ;
#13248 = ORIENTED_EDGE ( 'NONE', *, *, #17338, .T. ) ;
#13249 = CARTESIAN_POINT ( 'NONE',  ( 3.312932182603870679, 3.356011527877057254, -57.30805965152501358 ) ) ;
#13250 = DIRECTION ( 'NONE',  ( -2.416122857340496113E-12, 0.9341647027306024809, 0.3568421334038978099 ) ) ;
#13251 = ORIENTED_EDGE ( 'NONE', *, *, #10955, .F. ) ;
#13252 = EDGE_CURVE ( 'NONE', #23341, #9577, #4658, .T. ) ;
#13253 = CARTESIAN_POINT ( 'NONE',  ( -3.283272085058491996, -5.616145207990252963, -15.68182079290000175 ) ) ;
#13254 = ORIENTED_EDGE ( 'NONE', *, *, #12491, .T. ) ;
#13255 = CARTESIAN_POINT ( 'NONE',  ( 26.93395402219999824, -3.298349122899999616E-15, 137.7567592739999895 ) ) ;
#13256 = DIRECTION ( 'NONE',  ( 1.000000000000000000, -0.000000000000000000, 0.000000000000000000 ) ) ;
#13257 = AXIS2_PLACEMENT_3D ( 'NONE', #3069, #15608, #5121 ) ;
#13258 = ORIENTED_EDGE ( 'NONE', *, *, #8017, .F. ) ;
#13259 =( NAMED_UNIT ( * ) SI_UNIT ( $, .STERADIAN. ) SOLID_ANGLE_UNIT ( ) );
#13260 = CIRCLE ( 'NONE', #24324, 4.000000000000000888 ) ;
#13261 = VERTEX_POINT ( 'NONE', #2312 ) ;
#13262 = AXIS2_PLACEMENT_3D ( 'NONE', #7831, #24984, #6091 ) ;
#13263 = VERTEX_POINT ( 'NONE', #11895 ) ;
#13264 = FACE_OUTER_BOUND ( 'NONE', #24495, .T. ) ;
#13265 =( NAMED_UNIT ( * ) SI_UNIT ( $, .STERADIAN. ) SOLID_ANGLE_UNIT ( ) );
#13266 = VECTOR ( 'NONE', #11899, 1000.000000000000114 ) ;
#13267 = ORIENTED_EDGE ( 'NONE', *, *, #4639, .T. ) ;
#13268 = CARTESIAN_POINT ( 'NONE',  ( 13.67718073920000066, 20.99999999999999645, -57.16242423349999768 ) ) ;
#13269 = CARTESIAN_POINT ( 'NONE',  ( 20.30405755279999980, 20.00000000000000000, 229.0000000000000000 ) ) ;
#13270 = EDGE_CURVE ( 'NONE', #26486, #2751, #24502, .T. ) ;
#13271 = CARTESIAN_POINT ( 'NONE',  ( -4.069925668896384963, 4.914984763948436530, -62.51933298482501300 ) ) ;
#13272 = CARTESIAN_POINT ( 'NONE',  ( -27.79999999970000246, -10.21376199200000201, 229.0000000000000000 ) ) ;
#13273 = EDGE_CURVE ( 'NONE', #27091, #17864, #26676, .T. ) ;
#13274 = CARTESIAN_POINT ( 'NONE',  ( -10.00000000021355362, -24.37864083493692746, -29.91085694111383120 ) ) ;
#13275 = CARTESIAN_POINT ( 'NONE',  ( 9.301654454730000410, 19.99999999999999645, -44.08327288285030221 ) ) ;
#13276 =( GEOMETRIC_REPRESENTATION_CONTEXT ( 3 ) GLOBAL_UNCERTAINTY_ASSIGNED_CONTEXT ( ( #7173 ) ) GLOBAL_UNIT_ASSIGNED_CONTEXT ( ( #3868, #23075, #23548 ) ) REPRESENTATION_CONTEXT ( 'NONE', 'WORKASPACE' ) );
#13277 = CARTESIAN_POINT ( 'NONE',  ( -17.48633009204635869, -24.20600253127152612, -24.23958570799475254 ) ) ;
#13278 = PLANE ( 'NONE',  #7944 ) ;
#13279 = ORIENTED_EDGE ( 'NONE', *, *, #17499, .T. ) ;
#13280 = ADVANCED_FACE ( 'NONE', ( #14579 ), #24019, .T. ) ;
#13281 = CARTESIAN_POINT ( 'NONE',  ( 1.348918213770415653, 4.124136235849971577, -11.07047964830000453 ) ) ;
#13282 = CARTESIAN_POINT ( 'NONE',  ( -3.907985046680000082E-14, -26.80000000000000071, 6.099999999630000502 ) ) ;
#13283 = AXIS2_PLACEMENT_3D ( 'NONE', #21743, #5206, #7270 ) ;
#13284 = FACE_OUTER_BOUND ( 'NONE', #202, .T. ) ;
#13285 = EDGE_LOOP ( 'NONE', ( #452, #2479, #14088, #9203 ) ) ;
#13286 = CARTESIAN_POINT ( 'NONE',  ( 24.91921101730000032, -13.83103916679999834, 223.9972514410000031 ) ) ;
#13287 = DIRECTION ( 'NONE',  ( 0.000000000000000000, -2.257157423930000049E-12, -1.000000000000000000 ) ) ;
#13288 = AXIS2_PLACEMENT_3D ( 'NONE', #20578, #11299, #6416 ) ;
#13289 = CARTESIAN_POINT ( 'NONE',  ( -20.30403093128963476, 20.00000000003735323, 3.000000106999994642 ) ) ;
#13290 = AXIS2_PLACEMENT_3D ( 'NONE', #2998, #15853, #18194 ) ;
#13291 = CARTESIAN_POINT ( 'NONE',  ( 24.71356588429571488, 13.94368305209927428, 1.000000000000000888 ) ) ;
#13292 = AXIS2_PLACEMENT_3D ( 'NONE', #12474, #26648, #23992 ) ;
#13293 = DIRECTION ( 'NONE',  ( -1.000000000000000000, 5.665498452320000818E-16, 0.000000000000000000 ) ) ;
#13294 = CARTESIAN_POINT ( 'NONE',  ( -0.6751951171170902377, 5.935132877048193478, -48.26410749642499809 ) ) ;
#13295 = ADVANCED_FACE ( 'NONE', ( #19445 ), #5115, .F. ) ;
#13296 = CARTESIAN_POINT ( 'NONE',  ( -11.51411769270000107, -24.20066399839999960, -0.7084723282999999538 ) ) ;
#13297 = CARTESIAN_POINT ( 'NONE',  ( 26.80000000069999899, -3.281945028320000125E-15, 186.7828584129999854 ) ) ;
#13298 = VERTEX_POINT ( 'NONE', #2767 ) ;
#13299 = CARTESIAN_POINT ( 'NONE',  ( 26.95545381250000361, 8.667969360469999884, 222.0000000000000000 ) ) ;
#13300 = B_SPLINE_CURVE_WITH_KNOTS ( 'NONE', 5,
 ( #6156, #6322, #13395, #3483, #22687, #3807 ),
 .UNSPECIFIED., .F., .F.,
 ( 6, 6 ),
 ( 0.000000000000000000, 2.319814964739999930 ),
 .UNSPECIFIED. ) ;
#13301 = CARTESIAN_POINT ( 'NONE',  ( 2.876615514287123254, -3.533536248196276652, -68.10000000002499121 ) ) ;
#13302 = AXIS2_PLACEMENT_3D ( 'NONE', #21219, #13672, #16644 ) ;
#13303 = EDGE_CURVE ( 'NONE', #979, #14446, #1466, .T. ) ;
#13304 = CARTESIAN_POINT ( 'NONE',  ( -10.82908725742656308, -27.76276047461853835, 43.21714158840000408 ) ) ;
#13305 = CARTESIAN_POINT ( 'NONE',  ( -4.237596627851885067, 0.8380315630058113863, -44.10000000002499121 ) ) ;
#13306 = FACE_OUTER_BOUND ( 'NONE', #6271, .T. ) ;
#13307 = CARTESIAN_POINT ( 'NONE',  ( -17.83928249680000278, 19.99999999999999645, -0.6999999999999992895 ) ) ;
#13308 = CARTESIAN_POINT ( 'NONE',  ( 5.384875807261761516, 2.601783486389667832, -66.85315453642499506 ) ) ;
#13309 = ORIENTED_EDGE ( 'NONE', *, *, #23688, .T. ) ;
#13310 = CARTESIAN_POINT ( 'NONE',  ( 19.42821516957057071, 19.99999712421914566, 230.3105388825946989 ) ) ;
#13311 = ORIENTED_EDGE ( 'NONE', *, *, #13554, .F. ) ;
#13312 = B_SPLINE_CURVE_WITH_KNOTS ( 'NONE', 1,
 ( #10553, #8020 ),
 .UNSPECIFIED., .F., .F.,
 ( 2, 2 ),
 ( -3.500000000000000000, 3.500000000000000000 ),
 .UNSPECIFIED. ) ;
#13313 = CARTESIAN_POINT ( 'NONE',  ( -19.63983047447944941, -20.49826324463772664, 0.000000000000000000 ) ) ;
#13314 = ORIENTED_EDGE ( 'NONE', *, *, #8898, .F. ) ;
#13315 = CARTESIAN_POINT ( 'NONE',  ( -23.81776757772072983, -15.65134804123479917, 4.895813258999987205 ) ) ;
#13316 = CARTESIAN_POINT ( 'NONE',  ( -23.20948082139999968, -13.40000000000000036, 6.099999999630000502 ) ) ;
#13317 = CARTESIAN_POINT ( 'NONE',  ( 1.108738578190967550, 3.350312884103880950, 0.000000000000000000 ) ) ;
#13318 = AXIS2_PLACEMENT_3D ( 'NONE', #3802, #1128, #1447 ) ;
#13319 = DIRECTION ( 'NONE',  ( 1.000000000000000000, 0.000000000000000000, 0.000000000000000000 ) ) ;
#13320 = CARTESIAN_POINT ( 'NONE',  ( -12.32027642597305039, -21.99999999999999645, -28.95335161925533640 ) ) ;
#13321 = CIRCLE ( 'NONE', #3275, 3.999999999669999973 ) ;
#13322 = AXIS2_PLACEMENT_3D ( 'NONE', #16524, #21415, #31005 ) ;
#13323 = LINE ( 'NONE', #29693, #6986 ) ;
#13324 = VERTEX_POINT ( 'NONE', #422 ) ;
#13325 = DIRECTION ( 'NONE',  ( 0.3642835349036590564, 4.461186650018491474E-17, -0.9312880897971875793 ) ) ;
#13326 = CARTESIAN_POINT ( 'NONE',  ( -8.699999999707452858, -24.10060434105348648, -29.26520274339392813 ) ) ;
#13327 = CARTESIAN_POINT ( 'NONE',  ( -7.355580493362803729, -15.96062638079863483, -74.68752247181846826 ) ) ;
#13328 = CARTESIAN_POINT ( 'NONE',  ( -17.87802153471533018, -8.632840205466846939, 0.000000000000000000 ) ) ;
#13329 = CARTESIAN_POINT ( 'NONE',  ( -24.34159889609999894, -14.82483853620000147, 225.9014025209999943 ) ) ;
#13330 = DIRECTION ( 'NONE',  ( 0.000000000000000000, 1.000000000000000000, 0.000000000000000000 ) ) ;
#13331 = ADVANCED_FACE ( 'NONE', ( #2915 ), #23072, .T. ) ;
#13332 = CARTESIAN_POINT ( 'NONE',  ( 9.999999999969999109, -24.87872937930000106, -30.52127062269999769 ) ) ;
#13333 = PLANE ( 'NONE',  #1065 ) ;
#13334 = CARTESIAN_POINT ( 'NONE',  ( 0.8648632234848976363, -6.342619565911398638, -49.76468436622499780 ) ) ;
#13335 = EDGE_CURVE ( 'NONE', #11684, #25785, #19757, .T. ) ;
#13336 = LINE ( 'NONE', #22630, #9705 ) ;
#13337 = PRODUCT_DEFINITION_SHAPE ( 'NONE', 'NONE',  #2325 ) ;
#13338 = EDGE_CURVE ( 'NONE', #21717, #5024, #12508, .T. ) ;
#13339 = CARTESIAN_POINT ( 'NONE',  ( 14.85086212533906469, -24.40458379250578247, -24.12496155405706588 ) ) ;
#13340 = CARTESIAN_POINT ( 'NONE',  ( 14.54973694814395913, -27.44328476931316274, -33.91757211090763491 ) ) ;
#13341 = LINE ( 'NONE', #22947, #28395 ) ;
#13342 = CARTESIAN_POINT ( 'NONE',  ( 3.664716979113602946, -26.54951320538905080, 20.19324488679039931 ) ) ;
#13343 = ORIENTED_EDGE ( 'NONE', *, *, #27570, .F. ) ;
#13344 = CARTESIAN_POINT ( 'NONE',  ( -4.976668802704899086, 3.592974922927941073, -34.46696136359999940 ) ) ;
#13345 = PRODUCT_DEFINITION_FORMATION_WITH_SPECIFIED_SOURCE ( 'ANY', '', #20959, .NOT_KNOWN. ) ;
#13346 = ORIENTED_EDGE ( 'NONE', *, *, #8892, .F. ) ;
#13347 = CARTESIAN_POINT ( 'NONE',  ( 1.321824945545745145, 4.319062652178982553, -51.46125421262499344 ) ) ;
#13348 = ORIENTED_EDGE ( 'NONE', *, *, #23730, .F. ) ;
#13349 = APPLICATION_PROTOCOL_DEFINITION ( 'draft international standard', 'automotive_design', 1998, #3128 ) ;
#13350 = ORIENTED_EDGE ( 'NONE', *, *, #20365, .F. ) ;
#13351 = VERTEX_POINT ( 'NONE', #3064 ) ;
#13352 = CARTESIAN_POINT ( 'NONE',  ( 23.83639842146205368, 14.30623132797946084, 3.899998581000013509 ) ) ;
#13353 = CARTESIAN_POINT ( 'NONE',  ( 17.18658402238548533, 9.900182044515950963, -1.000005633855494125E-09 ) ) ;
#13354 = DIRECTION ( 'NONE',  ( 1.000000000000000000, 0.000000000000000000, 0.000000000000000000 ) ) ;
#13355 = CARTESIAN_POINT ( 'NONE',  ( 27.79999999999999716, -2.355626804729999831E-11, 222.0000000000000000 ) ) ;
#13356 = FACE_OUTER_BOUND ( 'NONE', #31072, .T. ) ;
#13357 = DIRECTION ( 'NONE',  ( 0.000000000000000000, -0.8660254037843289066, 0.5000000000001899592 ) ) ;
#13358 = CARTESIAN_POINT ( 'NONE',  ( -0.7873752056533391830, -4.273814420472604070, -3.025234013000003497 ) ) ;
#13359 = CARTESIAN_POINT ( 'NONE',  ( -10.00000000009183942, -29.39900052719528389, -30.24364015992538057 ) ) ;
#13360 = CARTESIAN_POINT ( 'NONE',  ( 27.79999999990000248, 3.330083893049999855, 222.0000000000000000 ) ) ;
#13361 = ORIENTED_EDGE ( 'NONE', *, *, #503, .T. ) ;
#13362 = CARTESIAN_POINT ( 'NONE',  ( 5.466312515054250198, -2.792605348973308477, -12.51474735220000412 ) ) ;
#13363 = CARTESIAN_POINT ( 'NONE',  ( -4.434312336397093546, -3.917832084918029256, -32.83447003410000065 ) ) ;
#13364 = CARTESIAN_POINT ( 'NONE',  ( 4.288653532660000600, -4.054393014039999521, 226.6412452697800006 ) ) ;
#13365 = CARTESIAN_POINT ( 'NONE',  ( 19.18333294668393307, 19.99999946087643465, -0.4459674450000006285 ) ) ;
#13366 = CARTESIAN_POINT ( 'NONE',  ( 1.099998580829999906, -27.77839262550000043, 224.8959500220000223 ) ) ;
#13367 = CARTESIAN_POINT ( 'NONE',  ( -26.33250508584143290, -9.378843469325163440, 8.000000000000007105 ) ) ;
#13368 = CARTESIAN_POINT ( 'NONE',  ( -26.96951804470000269, 10.12763618690000023, 222.0000000000000000 ) ) ;
#13369 = EDGE_CURVE ( 'NONE', #2756, #20972, #12499, .T. ) ;
#13370 = B_SPLINE_CURVE_WITH_KNOTS ( 'NONE', 5,
 ( #7378, #17277, #29087, #24527, #26578, #26887, #5326, #26725, #10056, #22166, #773, #19183, #624, #17124, #26429 ),
 .UNSPECIFIED., .F., .F.,
 ( 6, 3, 3, 3, 6 ),
 ( 10.75845894650000112, 13.17160129120000001, 18.65982206369999830, 20.85462967400000167, 21.51695457350000140 ),
 .UNSPECIFIED. ) ;
#13371 = CARTESIAN_POINT ( 'NONE',  ( 18.97091132402077562, 21.26865671814604752, 1.000000000000000888 ) ) ;
#13372 = DIRECTION ( 'NONE',  ( 0.000000000000000000, 0.3420201433259318358, -0.9396926207858125046 ) ) ;
#13373 = FACE_OUTER_BOUND ( 'NONE', #6574, .T. ) ;
#13374 = EDGE_CURVE ( 'NONE', #24923, #13901, #576, .T. ) ;
#13375 = VERTEX_POINT ( 'NONE', #19137 ) ;
#13376 = DIRECTION ( 'NONE',  ( -1.000000000000000000, 2.082932338114093583E-15, -6.768115529734696084E-12 ) ) ;
#13377 = CARTESIAN_POINT ( 'NONE',  ( -133283.2432719999924, -454259.0741890000063, -160669.1380380000046 ) ) ;
#13378 = EDGE_LOOP ( 'NONE', ( #7870, #17324, #173, #23268 ) ) ;
#13379 = CARTESIAN_POINT ( 'NONE',  ( -22.68420274106557599, -14.27219891856329781, 224.5770195892032177 ) ) ;
#13380 = CARTESIAN_POINT ( 'NONE',  ( 4.000000000000000000, -31.15538618883996946, -82.34631830372681804 ) ) ;
#13381 = CARTESIAN_POINT ( 'NONE',  ( 1.087555312692434661, -26.77834283312493824, 4.781945490036553004 ) ) ;
#13382 = EDGE_LOOP ( 'NONE', ( #19660, #19584, #29804, #7503 ) ) ;
#13383 = DIRECTION ( 'NONE',  ( -5.550937487439999770E-18, 0.000000000000000000, -1.000000000000000000 ) ) ;
#13384 = VERTEX_POINT ( 'NONE', #26989 ) ;
#13385 = ORIENTED_EDGE ( 'NONE', *, *, #15472, .F. ) ;
#13386 = ORIENTED_EDGE ( 'NONE', *, *, #4297, .F. ) ;
#13387 = DIRECTION ( 'NONE',  ( 0.000000000000000000, -1.000000000000000000, 0.000000000000000000 ) ) ;
#13388 = ORIENTED_EDGE ( 'NONE', *, *, #19923, .F. ) ;
#13389 = CARTESIAN_POINT ( 'NONE',  ( 8.699999999559956620, -18.28443321520602183, -36.42483785839191768 ) ) ;
#13390 = DIRECTION ( 'NONE',  ( 1.000000000000000000, -0.000000000000000000, 0.000000000000000000 ) ) ;
#13391 = CARTESIAN_POINT ( 'NONE',  ( 3.746497173757565413, -0.1670055334890632737, -35.69999999999999574 ) ) ;
#13392 = CARTESIAN_POINT ( 'NONE',  ( 17.70297572270220243, -8.028915810492925687, -4.336808689942018722E-16 ) ) ;
#13393 = DIRECTION ( 'NONE',  ( 0.8090169943751909232, 0.5877852522921378498, 0.000000000000000000 ) ) ;
#13394 = CARTESIAN_POINT ( 'NONE',  ( 3.489276519439490798, -0.9563957866777589301, 227.7139869426456471 ) ) ;
#13395 = CARTESIAN_POINT ( 'NONE',  ( 26.93395402219999824, -3.298349122909999612E-15, 187.7567592740000180 ) ) ;
#13396 = EDGE_CURVE ( 'NONE', #5518, #23628, #18138, .T. ) ;
#13397 = B_SPLINE_CURVE_WITH_KNOTS ( 'NONE', 3,
 ( #27560, #15453, #3332, #26955, #8354, #7746 ),
 .UNSPECIFIED., .F., .F.,
 ( 4, 2, 4 ),
 ( 0.000000000000000000, 0.5000000000000000000, 1.000000000000000000 ),
 .UNSPECIFIED. ) ;
#13398 = CARTESIAN_POINT ( 'NONE',  ( 4.080592064681261455, -5.083854565965863159, -3.105321867100004241 ) ) ;
#13399 = CARTESIAN_POINT ( 'NONE',  ( 0.2309929099465236890, 4.358477053493579056, -22.44418644580001043 ) ) ;
#13400 = CARTESIAN_POINT ( 'NONE',  ( -6.112318018889845384, -26.81313817375427178, 208.9612952676429245 ) ) ;
#13401 = CARTESIAN_POINT ( 'NONE',  ( -23.94309786570000043, 13.28188914049999880, 230.6999999999999886 ) ) ;
#13402 = CARTESIAN_POINT ( 'NONE',  ( 24.73445225629999911, -14.15837998019999944, 223.9040346120000038 ) ) ;
#13403 = CARTESIAN_POINT ( 'NONE',  ( -22.55348085480000364, 18.07310466239999869, 229.0000000000000000 ) ) ;
#13404 = CARTESIAN_POINT ( 'NONE',  ( 17.95841148948556310, 10.23646161652002817, -0.6999999999999784173 ) ) ;
#13405 = CARTESIAN_POINT ( 'NONE',  ( 9.999999999982071230, -128.1247626104539279, -35.28103264683748819 ) ) ;
#13406 = CARTESIAN_POINT ( 'NONE',  ( -17.93058398061198133, 10.83371123202060993, 0.000000000000000000 ) ) ;
#13407 = CARTESIAN_POINT ( 'NONE',  ( -24.12155405280000053, -12.35224656769999996, 230.6999999999999886 ) ) ;
#13408 = CARTESIAN_POINT ( 'NONE',  ( -27.69999999930000101, 3.392159599999999562E-15, 90.00000000000000000 ) ) ;
#13409 = VERTEX_POINT ( 'NONE', #28726 ) ;
#13410 = CARTESIAN_POINT ( 'NONE',  ( 4.569612387855602087, -0.08076758077263379576, -58.09793411332499602 ) ) ;
#13411 = CARTESIAN_POINT ( 'NONE',  ( 0.000000000000000000, -119.7166638525666826, -43.39999999999999858 ) ) ;
#13412 = ORIENTED_EDGE ( 'NONE', *, *, #14640, .T. ) ;
#13413 = CARTESIAN_POINT ( 'NONE',  ( -2.825020644939634007, -4.425443225455641283, -0.6999999999999992895 ) ) ;
#13414 = ORIENTED_EDGE ( 'NONE', *, *, #2473, .F. ) ;
#13415 = DIRECTION ( 'NONE',  ( 0.000000000000000000, 1.000000000000000000, 0.000000000000000000 ) ) ;
#13416 = DIRECTION ( 'NONE',  ( 0.2665630446479613780, 0.9085064176298685013, -0.3218077568259533061 ) ) ;
#13417 = ORIENTED_EDGE ( 'NONE', *, *, #28501, .F. ) ;
#13418 = FACE_OUTER_BOUND ( 'NONE', #16334, .T. ) ;
#13419 = ORIENTED_EDGE ( 'NONE', *, *, #30813, .F. ) ;
#13420 = ORIENTED_EDGE ( 'NONE', *, *, #27315, .F. ) ;
#13421 = CARTESIAN_POINT ( 'NONE',  ( -7.105427357599999217E-15, -7.105427357599999217E-15, 36.78285841159999592 ) ) ;
#13422 = ORIENTED_EDGE ( 'NONE', *, *, #232, .F. ) ;
#13423 = DIRECTION ( 'NONE',  ( 0.000000000000000000, 0.000000000000000000, 1.000000000000000000 ) ) ;
#13424 = B_SPLINE_CURVE_WITH_KNOTS ( 'NONE', 3,
 ( #7928, #5421, #9682, #5112, #19597, #29176, #5272, #571, #19750, #12048 ),
 .UNSPECIFIED., .F., .F.,
 ( 4, 2, 2, 2, 4 ),
 ( 0.000000000000000000, 0.2500000000000000000, 0.5000000000000000000, 0.7500000000000000000, 1.000000000000000000 ),
 .UNSPECIFIED. ) ;
#13425 = CARTESIAN_POINT ( 'NONE',  ( -8.699999999669005391, -18.23122067931867107, -34.51216076567753532 ) ) ;
#13426 = CARTESIAN_POINT ( 'NONE',  ( 1.304267357867700872, -5.326741986711696519, -63.90397119102498635 ) ) ;
#13427 = EDGE_CURVE ( 'NONE', #15990, #12600, #9112, .T. ) ;
#13428 = CARTESIAN_POINT ( 'NONE',  ( -22.88601245399999939, -20.23007972099999563, 229.7313215430000071 ) ) ;
#13429 = B_SPLINE_CURVE_WITH_KNOTS ( 'NONE', 3,
 ( #1, #1738, #9422, #6446, #9113, #16509 ),
 .UNSPECIFIED., .F., .F.,
 ( 4, 2, 4 ),
 ( 0.000000000000000000, 0.5000000000000000000, 1.000000000000000000 ),
 .UNSPECIFIED. ) ;
#13430 = AXIS2_PLACEMENT_3D ( 'NONE', #10041, #304, #9722 ) ;
#13431 = CARTESIAN_POINT ( 'NONE',  ( 1.099998580829999906, -27.77839262550000043, 225.0000014190000002 ) ) ;
#13432 = CARTESIAN_POINT ( 'NONE',  ( -28.50002393070000295, -4.358072777779999203E-15, 222.0000000000000000 ) ) ;
#13433 = DIRECTION ( 'NONE',  ( 0.000000000000000000, 0.000000000000000000, -1.000000000000000000 ) ) ;
#13434 = ORIENTED_EDGE ( 'NONE', *, *, #26012, .F. ) ;
#13435 = ADVANCED_FACE ( 'NONE', ( #20211 ), #29803, .T. ) ;
#13436 = CYLINDRICAL_SURFACE ( 'NONE', #21527, 27.50000000000000000 ) ;
#13437 = CARTESIAN_POINT ( 'NONE',  ( -2.929853409778804263, 3.622264489389753539, -13.10352819870000118 ) ) ;
#13438 = CARTESIAN_POINT ( 'NONE',  ( 10.69999999999999929, -27.00000000000000000, -28.40000000000000213 ) ) ;
#13439 = CARTESIAN_POINT ( 'NONE',  ( -26.79556473285982321, -0.4875557887251183442, -0.6999999999999784173 ) ) ;
#13440 = ORIENTED_EDGE ( 'NONE', *, *, #23883, .T. ) ;
#13441 = CARTESIAN_POINT ( 'NONE',  ( 24.69936741169999905, -14.21947533890000059, 223.9000014189999774 ) ) ;
#13442 = CARTESIAN_POINT ( 'NONE',  ( 17.00199034983389978, -7.902812560182772117, -0.6999999999999783062 ) ) ;
#13443 = CARTESIAN_POINT ( 'NONE',  ( -24.36375418918093061, -14.78716628874576244, 6.095965061000018892 ) ) ;
#13444 = CARTESIAN_POINT ( 'NONE',  ( 9.944224317832768278, -25.63928765730900139, 26.94315197391175332 ) ) ;
#13445 = CARTESIAN_POINT ( 'NONE',  ( -9.738910687886857431, -24.96785170200598714, 202.5331423531274311 ) ) ;
#13446 = FACE_OUTER_BOUND ( 'NONE', #9400, .T. ) ;
#13447 = CARTESIAN_POINT ( 'NONE',  ( -23.47637529058820860, -14.89020704899713365, 5.901296963999991263 ) ) ;
#13448 = DIRECTION ( 'NONE',  ( 0.000000000000000000, 0.7113488923935522568, -0.7028390664230799167 ) ) ;
#13449 = VERTEX_POINT ( 'NONE', #1179 ) ;
#13450 = EDGE_CURVE ( 'NONE', #11773, #15620, #27494, .T. ) ;
#13451 = FACE_OUTER_BOUND ( 'NONE', #11986, .T. ) ;
#13452 = CARTESIAN_POINT ( 'NONE',  ( 26.95545381250000361, 8.667969382629999942, 224.8000000000000114 ) ) ;
#13453 = VECTOR ( 'NONE', #16871, 1000.000000000000000 ) ;
#13454 = ADVANCED_FACE ( 'NONE', ( #6044 ), #22268, .F. ) ;
#13455 = AXIS2_PLACEMENT_3D ( 'NONE', #16943, #128, #7649 ) ;
#13456 = CARTESIAN_POINT ( 'NONE',  ( 1.338051363053742282, -3.857864915027613861, -68.10000000002501963 ) ) ;
#13457 = CIRCLE ( 'NONE', #432, 4.000000004070001225 ) ;
#13458 = DIRECTION ( 'NONE',  ( 1.000000000000000000, 0.000000000000000000, 0.000000000000000000 ) ) ;
#13459 = CARTESIAN_POINT ( 'NONE',  ( -23.78789221090044137, 14.38747862758026663, 5.287321609440595260 ) ) ;
#13460 = DIRECTION ( 'NONE',  ( 1.000000000000000000, 0.000000000000000000, 0.000000000000000000 ) ) ;
#13461 = CARTESIAN_POINT ( 'NONE',  ( -2.900346203986609694, 11.98357192835207741, 232.6627637660202481 ) ) ;
#13462 = CARTESIAN_POINT ( 'NONE',  ( 6.385918709370476343, 0.1527399656023400998, -64.06686508972499894 ) ) ;
#13463 = ORIENTED_EDGE ( 'NONE', *, *, #1567, .F. ) ;
#13464 = LINE ( 'NONE', #18016, #29553 ) ;
#13465 = ORIENTED_EDGE ( 'NONE', *, *, #5330, .F. ) ;
#13467 = EDGE_CURVE ( 'NONE', #6095, #16248, #27443, .T. ) ;
#13466 = CARTESIAN_POINT ( 'NONE',  ( -1.609514238130545838, -3.181902231687246285, -88.52261276296684400 ) ) ;
#13468 = ORIENTED_EDGE ( 'NONE', *, *, #21414, .F. ) ;
#13469 = CARTESIAN_POINT ( 'NONE',  ( -10.99999999969999998, 20.99999999999999645, -70.09999999999999432 ) ) ;
#13470 = FACE_OUTER_BOUND ( 'NONE', #938, .T. ) ;
#13471 = CARTESIAN_POINT ( 'NONE',  ( -12.47331730070000155, 21.70000000000000284, -55.90289625529999995 ) ) ;
#13472 = CARTESIAN_POINT ( 'NONE',  ( -15.86372220156776613, 10.46175468665682118, -0.6999999999999785283 ) ) ;
#13473 = AXIS2_PLACEMENT_3D ( 'NONE', #28100, #8899, #15986 ) ;
#13474 = CARTESIAN_POINT ( 'NONE',  ( 0.4478609109089253248, -28.49673184309138918, 3.901345920999998995 ) ) ;
#13475 = VECTOR ( 'NONE', #21191, 1000.000000000000000 ) ;
#13476 = CARTESIAN_POINT ( 'NONE',  ( 6.770906559283583981, -16.24115510245209038, -74.78962657635717903 ) ) ;
#13477 = DIRECTION ( 'NONE',  ( 0.000000000000000000, -2.255973186040000320E-12, -1.000000000000000000 ) ) ;
#13478 = EDGE_LOOP ( 'NONE', ( #8378, #5059, #30209, #6157 ) ) ;
#13479 = DIRECTION ( 'NONE',  ( 0.000000000000000000, -0.3420201433259318358, 0.9396926207858125046 ) ) ;
#13480 = CARTESIAN_POINT ( 'NONE',  ( 3.767248616521118976, -2.502283324777556661, -0.7105340489000482318 ) ) ;
#13481 = EDGE_CURVE ( 'NONE', #24619, #8103, #29962, .T. ) ;
#13482 = DIRECTION ( 'NONE',  ( 1.000000000000000000, 0.000000000000000000, 0.000000000000000000 ) ) ;
#13483 = CARTESIAN_POINT ( 'NONE',  ( 0.000000000000000000, -119.7166638525666826, -44.10000000000000142 ) ) ;
#13484 = CARTESIAN_POINT ( 'NONE',  ( -24.25909092270000045, -14.95913241679999928, 225.7602679599999931 ) ) ;
#13485 = DIRECTION ( 'NONE',  ( -0.8775825618903722036, -0.4794255386042040601, 0.000000000000000000 ) ) ;
#13486 = EDGE_CURVE ( 'NONE', #21601, #23040, #20067, .T. ) ;
#13487 = CARTESIAN_POINT ( 'NONE',  ( -1.099929244070900536, -27.47799402545702563, 225.1456731700734792 ) ) ;
#13488 = CARTESIAN_POINT ( 'NONE',  ( -16.03124949821963341, 10.23368197014037406, -1.400000000000001910 ) ) ;
#13489 = CARTESIAN_POINT ( 'NONE',  ( 5.066518387468507356, -3.138291312573631586, -48.85324460762499399 ) ) ;
#13490 = VECTOR ( 'NONE', #12783, 1000.000000000000000 ) ;
#13491 = EDGE_CURVE ( 'NONE', #26103, #20099, #1028, .T. ) ;
#13492 = CARTESIAN_POINT ( 'NONE',  ( -23.24663841807413434, -14.69162354064478571, 5.096459710828290746 ) ) ;
#13493 = CARTESIAN_POINT ( 'NONE',  ( 14.80644526029530539, -28.75091651964295991, -33.16236467793404330 ) ) ;
#13494 = DIRECTION ( 'NONE',  ( 0.9880370573969196046, -0.1542166437529880751, 0.000000000000000000 ) ) ;
#13495 = AXIS2_PLACEMENT_3D ( 'NONE', #30544, #8972, #25511 ) ;
#13496 = PRODUCT_RELATED_PRODUCT_CATEGORY ( 'part', '', ( #28241 ) ) ;
#13497 = CARTESIAN_POINT ( 'NONE',  ( -23.86403265537058616, -13.66628296746374893, 223.9000000000011426 ) ) ;
#13498 = ORIENTED_EDGE ( 'NONE', *, *, #29496, .F. ) ;
#13499 = CARTESIAN_POINT ( 'NONE',  ( 5.877945039781666381, 1.734296231098907182, -36.13159726780000369 ) ) ;
#13500 = AXIS2_PLACEMENT_3D ( 'NONE', #30165, #3414, #18198 ) ;
#13501 = ORIENTED_EDGE ( 'NONE', *, *, #24895, .F. ) ;
#13502 = CARTESIAN_POINT ( 'NONE',  ( 0.7192951553254730568, 4.518739695583319893, -54.81500058692499522 ) ) ;
#13503 = ORIENTED_EDGE ( 'NONE', *, *, #30861, .F. ) ;
#13504 = SHAPE_DEFINITION_REPRESENTATION ( #13337, #339 ) ;
#13505 = ORIENTED_EDGE ( 'NONE', *, *, #27343, .F. ) ;
#13506 = EDGE_CURVE ( 'NONE', #17663, #11652, #3685, .T. ) ;
#13507 = ORIENTED_EDGE ( 'NONE', *, *, #20200, .T. ) ;
#13508 = SURFACE_STYLE_FILL_AREA ( #27825 ) ;
#13509 = CARTESIAN_POINT ( 'NONE',  ( 17.73794748049035874, 10.04907227125707792, -4.336808689942017243E-16 ) ) ;
#13510 = CARTESIAN_POINT ( 'NONE',  ( -17.49230054464772977, -29.69120553467622869, -24.18026554819070739 ) ) ;
#13511 = VECTOR ( 'NONE', #27333, 1000.000000000000000 ) ;
#13512 = ADVANCED_FACE ( 'NONE', ( #13284 ), #18008, .T. ) ;
#13513 = LINE ( 'NONE', #27511, #30017 ) ;
#13514 = DIRECTION ( 'NONE',  ( 0.000000000000000000, -1.000000000000000000, 0.000000000000000000 ) ) ;
#13515 = CARTESIAN_POINT ( 'NONE',  ( 3.550686850769999806E-05, -28.50022181210000127, 226.1000014189999945 ) ) ;
#13516 = CARTESIAN_POINT ( 'NONE',  ( -2.886686092853935293, -3.810306705960904594, -2.791445369299998536 ) ) ;
#13517 = CARTESIAN_POINT ( 'NONE',  ( -8.424250880209998925E-16, -2.000000000000000000, 230.8412452700000017 ) ) ;
#13518 = B_SPLINE_CURVE_WITH_KNOTS ( 'NONE', 3,
 ( #24717, #14667, #19851, #5056, #19541, #15119, #7868, #28808, #17472, #27078, #11983, #29124 ),
 .UNSPECIFIED., .F., .F.,
 ( 4, 2, 2, 2, 2, 4 ),
 ( 0.000000000000000000, 0.2499999999999932276, 0.3749999999999916178, 0.4374999999999923395, 0.4999999999999931166, 1.000000000000000000 ),
 .UNSPECIFIED. ) ;
#13519 = DIRECTION ( 'NONE',  ( -1.224606353819999829E-16, -1.000000000000000000, 0.000000000000000000 ) ) ;
#13520 = EDGE_CURVE ( 'NONE', #19036, #29420, #22274, .T. ) ;
#13521 = CARTESIAN_POINT ( 'NONE',  ( 1.942707423728255778, -5.758494596869851989, -15.26414732020000464 ) ) ;
#13522 = CARTESIAN_POINT ( 'NONE',  ( 4.417684705200791484, 4.247747620870205409, -34.72341724620000036 ) ) ;
#13523 = VECTOR ( 'NONE', #23062, 1000.000000000000000 ) ;
#13524 = CARTESIAN_POINT ( 'NONE',  ( 8.999999999769999093, 20.50498856619357113, -44.22672584786599970 ) ) ;
#13525 = CARTESIAN_POINT ( 'NONE',  ( -10.14902473054660348, -26.01926976365539090, 137.9396849850000137 ) ) ;
#13526 = CARTESIAN_POINT ( 'NONE',  ( -19.79264346680938758, 19.51191464210150173, 0.8505138480000007384 ) ) ;
#13527 = CARTESIAN_POINT ( 'NONE',  ( 3.940320149735934141, -28.38476056077625742, 8.000000000000007105 ) ) ;
#13528 = DIRECTION ( 'NONE',  ( 0.3633921898465289901, 0.9316362575375348731, -1.734723475976805832E-14 ) ) ;
#13529 = B_SPLINE_CURVE_WITH_KNOTS ( 'NONE', 5,
 ( #16827, #24804, #7078, #21712, #19353, #16666, #19508, #21409, #11953, #26435, #14331, #2214 ),
 .UNSPECIFIED., .F., .F.,
 ( 6, 3, 3, 6 ),
 ( 2.782752056640000138, 3.293393369919999980, 4.940089939659999985, 5.565010778129999558 ),
 .UNSPECIFIED. ) ;
#13530 = CARTESIAN_POINT ( 'NONE',  ( -6.982632971260602339, 5.672256964453205264, -40.24571374340602148 ) ) ;
#13531 = CYLINDRICAL_SURFACE ( 'NONE', #29322, 26.80000000000002203 ) ;
#13532 = CARTESIAN_POINT ( 'NONE',  ( 8.700000000287717583, -16.96959321760160222, -37.81493174583334849 ) ) ;
#13533 = CARTESIAN_POINT ( 'NONE',  ( 11.00000000000000000, 26.42151601322854759, -59.26168417594741555 ) ) ;
#13534 = B_SPLINE_CURVE_WITH_KNOTS ( 'NONE', 3,
 ( #2311, #7022, #5540, #11894, #14852, #4512, #12469, #4657, #21496, #24443 ),
 .UNSPECIFIED., .F., .F.,
 ( 4, 2, 2, 2, 4 ),
 ( 0.000000000000000000, 0.2500000000000000000, 0.5000000000000000000, 0.7500000000000000000, 1.000000000000000000 ),
 .UNSPECIFIED. ) ;
#13535 = ORIENTED_EDGE ( 'NONE', *, *, #13491, .T. ) ;
#13536 = CARTESIAN_POINT ( 'NONE',  ( 0.6616560533897080099, -3.500000000000000444, 227.6811464142208479 ) ) ;
#13537 = DIRECTION ( 'NONE',  ( 0.000000000000000000, -0.000000000000000000, 1.000000000000000000 ) ) ;
#13538 = CARTESIAN_POINT ( 'NONE',  ( -2.413485703671791605, -4.688120701072898910, -0.7000000000061800121 ) ) ;
#13539 = ORIENTED_EDGE ( 'NONE', *, *, #12199, .F. ) ;
#13540 = CARTESIAN_POINT ( 'NONE',  ( 3.001777156698443250, -4.698362801289899693, -44.04966640442499681 ) ) ;
#13541 = VERTEX_POINT ( 'NONE', #9031 ) ;
#13542 = ORIENTED_EDGE ( 'NONE', *, *, #23342, .T. ) ;
#13543 =( NAMED_UNIT ( * ) SI_UNIT ( $, .STERADIAN. ) SOLID_ANGLE_UNIT ( ) );
#13544 = VECTOR ( 'NONE', #10762, 1000.000000000000000 ) ;
#13545 = ORIENTED_EDGE ( 'NONE', *, *, #17209, .T. ) ;
#13546 = FACE_OUTER_BOUND ( 'NONE', #26037, .T. ) ;
#13547 = EDGE_CURVE ( 'NONE', #26737, #17896, #4603, .T. ) ;
#13548 = ORIENTED_EDGE ( 'NONE', *, *, #22817, .T. ) ;
#13549 = CARTESIAN_POINT ( 'NONE',  ( -25.22658730140000216, -13.26242337740000110, 225.1042194559999814 ) ) ;
#13550 =( LENGTH_UNIT ( ) NAMED_UNIT ( * ) SI_UNIT ( .MILLI., .METRE. ) );
#13551 = DIRECTION ( 'NONE',  ( 0.000000000000000000, 0.000000000000000000, 1.000000000000000000 ) ) ;
#13552 = CLOSED_SHELL ( 'NONE', ( #26530, #995, #28156, #19886, #6623, #12439, #14010, #29468, #14404, #20556, #26844, #15389, #13295, #5684 ) ) ;
#13553 = B_SPLINE_CURVE_WITH_KNOTS ( 'NONE', 1,
 ( #11995, #11842 ),
 .UNSPECIFIED., .F., .F.,
 ( 2, 2 ),
 ( -0.0003774847559270000114, 0.7000000095410000567 ),
 .UNSPECIFIED. ) ;
#13554 = EDGE_CURVE ( 'NONE', #18252, #9397, #11558, .T. ) ;
#13555 = CARTESIAN_POINT ( 'NONE',  ( 0.1183905698532920631, -5.181952515350124244, -93.28167488204269375 ) ) ;
#13556 = EDGE_CURVE ( 'NONE', #8808, #6095, #23001, .T. ) ;
#13557 = CARTESIAN_POINT ( 'NONE',  ( -27.23548386990000125, 3.335274659649999582E-15, 138.3395398259999922 ) ) ;
#13558 = CARTESIAN_POINT ( 'NONE',  ( 2.720322858944644207, -2.288262595320229131, 227.6701688388524190 ) ) ;
#13559 = CARTESIAN_POINT ( 'NONE',  ( 23.79192443588063455, -14.38068074323726186, 4.711737058110762710 ) ) ;
#13560 = ORIENTED_EDGE ( 'NONE', *, *, #14423, .T. ) ;
#13561 = CARTESIAN_POINT ( 'NONE',  ( -4.646804529178800713, -0.2974863596997128767, -4.648838774900006854 ) ) ;
#13562 = CARTESIAN_POINT ( 'NONE',  ( 4.266075142677459908, -0.9221078188639819651, -23.29036215649999875 ) ) ;
#13563 = CARTESIAN_POINT ( 'NONE',  ( -5.654928157491454499, -26.91331636611315759, 209.2041907114654862 ) ) ;
#13564 = B_SPLINE_CURVE_WITH_KNOTS ( 'NONE', 3,
 ( #2615, #16927, #29043, #24027, #273, #19919 ),
 .UNSPECIFIED., .F., .F.,
 ( 4, 2, 4 ),
 ( 0.000000000000000000, 0.5000000000000000000, 1.000000000000000000 ),
 .UNSPECIFIED. ) ;
#13565 = CARTESIAN_POINT ( 'NONE',  ( -18.29999999989999893, -29.92682926828999967, -28.39999999989999679 ) ) ;
#13566 = CARTESIAN_POINT ( 'NONE',  ( -2.077512584961602293, -2.798799908081698540, -90.35662574872537789 ) ) ;
#13567 = CARTESIAN_POINT ( 'NONE',  ( -7.614137047376521750, -115.2001938015495028, 21.77735005150014302 ) ) ;
#13568 = LINE ( 'NONE', #11365, #10630 ) ;
#13569 = CARTESIAN_POINT ( 'NONE',  ( -24.34159889609999894, -14.82483853620000147, 225.9014025209999943 ) ) ;
#13570 = CARTESIAN_POINT ( 'NONE',  ( 27.79999999980000069, -7.282770092329999834, 229.0000000000000000 ) ) ;
#13571 = CARTESIAN_POINT ( 'NONE',  ( -19.80526744909999692, 19.50877353739999975, 229.0000000010000178 ) ) ;
#13572 = LINE ( 'NONE', #6799, #21833 ) ;
#13573 = ORIENTED_EDGE ( 'NONE', *, *, #532, .F. ) ;
#13574 = CARTESIAN_POINT ( 'NONE',  ( 3.178712542294670040, -4.426710093576285310, -60.72197827312499641 ) ) ;
#13575 = CARTESIAN_POINT ( 'NONE',  ( -13.11056599509667464, -23.44705117439653819, 36.78285841135430445 ) ) ;
#13576 = ORIENTED_EDGE ( 'NONE', *, *, #28483, .F. ) ;
#13577 = CARTESIAN_POINT ( 'NONE',  ( -24.83284505762695815, -10.07844553579556823, 93.21714158839638742 ) ) ;
#13578 = CARTESIAN_POINT ( 'NONE',  ( 1.888485499342153151, 5.773790730162923879, -11.07047964830000453 ) ) ;
#13579 = ORIENTED_EDGE ( 'NONE', *, *, #19236, .F. ) ;
#13580 = CARTESIAN_POINT ( 'NONE',  ( -23.78820481377726281, 14.38695943193400417, 4.711274593993440618 ) ) ;
#13581 = CARTESIAN_POINT ( 'NONE',  ( 26.80000000069999899, -3.281945028320000125E-15, 186.7828584129999854 ) ) ;
#13582 = VERTEX_POINT ( 'NONE', #11091 ) ;
#13583 = EDGE_CURVE ( 'NONE', #24581, #9016, #5467, .T. ) ;
#13584 = EDGE_LOOP ( 'NONE', ( #21289, #23861, #1160, #4308 ) ) ;
#13585 = EDGE_CURVE ( 'NONE', #49, #18717, #6669, .T. ) ;
#13586 = ORIENTED_EDGE ( 'NONE', *, *, #14851, .T. ) ;
#13587 = DIRECTION ( 'NONE',  ( 0.3090169943750400994, -0.9510565162951234441, 0.000000000000000000 ) ) ;
#13588 =( NAMED_UNIT ( * ) SI_UNIT ( $, .STERADIAN. ) SOLID_ANGLE_UNIT ( ) );
#13589 = ORIENTED_EDGE ( 'NONE', *, *, #1528, .F. ) ;
#13590 = CARTESIAN_POINT ( 'NONE',  ( -12.30000000021392736, -28.96654950391973671, -30.95893389568501419 ) ) ;
#13591 = VECTOR ( 'NONE', #12428, 1000.000000000000000 ) ;
#13592 = CARTESIAN_POINT ( 'NONE',  ( -10.00000000057898220, -121.7869891323785083, -31.32664466904982348 ) ) ;
#13593 = CARTESIAN_POINT ( 'NONE',  ( 4.441146713721671802, -1.990734395214990071, -67.27841551502500295 ) ) ;
#13594 = CARTESIAN_POINT ( 'NONE',  ( 27.79999999999999716, 2.356159711779999785E-11, 229.0000000000000000 ) ) ;
#13595 = B_SPLINE_CURVE_WITH_KNOTS ( 'NONE', 3,
 ( #10360, #29389, #8285, #19952, #17429, #30005 ),
 .UNSPECIFIED., .F., .F.,
 ( 4, 2, 4 ),
 ( 0.000000000000000000, 0.5000000000000000000, 1.000000000000000000 ),
 .UNSPECIFIED. ) ;
#13596 = CARTESIAN_POINT ( 'NONE',  ( -1.099927927707951447, -26.77741881808350044, 224.8541214485396722 ) ) ;
#13597 = DIRECTION ( 'NONE',  ( 0.7071067811870488384, 0.000000000000000000, -0.7071067811860461960 ) ) ;
#13598 = DIRECTION ( 'NONE',  ( 0.000000000000000000, 0.000000000000000000, -1.000000000000000000 ) ) ;
#13599 = ORIENTED_EDGE ( 'NONE', *, *, #4593, .F. ) ;
#13600 = FACE_OUTER_BOUND ( 'NONE', #29253, .T. ) ;
#13601 = CARTESIAN_POINT ( 'NONE',  ( 4.630235822890138131, 0.3309221515414816350, -14.14454535870000029 ) ) ;
#13602 = DIRECTION ( 'NONE',  ( 1.000000000000000000, -1.224606353819999829E-16, 0.000000000000000000 ) ) ;
#13603 = CARTESIAN_POINT ( 'NONE',  ( -27.55801272791059731, -0.5014288284350311153, -0.5592437529999827461 ) ) ;
#13604 = ORIENTED_EDGE ( 'NONE', *, *, #7405, .F. ) ;
#13605 = CARTESIAN_POINT ( 'NONE',  ( 18.65047562642688916, 19.27644483004725728, -1.399999999999998579 ) ) ;
#13606 = CARTESIAN_POINT ( 'NONE',  ( -22.95800506017165077, -13.82601854610103409, 4.006804826634700945 ) ) ;
#13607 = DIRECTION ( 'NONE',  ( 0.3633921898465273803, -0.9316362575375355393, -2.081668171172167567E-14 ) ) ;
#13608 = CARTESIAN_POINT ( 'NONE',  ( 27.71196445724500990, 5.091237891590008502, 0.8585786439999909536 ) ) ;
#13609 = DIRECTION ( 'NONE',  ( 0.000000000000000000, -1.000000000000000000, 0.000000000000000000 ) ) ;
#13610 = CARTESIAN_POINT ( 'NONE',  ( 3.314820598666778917, -5.455691467570147779, -46.56669147682499954 ) ) ;
#13611 = CARTESIAN_POINT ( 'NONE',  ( 27.23548386990000125, -3.335274659639999982E-15, 191.6604601740000078 ) ) ;
#13612 = CARTESIAN_POINT ( 'NONE',  ( -4.175165894169885483, -119.7166638525666826, -44.10000000000000142 ) ) ;
#13613 = EDGE_LOOP ( 'NONE', ( #2407, #30814, #17228, #11885 ) ) ;
#13614 = ADVANCED_FACE ( 'NONE', ( #25570 ), #27593, .T. ) ;
#13615 = CARTESIAN_POINT ( 'NONE',  ( 24.29138541237941240, -13.52003710528471281, 3.901342110999989288 ) ) ;
#13616 = CARTESIAN_POINT ( 'NONE',  ( 19.80538173169999894, 19.50875421069999760, 222.0000000000000000 ) ) ;
#13617 = EDGE_CURVE ( 'NONE', #5647, #13739, #5384, .T. ) ;
#13618 =( REPRESENTATION_RELATIONSHIP ('NONE','NONE', #2712, #17403 ) REPRESENTATION_RELATIONSHIP_WITH_TRANSFORMATION ( #2176 )SHAPE_REPRESENTATION_RELATIONSHIP( ) );
#13619 = CARTESIAN_POINT ( 'NONE',  ( 2.029564108346094908, -3.664007903844075820, -68.10000000002500542 ) ) ;
#13620 = ADVANCED_FACE ( 'NONE', ( #16578 ), #15527, .F. ) ;
#13621 = CARTESIAN_POINT ( 'NONE',  ( 22.88248055069271203, 14.29577554333692468, -0.6999999999999784173 ) ) ;
#13622 = CARTESIAN_POINT ( 'NONE',  ( -23.84668919686734156, 14.28982133724830383, 5.560031205887339567 ) ) ;
#13623 = CIRCLE ( 'NONE', #19643, 3.000000000000001332 ) ;
#13624 = CARTESIAN_POINT ( 'NONE',  ( 14.75111860152068033, -23.36471428914778059, -32.07437842398911698 ) ) ;
#13625 = CARTESIAN_POINT ( 'NONE',  ( 1.818424738700763044, 3.920024695825002681, -39.39109296325933940 ) ) ;
#13626 = CARTESIAN_POINT ( 'NONE',  ( 3.705709820302785396, 4.685590126413917034, -63.63768011632500787 ) ) ;
#13627 = ORIENTED_EDGE ( 'NONE', *, *, #9680, .T. ) ;
#13628 = CARTESIAN_POINT ( 'NONE',  ( 24.64102059410889822, -12.87216126329460941, 4.113191254464338975 ) ) ;
#13629 = ORIENTED_EDGE ( 'NONE', *, *, #30930, .T. ) ;
#13630 = CARTESIAN_POINT ( 'NONE',  ( -18.15350094950000326, 19.92137095469999863, 229.9929676959999938 ) ) ;
#13631 = VERTEX_POINT ( 'NONE', #30282 ) ;
#13632 = DIRECTION ( 'NONE',  ( -9.220055274816719609E-13, -0.9128796883888953273, 0.4082287037029531662 ) ) ;
#13633 = EDGE_CURVE ( 'NONE', #8882, #27430, #12165, .T. ) ;
#13634 = CARTESIAN_POINT ( 'NONE',  ( -27.23548386990000125, 3.335274659649999582E-15, 188.3395398260000206 ) ) ;
#13635 = CYLINDRICAL_SURFACE ( 'NONE', #21543, 3.000000000000005329 ) ;
#13636 = CARTESIAN_POINT ( 'NONE',  ( -3.221827467136498591, -1.415571281914143720, 0.000000000000000000 ) ) ;
#13637 = CARTESIAN_POINT ( 'NONE',  ( 0.4831567132674381426, -28.49614615030699838, 3.899998581000013509 ) ) ;
#13638 = CARTESIAN_POINT ( 'NONE',  ( -16.14281465707167840, -9.860486966977234147, 0.000000000000000000 ) ) ;
#13639 = CARTESIAN_POINT ( 'NONE',  ( 8.700000000245887932, -28.22468611110281245, -31.13863906511161517 ) ) ;
#13640 = ADVANCED_FACE ( 'NONE', ( #17045 ), #19412, .T. ) ;
#13641 = ORIENTED_EDGE ( 'NONE', *, *, #80, .T. ) ;
#13642 = FACE_BOUND ( 'NONE', #18539, .T. ) ;
#13643 = CARTESIAN_POINT ( 'NONE',  ( 3.728929371600147924, -2.476830901180399724, -0.7104894750999627417 ) ) ;
#13644 = CARTESIAN_POINT ( 'NONE',  ( -3.797468263909999919, 11.45463590949999855, 231.9999989789999972 ) ) ;
#13645 = CARTESIAN_POINT ( 'NONE',  ( -2.631407904598755287, 2.442267813799901433, 230.7846409045018277 ) ) ;
#13646 = VECTOR ( 'NONE', #16506, 1000.000000000000000 ) ;
#13647 = CARTESIAN_POINT ( 'NONE',  ( -24.68204616399999907, -14.25020164319999871, 226.1000014189999945 ) ) ;
#13648 = CARTESIAN_POINT ( 'NONE',  ( -0.4820778520819999913, -28.49640832880000119, 226.0025182780000250 ) ) ;
#13649 = CARTESIAN_POINT ( 'NONE',  ( 8.700000000245887932, -28.22468611110281245, -31.13863906511161517 ) ) ;
#13650 = CARTESIAN_POINT ( 'NONE',  ( -16.66189934012373897, 9.903956624658377450, -1.400000000000001910 ) ) ;
#13651 = CARTESIAN_POINT ( 'NONE',  ( -5.473571180597741836, 3.247285761689575168, -50.83267869292499341 ) ) ;
#13652 = B_SPLINE_CURVE_WITH_KNOTS ( 'NONE', 3,
 ( #13161, #13326, #24974, #1538, #22768, #30491 ),
 .UNSPECIFIED., .F., .F.,
 ( 4, 2, 4 ),
 ( 0.000000000000000000, 0.5000000000000000000, 1.000000000000000000 ),
 .UNSPECIFIED. ) ;
#13653 = CARTESIAN_POINT ( 'NONE',  ( 26.79556473285982321, 0.4875557887249620803, 0.000000000000000000 ) ) ;
#13654 = CARTESIAN_POINT ( 'NONE',  ( 17.93011078763067090, 11.79183908526299085, 0.000000000000000000 ) ) ;
#13655 = CARTESIAN_POINT ( 'NONE',  ( 0.000000000000000000, 21.72305290929948640, -60.97178489257708378 ) ) ;
#13656 = EDGE_CURVE ( 'NONE', #17696, #6778, #11018, .T. ) ;
#13657 = CARTESIAN_POINT ( 'NONE',  ( -2.947640775130000104E-14, -27.50000000000000000, 223.8999999999999773 ) ) ;
#13658 = ORIENTED_EDGE ( 'NONE', *, *, #18659, .F. ) ;
#13659 = CARTESIAN_POINT ( 'NONE',  ( 4.051823674760414384, -0.6775361292690335047, -36.24517599850000948 ) ) ;
#13660 = ORIENTED_EDGE ( 'NONE', *, *, #29983, .F. ) ;
#13661 = CARTESIAN_POINT ( 'NONE',  ( 3.317242526498128008, 4.404831280267538673, -55.42619010302500016 ) ) ;
#13662 = EDGE_LOOP ( 'NONE', ( #3986, #30581, #3317, #22452 ) ) ;
#13663 = APPLICATION_PROTOCOL_DEFINITION ( 'draft international standard', 'automotive_design', 1998, #25243 ) ;
#13664 = VECTOR ( 'NONE', #16158, 1000.000000000000000 ) ;
#13665 = VERTEX_POINT ( 'NONE', #29304 ) ;
#13666 = EDGE_LOOP ( 'NONE', ( #15571, #3788, #4623, #6544, #462 ) ) ;
#13667 = EDGE_CURVE ( 'NONE', #6732, #25385, #27905, .T. ) ;
#13668 = CARTESIAN_POINT ( 'NONE',  ( 14.65905325912680013, -27.90098191447954434, -23.14712954807390588 ) ) ;
#13669 = LINE ( 'NONE', #16641, #26546 ) ;
#13670 = CARTESIAN_POINT ( 'NONE',  ( -17.45872973692405594, -28.73157446327232734, -23.62622229079265779 ) ) ;
#13671 = ADVANCED_FACE ( 'NONE', ( #12017 ), #26491, .F. ) ;
#13672 = DIRECTION ( 'NONE',  ( 0.000000000000000000, 0.000000000000000000, 1.000000000000000000 ) ) ;
#13673 = CARTESIAN_POINT ( 'NONE',  ( -16.85343921402336775, -7.900182044543379689, -0.6999999999999784173 ) ) ;
#13674 = CARTESIAN_POINT ( 'NONE',  ( -3.552713678799999608E-15, 0.000000000000000000, 43.21714158840000408 ) ) ;
#13675 = CARTESIAN_POINT ( 'NONE',  ( -3.510061880997908279, 5.032561185093348044, -1.627651354100000169 ) ) ;
#13676 = CARTESIAN_POINT ( 'NONE',  ( 24.95644072989999884, -14.30264549059999979, 230.6577119970000069 ) ) ;
#13677 = VERTEX_POINT ( 'NONE', #2578 ) ;
#13678 = CARTESIAN_POINT ( 'NONE',  ( 9.993285220779439371, -25.61999708228226069, 115.0000000000000000 ) ) ;
#13679 = EDGE_CURVE ( 'NONE', #7142, #22455, #20766, .T. ) ;
#13680 = CARTESIAN_POINT ( 'NONE',  ( -3.283272085064022239, -5.616145207998583189, -16.28182079290000672 ) ) ;
#13681 = CARTESIAN_POINT ( 'NONE',  ( 4.638687372303289536, 6.462009008183451364, -40.63090155201975762 ) ) ;
#13682 = VECTOR ( 'NONE', #22760, 1000.000000000000227 ) ;
#13683 = DIRECTION ( 'NONE',  ( -1.000000000000000000, 0.000000000000000000, -2.257144471330000330E-12 ) ) ;
#13684 = CARTESIAN_POINT ( 'NONE',  ( -7.999999999703424791, -29.80249410822368006, -29.47052640025566816 ) ) ;
#13685 = CARTESIAN_POINT ( 'NONE',  ( 1.127732790480000080, -28.47784299079999926, 225.0000014190000002 ) ) ;
#13686 = CARTESIAN_POINT ( 'NONE',  ( -27.65104932737173371, -3.057638586815402348, 8.000000000000007105 ) ) ;
#13687 = CARTESIAN_POINT ( 'NONE',  ( -2.758214512664866280, 2.222207457346479842, 227.6700655910688056 ) ) ;
#13688 = DIRECTION ( 'NONE',  ( -1.000000000000000000, 0.000000000000000000, 0.000000000000000000 ) ) ;
#13689 = DIRECTION ( 'NONE',  ( 0.5532886644841251700, 0.8329895880221872551, -0.000000000000000000 ) ) ;
#13690 = CARTESIAN_POINT ( 'NONE',  ( -10.00000000000000000, 19.99999999999999645, -42.39999999999999858 ) ) ;
#13691 = ADVANCED_FACE ( 'NONE', ( #2731 ), #12328, .F. ) ;
#13692 = DIRECTION ( 'NONE',  ( 1.000000000000000000, 0.000000000000000000, 0.000000000000000000 ) ) ;
#13693 = B_SPLINE_CURVE_WITH_KNOTS ( 'NONE', 5,
 ( #24017, #15299, #12620, #27104, #7019, #22232 ),
 .UNSPECIFIED., .F., .F.,
 ( 6, 6 ),
 ( -3.500000000000000000, -1.499999893000000029 ),
 .UNSPECIFIED. ) ;
#13694 = VERTEX_POINT ( 'NONE', #7748 ) ;
#13695 = CARTESIAN_POINT ( 'NONE',  ( 11.20000000009999930, -24.49999999969999820, -32.73012701864999485 ) ) ;
#13696 = CARTESIAN_POINT ( 'NONE',  ( 3.162589221723357991, -1.641472262613852262, -36.67856965541876946 ) ) ;
#13697 = AXIS2_PLACEMENT_3D ( 'NONE', #14480, #16982, #29518 ) ;
#13698 = CARTESIAN_POINT ( 'NONE',  ( 9.999999999949999108, -30.49251257979999963, -21.04205368479999905 ) ) ;
#13699 = VERTEX_POINT ( 'NONE', #19569 ) ;
#13700 = CARTESIAN_POINT ( 'NONE',  ( -1.557622931652903331, -4.259165208650873780, -44.38640794712500792 ) ) ;
#13701 = ORIENTED_EDGE ( 'NONE', *, *, #2892, .T. ) ;
#13702 = EDGE_CURVE ( 'NONE', #4180, #902, #14044, .T. ) ;
#13703 = ORIENTED_EDGE ( 'NONE', *, *, #26382, .T. ) ;
#13704 = ORIENTED_EDGE ( 'NONE', *, *, #25344, .T. ) ;
#13705 = LINE ( 'NONE', #11039, #14475 ) ;
#13706 = VERTEX_POINT ( 'NONE', #2881 ) ;
#13707 = AXIS2_PLACEMENT_3D ( 'NONE', #82, #11565, #16893 ) ;
#13708 = CARTESIAN_POINT ( 'NONE',  ( -2.962149026499999369E-14, -27.50000000069999828, 6.100000000000000533 ) ) ;
#13709 = CARTESIAN_POINT ( 'NONE',  ( -24.06750537087913600, -15.26514226587110379, 4.098700198000015504 ) ) ;
#13710 = B_SPLINE_CURVE_WITH_KNOTS ( 'NONE', 3,
 ( #28431, #23575, #16315, #28733, #28588, #16619 ),
 .UNSPECIFIED., .F., .F.,
 ( 4, 2, 4 ),
 ( 0.000000000000000000, 0.5000000000000000000, 1.000000000000000000 ),
 .UNSPECIFIED. ) ;
#13711 = CARTESIAN_POINT ( 'NONE',  ( 0.4125558677724673329, -28.49726274111925761, 3.904047916000019658 ) ) ;
#13712 = CARTESIAN_POINT ( 'NONE',  ( 14.77490805647873273, -21.99999999999999645, -29.54211979042643677 ) ) ;
#13713 = CARTESIAN_POINT ( 'NONE',  ( 23.61599683838066710, -12.66993935541866634, 5.719315393927735691 ) ) ;
#13714 = CARTESIAN_POINT ( 'NONE',  ( -0.6685465368700000965, -28.49273882800000024, 225.9009104920000084 ) ) ;
#13715 = EDGE_LOOP ( 'NONE', ( #15128, #24194, #25145, #4616 ) ) ;
#13716 = CARTESIAN_POINT ( 'NONE',  ( -2.624260084387262104, -3.463915187244965388, -4.228945369299999868 ) ) ;
#13717 = CARTESIAN_POINT ( 'NONE',  ( 5.195105410215491659, 3.969764343816663210, -22.76727430110000938 ) ) ;
#13718 = DIRECTION ( 'NONE',  ( -0.000000000000000000, -0.9396926207858126157, -0.3420201433259318913 ) ) ;
#13719 = CARTESIAN_POINT ( 'NONE',  ( -23.53911279557259206, -12.81252279922326132, 224.1183286170036411 ) ) ;
#13720 = CARTESIAN_POINT ( 'NONE',  ( 0.5453808542172137175, 3.499787565727434213, 227.6700655910692603 ) ) ;
#13721 = FACE_OUTER_BOUND ( 'NONE', #7282, .T. ) ;
#13722 = CARTESIAN_POINT ( 'NONE',  ( -24.04140365350000152, -13.95971772459999904, 226.0986578890000089 ) ) ;
#13723 = CARTESIAN_POINT ( 'NONE',  ( 5.414213562369999622, -30.60492699607083722, -82.14596754238048959 ) ) ;
#13724 = CARTESIAN_POINT ( 'NONE',  ( 1.533144572080375800, -28.45911136072489001, 5.506490228000010312 ) ) ;
#13725 = DIRECTION ( 'NONE',  ( -5.551115123049999208E-18, 3.153710283929999911E-31, -1.000000000000000000 ) ) ;
#13726 = EDGE_CURVE ( 'NONE', #19159, #8911, #5708, .T. ) ;
#13727 = ORIENTED_EDGE ( 'NONE', *, *, #13147, .F. ) ;
#13728 = CARTESIAN_POINT ( 'NONE',  ( -5.296314592117303377, -2.692763687817543161, -61.88424626872500056 ) ) ;
#13729 = VECTOR ( 'NONE', #17608, 1000.000000000000000 ) ;
#13730 = CARTESIAN_POINT ( 'NONE',  ( -24.41841039498785193, -14.69667350221323865, 6.099998581000020792 ) ) ;
#13731 = ORIENTED_EDGE ( 'NONE', *, *, #24858, .T. ) ;
#13732 = EDGE_CURVE ( 'NONE', #26662, #790, #20552, .T. ) ;
#13733 = CARTESIAN_POINT ( 'NONE',  ( 8.700000000274950906, -15.55224769787477257, -33.04262248272473812 ) ) ;
#13734 = CARTESIAN_POINT ( 'NONE',  ( 5.323890883912177685, 1.532987191732344767, -35.53910482770000812 ) ) ;
#13735 = ORIENTED_EDGE ( 'NONE', *, *, #22900, .T. ) ;
#13736 = ADVANCED_FACE ( 'NONE', ( #841 ), #15304, .T. ) ;
#13737 = DIRECTION ( 'NONE',  ( 0.000000000000000000, 0.000000000000000000, -1.000000000000000000 ) ) ;
#13738 = CARTESIAN_POINT ( 'NONE',  ( 1.638687372183706747, -17.80543024188206758, -28.79488058872038891 ) ) ;
#13739 = VERTEX_POINT ( 'NONE', #29929 ) ;
#13740 = ORIENTED_EDGE ( 'NONE', *, *, #13800, .F. ) ;
#13741 = ORIENTED_EDGE ( 'NONE', *, *, #19054, .F. ) ;
#13742 = LINE ( 'NONE', #25234, #16259 ) ;
#13743 = EDGE_LOOP ( 'NONE', ( #25075, #753, #12447, #2945 ) ) ;
#13744 = CARTESIAN_POINT ( 'NONE',  ( -12.30000000008458549, -27.41887902047864500, -31.60000000001083365 ) ) ;
#13745 = CARTESIAN_POINT ( 'NONE',  ( 23.34643930336224216, -14.53345043318084251, 4.357489521687117673 ) ) ;
#13746 = CARTESIAN_POINT ( 'NONE',  ( 1.644051155559919764, -5.677575162961061572, -67.70367649352500905 ) ) ;
#13747 = CIRCLE ( 'NONE', #13262, 1.700000000000000178 ) ;
#13748 = CARTESIAN_POINT ( 'NONE',  ( 25.41516571979999739, -14.56554165010000013, 229.1414211990000354 ) ) ;
#13749 = CARTESIAN_POINT ( 'NONE',  ( -10.00000000009184120, -24.60099947280526678, -30.24364015992614085 ) ) ;
#13750 = CARTESIAN_POINT ( 'NONE',  ( 8.000000000485913532, -30.00976070830145304, -28.70911655965779730 ) ) ;
#13751 = CARTESIAN_POINT ( 'NONE',  ( -23.20948082139999968, -13.40000000000000036, 6.099999999630000502 ) ) ;
#13752 = ORIENTED_EDGE ( 'NONE', *, *, #26577, .F. ) ;
#13753 = CARTESIAN_POINT ( 'NONE',  ( -23.20948082139999968, -13.40000000000000036, 226.0999999999999943 ) ) ;
#13754 = CARTESIAN_POINT ( 'NONE',  ( 5.466312515054250198, -2.792605348973308477, -11.91474735220000092 ) ) ;
#13755 = DIRECTION ( 'NONE',  ( 0.000000000000000000, 0.000000000000000000, 1.000000000000000000 ) ) ;
#13756 = DIRECTION ( 'NONE',  ( -0.000000000000000000, -0.000000000000000000, -1.000000000000000000 ) ) ;
#13757 = ORIENTED_EDGE ( 'NONE', *, *, #623, .T. ) ;
#13758 = CARTESIAN_POINT ( 'NONE',  ( 26.80000000069999899, -3.281945028320000125E-15, 211.6085707940000020 ) ) ;
#13759 = FACE_OUTER_BOUND ( 'NONE', #30252, .T. ) ;
#13760 = CARTESIAN_POINT ( 'NONE',  ( -23.14178524820000149, 15.40497058279999898, 222.0000000000000000 ) ) ;
#13761 = CARTESIAN_POINT ( 'NONE',  ( 26.42504859323178934, 9.566195259927013694, 0.2686740800000309015 ) ) ;
#13762 = DIRECTION ( 'NONE',  ( 0.000000000000000000, 1.000000000000000000, 0.000000000000000000 ) ) ;
#13763 = CARTESIAN_POINT ( 'NONE',  ( 5.943504367937093136, -0.4395870339238064362, -49.12442242802499948 ) ) ;
#13764 = CARTESIAN_POINT ( 'NONE',  ( 27.24857305730000334, -4.377319704760001142E-12, 229.9172022069999741 ) ) ;
#13765 = FACE_OUTER_BOUND ( 'NONE', #24926, .T. ) ;
#13766 = VECTOR ( 'NONE', #6375, 1000.000000000000000 ) ;
#13767 = ORIENTED_EDGE ( 'NONE', *, *, #22334, .T. ) ;
#13768 =( NAMED_UNIT ( * ) PLANE_ANGLE_UNIT ( ) SI_UNIT ( $, .RADIAN. ) );
#13769 = CARTESIAN_POINT ( 'NONE',  ( 27.79999999999999716, -2.355458807519999858E-11, 227.5999999999999943 ) ) ;
#13770 = AXIS2_PLACEMENT_3D ( 'NONE', #5827, #1115, #20155 ) ;
#13771 = CIRCLE ( 'NONE', #24303, 2.999999999999999556 ) ;
#13772 = AXIS2_PLACEMENT_3D ( 'NONE', #26446, #24548, #12273 ) ;
#13773 = CARTESIAN_POINT ( 'NONE',  ( 1.905093263558854666, -3.704216562065955731, -68.10000000002500542 ) ) ;
#13774 = EDGE_CURVE ( 'NONE', #23742, #10372, #10433, .T. ) ;
#13775 = CARTESIAN_POINT ( 'NONE',  ( 1.682565990562016722, 2.345890382669250762, -68.02449527681511654 ) ) ;
#13776 = CARTESIAN_POINT ( 'NONE',  ( -24.08956650190513571, -13.26503430085140955, 225.9595466043619751 ) ) ;
#13777 =( LENGTH_UNIT ( ) NAMED_UNIT ( * ) SI_UNIT ( .MILLI., .METRE. ) );
#13778 = ORIENTED_EDGE ( 'NONE', *, *, #28078, .T. ) ;
#13779 = CARTESIAN_POINT ( 'NONE',  ( 3.441895497200000431, 11.73074891959999988, 232.6627635220000059 ) ) ;
#13780 = CARTESIAN_POINT ( 'NONE',  ( 2.833778097863427714, 3.583098331959792660, -63.63768011632500787 ) ) ;
#13781 = ORIENTED_EDGE ( 'NONE', *, *, #421, .F. ) ;
#13782 = CARTESIAN_POINT ( 'NONE',  ( 0.000000000000000000, 19.99999999999999645, -43.39999999999999858 ) ) ;
#13783 = CARTESIAN_POINT ( 'NONE',  ( -19.06889133170000150, 19.69230209619999883, 229.7995039799999972 ) ) ;
#13784 = ORIENTED_EDGE ( 'NONE', *, *, #17077, .F. ) ;
#13786 = LINE ( 'NONE', #18969, #10050 ) ;
#13785 = VECTOR ( 'NONE', #4908, 1000.000000000000114 ) ;
#13787 = VECTOR ( 'NONE', #24146, 1000.000000000000000 ) ;
#13788 = PLANE ( 'NONE',  #17553 ) ;
#13789 = AXIS2_PLACEMENT_3D ( 'NONE', #23188, #23348, #8688 ) ;
#13790 = CARTESIAN_POINT ( 'NONE',  ( 9.785465176140000665, 19.99999999999999645, -43.02073679144999829 ) ) ;
#13791 = CARTESIAN_POINT ( 'NONE',  ( -15.73360964030186970, 11.02001161816959396, -0.6999999999999784173 ) ) ;
#13792 = CIRCLE ( 'NONE', #242, 2.926829268290000119 ) ;
#13793 = CIRCLE ( 'NONE', #25873, 10.00564797610000056 ) ;
#13794 = CARTESIAN_POINT ( 'NONE',  ( 0.4713258872182368164, -27.79624559782057602, 3.899998581000013509 ) ) ;
#13795 = CARTESIAN_POINT ( 'NONE',  ( -12.30769945475813643, -22.00000000000000000, -28.62078513402536473 ) ) ;
#13796 = DIRECTION ( 'NONE',  ( 0.000000000000000000, 0.9396926207858125046, 0.3420201433259318358 ) ) ;
#13797 = VERTEX_POINT ( 'NONE', #29769 ) ;
#13798 = DIRECTION ( 'NONE',  ( -0.000000000000000000, 0.000000000000000000, -1.000000000000000000 ) ) ;
#13799 = CARTESIAN_POINT ( 'NONE',  ( 4.213005042626035923, -2.798363829541613335, -35.30210069600008183 ) ) ;
#13800 = EDGE_CURVE ( 'NONE', #725, #6775, #24908, .T. ) ;
#13801 = CARTESIAN_POINT ( 'NONE',  ( 11.69999999989999928, -2.500000000000002220, -2.399999999999999467 ) ) ;
#13802 = CARTESIAN_POINT ( 'NONE',  ( -2.400053023227272764, -2.842866040671395922, 230.7188131565800404 ) ) ;
#13803 = B_SPLINE_CURVE_WITH_KNOTS ( 'NONE', 1,
 ( #29001, #19411 ),
 .UNSPECIFIED., .F., .F.,
 ( 2, 2 ),
 ( 1.257340414754434539E-07, 0.7036780443879999680 ),
 .UNSPECIFIED. ) ;
#13804 = CARTESIAN_POINT ( 'NONE',  ( -24.11911872370000154, -15.18353100999999938, 225.3106464589999973 ) ) ;
#13805 = CARTESIAN_POINT ( 'NONE',  ( -1.127665019380000189, -28.47796022459999676, 225.0000014190000002 ) ) ;
#13806 = CARTESIAN_POINT ( 'NONE',  ( 9.999999999969999109, -24.00000000000000000, -28.40000000000000213 ) ) ;
#13807 = CARTESIAN_POINT ( 'NONE',  ( 1.099998490678508523, -27.77839035186579508, 224.8530690857243428 ) ) ;
#13808 = CARTESIAN_POINT ( 'NONE',  ( -3.347225659292417888, -3.617661372292495514, -49.44612412472500296 ) ) ;
#13809 = ADVANCED_FACE ( 'NONE', ( #20462 ), #12303, .T. ) ;
#13810 = CARTESIAN_POINT ( 'NONE',  ( -20.30396346370000060, 20.00000000000000000, 227.3999999999999773 ) ) ;
#13811 = DIRECTION ( 'NONE',  ( -3.927995826131583318E-12, 0.4082287037029531107, 0.9128796883888953273 ) ) ;
#13812 = DIRECTION ( 'NONE',  ( -5.962915006522622422E-16, -0.4383711467890810676, -0.8987940462991651502 ) ) ;
#13813 = VECTOR ( 'NONE', #22407, 1000.000000000000000 ) ;
#13814 = AXIS2_PLACEMENT_3D ( 'NONE', #3654, #1311, #13250 ) ;
#13815 = DIRECTION ( 'NONE',  ( -1.000000000000000000, 5.687698019339887572E-16, -6.771501495046482653E-12 ) ) ;
#13816 = EDGE_LOOP ( 'NONE', ( #12309, #14837, #3395, #15424 ) ) ;
#13817 = CARTESIAN_POINT ( 'NONE',  ( -23.52673845780000050, -14.81058795080000046, 224.6893563800000209 ) ) ;
#13818 = VERTEX_POINT ( 'NONE', #20487 ) ;
#13819 = EDGE_CURVE ( 'NONE', #23829, #25281, #29731, .T. ) ;
#13820 = CARTESIAN_POINT ( 'NONE',  ( 2.752605500610146638, 3.655072764496610560, -55.02619010302499447 ) ) ;
#13821 = ORIENTED_EDGE ( 'NONE', *, *, #13450, .T. ) ;
#13822 = PRODUCT_CONTEXT ( 'NONE', #10172, 'mechanical' ) ;
#13823 = ORIENTED_EDGE ( 'NONE', *, *, #13910, .T. ) ;
#13824 = CARTESIAN_POINT ( 'NONE',  ( 26.80000000000000071, -1.776356839399999804E-15, 43.21714158840000408 ) ) ;
#13825 = ORIENTED_EDGE ( 'NONE', *, *, #21502, .T. ) ;
#13826 = VECTOR ( 'NONE', #13832, 1000.000000000000000 ) ;
#13827 = COLOUR_RGB ( '', 0.31764706, 0.68627451, 0.89019608) ;
#13828 = LINE ( 'NONE', #19006, #26244 ) ;
#13829 = FACE_OUTER_BOUND ( 'NONE', #25981, .T. ) ;
#13830 = CARTESIAN_POINT ( 'NONE',  ( -17.44301831181996221, -30.31831338603490167, -24.54232643498374244 ) ) ;
#13831 = B_SPLINE_CURVE_WITH_KNOTS ( 'NONE', 5,
 ( #22696, #24909, #27884, #25211, #27718, #17649 ),
 .UNSPECIFIED., .F., .F.,
 ( 6, 6 ),
 ( 0.000000000000000000, 2.300779717540000213 ),
 .UNSPECIFIED. ) ;
#13832 = DIRECTION ( 'NONE',  ( -1.000000000000000000, 5.687697999151106851E-16, -6.771501495036750356E-12 ) ) ;
#13833 = FACE_OUTER_BOUND ( 'NONE', #1637, .T. ) ;
#13834 = CARTESIAN_POINT ( 'NONE',  ( 27.50000000000000000, -3.367667472999999580E-15, 93.60555127639999284 ) ) ;
#13835 = CARTESIAN_POINT ( 'NONE',  ( -6.505526340832360255, -0.4164809035307331930, -4.148838774900000637 ) ) ;
#13836 = CARTESIAN_POINT ( 'NONE',  ( -13.87066093029999969, -27.85049402390000139, 230.2432540810000319 ) ) ;
#13837 = ORIENTED_EDGE ( 'NONE', *, *, #24595, .F. ) ;
#13838 = DIRECTION ( 'NONE',  ( -0.000000000000000000, -0.9396926207858126157, -0.3420201433259318913 ) ) ;
#13839 = AXIS2_PLACEMENT_3D ( 'NONE', #10562, #29441, #26937 ) ;
#13840 = EDGE_CURVE ( 'NONE', #8329, #8607, #8201, .T. ) ;
#13841 = CARTESIAN_POINT ( 'NONE',  ( 3.082386449366550707, -3.056625787687244689, -15.56112212870000278 ) ) ;
#13842 = CARTESIAN_POINT ( 'NONE',  ( 3.123710955063047745, -2.074832491810059132, -35.45875473019999902 ) ) ;
#13843 = CARTESIAN_POINT ( 'NONE',  ( 23.81866167241657806, 14.33570040768432996, 3.899998581000013509 ) ) ;
#13844 = DIRECTION ( 'NONE',  ( 1.000000000000000000, -9.219545062029677348E-13, 4.710284450064082408E-12 ) ) ;
#13845 = CARTESIAN_POINT ( 'NONE',  ( -27.73177265635928990, -2.208742311170187378, 8.000000000000007105 ) ) ;
#13846 = CARTESIAN_POINT ( 'NONE',  ( -2.719334904039233169, 2.289552478158404902, 227.6774647154331319 ) ) ;
#13847 = CARTESIAN_POINT ( 'NONE',  ( 28.40974773466432168, 5.219434544874079762, 1.000000000000000888 ) ) ;
#13848 = DIRECTION ( 'NONE',  ( 0.000000000000000000, 0.000000000000000000, 1.000000000000000000 ) ) ;
#13849 = CARTESIAN_POINT ( 'NONE',  ( -17.93324555120827668, 10.97998838178171432, -1.000005633855494125E-09 ) ) ;
#13850 = AXIS2_PLACEMENT_3D ( 'NONE', #19665, #24543, #22491 ) ;
#13851 = EDGE_CURVE ( 'NONE', #8033, #26188, #27434, .T. ) ;
#13852 = EDGE_CURVE ( 'NONE', #28717, #15209, #29327, .T. ) ;
#13853 = DIRECTION ( 'NONE',  ( -1.224606353819999829E-16, -1.000000000000000000, 0.000000000000000000 ) ) ;
#13854 = EDGE_LOOP ( 'NONE', ( #23805, #20940 ) ) ;
#13855 = CARTESIAN_POINT ( 'NONE',  ( -17.69076634382037838, -8.309652824054660769, 0.000000000000000000 ) ) ;
#13856 = CARTESIAN_POINT ( 'NONE',  ( -8.000000000050000892, -13.30122639390952877, -75.84793558053411289 ) ) ;
#13857 = ORIENTED_EDGE ( 'NONE', *, *, #30558, .T. ) ;
#13858 = B_SPLINE_CURVE_WITH_KNOTS ( 'NONE', 5,
 ( #22601, #1626, #1041, #11217, #20817, #18450 ),
 .UNSPECIFIED., .F., .F.,
 ( 6, 6 ),
 ( 0.000000000000000000, 18.03450582460000007 ),
 .UNSPECIFIED. ) ;
#13859 = CARTESIAN_POINT ( 'NONE',  ( -5.534792526179823646, -1.995162464570431782, -45.21497819512499916 ) ) ;
#13860 = ORIENTED_EDGE ( 'NONE', *, *, #6289, .T. ) ;
#13861 = ORIENTED_EDGE ( 'NONE', *, *, #23979, .T. ) ;
#13862 = EDGE_CURVE ( 'NONE', #10144, #6778, #28943, .T. ) ;
#13863 =( NAMED_UNIT ( * ) SI_UNIT ( $, .STERADIAN. ) SOLID_ANGLE_UNIT ( ) );
#13864 = VERTEX_POINT ( 'NONE', #17648 ) ;
#13865 = CARTESIAN_POINT ( 'NONE',  ( 22.18615130530000101, 17.78888133539999927, 230.2432540810000319 ) ) ;
#13866 = EDGE_LOOP ( 'NONE', ( #17063, #16368, #25975, #26015, #12467, #4500 ) ) ;
#13867 = CARTESIAN_POINT ( 'NONE',  ( 10.69999999999999929, -29.12132034360000077, -30.52132034359999935 ) ) ;
#13868 = CARTESIAN_POINT ( 'NONE',  ( 24.16679028237082960, 15.10730797463399000, 3.997250016000014838 ) ) ;
#13869 = DIRECTION ( 'NONE',  ( -1.000000000000000000, 5.687697999151106851E-16, -6.771501495036750356E-12 ) ) ;
#13870 = DIRECTION ( 'NONE',  ( -1.000000000000000000, 5.665498452320000818E-16, 0.000000000000000000 ) ) ;
#13871 = CARTESIAN_POINT ( 'NONE',  ( -0.6094664100040195764, -28.49364619262437870, 4.999998581000003384 ) ) ;
#13872 = ADVANCED_FACE ( 'NONE', ( #15455 ), #20178, .F. ) ;
#13873 = FACE_OUTER_BOUND ( 'NONE', #15321, .T. ) ;
#13874 = CARTESIAN_POINT ( 'NONE',  ( 2.487884123742928111, -2.690858294336446743, 227.7407790647027923 ) ) ;
#13875 = DIRECTION ( 'NONE',  ( -0.6941258031311203780, -0.7198537139083029945, 0.000000000000000000 ) ) ;
#13876 = EDGE_LOOP ( 'NONE', ( #3823, #25783, #21996, #24272 ) ) ;
#13877 = CARTESIAN_POINT ( 'NONE',  ( -3.324062773583611907, -4.387625903868788591, -4.728945369300002532 ) ) ;
#13878 = CARTESIAN_POINT ( 'NONE',  ( 4.725722714813314518, -3.873618144263061946, -23.39674734060000105 ) ) ;
#13879 = CARTESIAN_POINT ( 'NONE',  ( 23.81569860410000317, -13.75000000000000000, 226.0999999999999943 ) ) ;
#13880 = CARTESIAN_POINT ( 'NONE',  ( -23.63672937765306159, -12.63153181569432881, 224.3233986254962815 ) ) ;
#13881 = CARTESIAN_POINT ( 'NONE',  ( 17.16657240490000191, -8.999999999699998199, -0.6999999999999992895 ) ) ;
#13882 = CARTESIAN_POINT ( 'NONE',  ( -3.703718188677836753, -21.27776243144296586, -30.43911684297082232 ) ) ;
#13883 = LINE ( 'NONE', #21122, #20856 ) ;
#13884 = EDGE_CURVE ( 'NONE', #5307, #28386, #2460, .T. ) ;
#13885 = DIRECTION ( 'NONE',  ( 0.000000000000000000, 0.000000000000000000, -1.000000000000000000 ) ) ;
#13886 = CARTESIAN_POINT ( 'NONE',  ( 7.611688852352022749, -5.971102853732826787, -34.56686771967835625 ) ) ;
#13887 = CARTESIAN_POINT ( 'NONE',  ( -10.00000000038429704, -25.59790977654974142, -12.29094066695284226 ) ) ;
#13888 = VERTEX_POINT ( 'NONE', #5698 ) ;
#13889 = CARTESIAN_POINT ( 'NONE',  ( -1.494970809075166329, -6.161113191638062148, -61.46311227092499507 ) ) ;
#13890 = CARTESIAN_POINT ( 'NONE',  ( -18.32611925129999975, 20.54576746559999734, 229.7313256839999838 ) ) ;
#13891 = ORIENTED_EDGE ( 'NONE', *, *, #10403, .T. ) ;
#13892 = ORIENTED_EDGE ( 'NONE', *, *, #13884, .T. ) ;
#13893 = DIRECTION ( 'NONE',  ( -0.000000000000000000, -0.000000000000000000, 1.000000000000000000 ) ) ;
#13894 = CARTESIAN_POINT ( 'NONE',  ( 2.831388952324535691, -5.386915550550475551, -33.20721934060000535 ) ) ;
#13895 = ORIENTED_EDGE ( 'NONE', *, *, #1586, .T. ) ;
#13896 = B_SPLINE_CURVE_WITH_KNOTS ( 'NONE', 5,
 ( #30981, #14310, #28461, #9413, #14309, #26110, #14150, #16498, #28763, #25955, #30827, #23915, #2350, #21390, #2195 ),
 .UNSPECIFIED., .F., .F.,
 ( 6, 3, 3, 3, 6 ),
 ( 0.000000000000000000, 0.09999999999942736639, 0.3999999999977094656, 0.7000000000000000666, 1.000000000000000000 ),
 .UNSPECIFIED. ) ;
#13897 = B_SPLINE_CURVE_WITH_KNOTS ( 'NONE', 3,
 ( #16664, #16361, #23928, #28776, #2365, #11950 ),
 .UNSPECIFIED., .F., .F.,
 ( 4, 2, 4 ),
 ( 0.000000000000000000, 0.5000000000000000000, 1.000000000000000000 ),
 .UNSPECIFIED. ) ;
#13898 = EDGE_CURVE ( 'NONE', #8911, #29654, #1197, .T. ) ;
#13899 = CARTESIAN_POINT ( 'NONE',  ( -6.999999999595749145, -114.9756814440741124, 22.27940384897737403 ) ) ;
#13900 = CARTESIAN_POINT ( 'NONE',  ( -7.000000000000000000, -15.86465192213301556, -74.65259062561435144 ) ) ;
#13901 = VERTEX_POINT ( 'NONE', #30831 ) ;
#13902 = ORIENTED_EDGE ( 'NONE', *, *, #13273, .F. ) ;
#13903 = EDGE_LOOP ( 'NONE', ( #21333, #10958, #7724 ) ) ;
#13904 = ORIENTED_EDGE ( 'NONE', *, *, #402, .T. ) ;
#13905 = CARTESIAN_POINT ( 'NONE',  ( 24.52721838744800920, -14.51532614964689394, 5.760265122000007842 ) ) ;
#13906 = PLANE ( 'NONE',  #3396 ) ;
#13907 = CARTESIAN_POINT ( 'NONE',  ( -3.200877993934844401, 3.183711413074225671, -68.54322600212499594 ) ) ;
#13908 = CARTESIAN_POINT ( 'NONE',  ( 27.79999999999999716, 2.355449169040000061E-11, 229.1414213560000235 ) ) ;
#13909 = CARTESIAN_POINT ( 'NONE',  ( -1.071233843433221589, -26.77863813582381525, 224.7119040166546995 ) ) ;
#13910 = EDGE_CURVE ( 'NONE', #29055, #17565, #6327, .T. ) ;
#13911 = CARTESIAN_POINT ( 'NONE',  ( 28.50002393070000295, -9.769962616699999258E-14, 222.0000000000000000 ) ) ;
#13912 = CARTESIAN_POINT ( 'NONE',  ( -19.80535397421925481, 19.50875616500616871, 0.9999999989999952543 ) ) ;
#13913 = EDGE_LOOP ( 'NONE', ( #13704, #18249, #28787, #1134 ) ) ;
#13914 = CARTESIAN_POINT ( 'NONE',  ( -22.65536946396631279, -14.31703147662669018, 225.2878164648193149 ) ) ;
#13915 = EDGE_CURVE ( 'NONE', #11379, #7420, #22603, .T. ) ;
#13916 = CARTESIAN_POINT ( 'NONE',  ( 3.904356169178446745, -3.871725997715349532, -14.06112212870000455 ) ) ;
#13917 = CARTESIAN_POINT ( 'NONE',  ( 21.30571717078112215, -16.35234564651914013, -0.000000000000000000 ) ) ;
#13918 = B_SPLINE_CURVE_WITH_KNOTS ( 'NONE', 3,
 ( #18672, #30333, #11601, #11293 ),
 .UNSPECIFIED., .F., .F.,
 ( 4, 4 ),
 ( 0.000000000000000000, 1.000000000000000000 ),
 .UNSPECIFIED. ) ;
#13919 = CARTESIAN_POINT ( 'NONE',  ( -10.69999999968107041, -25.38784894342604659, -31.19578670632331097 ) ) ;
#13920 = ORIENTED_EDGE ( 'NONE', *, *, #25159, .F. ) ;
#13921 = B_SPLINE_CURVE_WITH_KNOTS ( 'NONE', 5,
 ( #22741, #3378, #20534, #1660, #8880, #20694, #12983, #13447, #15499, #22596, #15650, #28083, #30292, #18163, #1036 ),
 .UNSPECIFIED., .F., .F.,
 ( 6, 3, 3, 3, 6 ),
 ( 0.000000000000000000, 0.1000000000011452422, 0.3999999999988547161, 0.7000000000011451506, 1.000000000000000000 ),
 .UNSPECIFIED. ) ;
#13922 = PLANE ( 'NONE',  #25757 ) ;
#13923 = FACE_OUTER_BOUND ( 'NONE', #26332, .T. ) ;
#13924 = CARTESIAN_POINT ( 'NONE',  ( -27.16600648770000248, 9.122293387490000072, 222.0000000000000000 ) ) ;
#13925 = DIRECTION ( 'NONE',  ( 0.000000000000000000, 0.3420201433259318358, -0.9396926207858125046 ) ) ;
#13926 = CARTESIAN_POINT ( 'NONE',  ( 11.69999999989999928, -24.11120071670000087, -1.399999999299995856 ) ) ;
#13927 = CARTESIAN_POINT ( 'NONE',  ( -1.494970809075166329, -6.161113191638062148, -61.94311227092499195 ) ) ;
#13928 = CARTESIAN_POINT ( 'NONE',  ( 10.69999999999999929, -24.87867965640000278, -26.27867965640000136 ) ) ;
#13929 = PLANE ( 'NONE',  #20287 ) ;
#13930 = VERTEX_POINT ( 'NONE', #26424 ) ;
#13931 = CARTESIAN_POINT ( 'NONE',  ( 0.000000000000000000, 0.000000000000000000, 20.00000000000000355 ) ) ;
#13932 = DIRECTION ( 'NONE',  ( 1.000000000000000000, -1.843431230200084908E-12, 2.650498504963248473E-12 ) ) ;
#13933 = CARTESIAN_POINT ( 'NONE',  ( 2.739374102630459884, -3.445395115450355483, -68.10000000002501963 ) ) ;
#13934 = PRODUCT ( 'Moving Handle', 'Moving Handle', '', ( #23269 ) ) ;
#13935 = AXIS2_PLACEMENT_3D ( 'NONE', #2304, #18807, #9528 ) ;
#13936 = LINE ( 'NONE', #20703, #18270 ) ;
#13937 = CARTESIAN_POINT ( 'NONE',  ( 10.06596365874881194, -25.80632433378973900, 90.00000000000000000 ) ) ;
#13938 = AXIS2_PLACEMENT_3D ( 'NONE', #459, #14458, #16494 ) ;
#13939 = ORIENTED_EDGE ( 'NONE', *, *, #19458, .F. ) ;
#13940 = CARTESIAN_POINT ( 'NONE',  ( 10.46457122910000059, 21.70000000000000284, -54.63542873130000288 ) ) ;
#13941 = CARTESIAN_POINT ( 'NONE',  ( -2.911316102860724175, -3.927725552502973727, -65.13409070562501313 ) ) ;
#13942 = ORIENTED_EDGE ( 'NONE', *, *, #2380, .F. ) ;
#13943 = CARTESIAN_POINT ( 'NONE',  ( 24.82523534259457421, -12.51291187729028742, 4.710542421340364605 ) ) ;
#13944 = CARTESIAN_POINT ( 'NONE',  ( 3.181902231748806376, -1.609514238137543796, -88.52261276306772686 ) ) ;
#13945 = EDGE_CURVE ( 'NONE', #11888, #1366, #10948, .T. ) ;
#13946 = VERTEX_POINT ( 'NONE', #21700 ) ;
#13947 = CARTESIAN_POINT ( 'NONE',  ( -5.799375405960000229, -1.094484689610000006, 226.6412452697800006 ) ) ;
#13948 = SURFACE_STYLE_USAGE ( .BOTH. , #9209 ) ;
#13949 = CARTESIAN_POINT ( 'NONE',  ( -12.57879864068154774, 21.69999999999986784, -55.96236416640539346 ) ) ;
#13950 = CARTESIAN_POINT ( 'NONE',  ( 10.69999999993204653, -25.59803261866920465, -12.29454957252203151 ) ) ;
#13951 = B_SPLINE_SURFACE_WITH_KNOTS ( 'NONE', 5, 1, ( 
 ( #19622, #24499 ),
 ( #2630, #9558 ),
 ( #26855, #24041 ),
 ( #12222, #12072 ),
 ( #26402, #21832 ),
 ( #5302, #19315 ),
 ( #15057, #14904 ),
 ( #2937, #12530 ),
 ( #21679, #292 ),
 ( #22138, #9869 ),
 ( #29060, #595 ),
 ( #10179, #19779 ),
 ( #29361, #7805 ),
 ( #17404, #27009 ),
 ( #5450, #30144 ) ),
 .UNSPECIFIED., .F., .F., .F.,
 ( 6, 3, 3, 3, 6 ),
 ( 2, 2 ),
 ( 0.000000000000000000, 0.5239010162220000266, 1.047802032450000143, 1.571703048660000102, 1.746336720740000015 ),
 ( -0.7000000000009999335, 2.556026448610000073E-06 ),
 .UNSPECIFIED. ) ;
#13952 = CARTESIAN_POINT ( 'NONE',  ( -0.5944614571882205212, -27.79380703160649446, 4.999998581000003384 ) ) ;
#13953 = EDGE_CURVE ( 'NONE', #14643, #13982, #2043, .T. ) ;
#13954 = AXIS2_PLACEMENT_3D ( 'NONE', #28455, #23750, #6890 ) ;
#13955 = CARTESIAN_POINT ( 'NONE',  ( 8.198872691879999995E-10, -3.797984149399999816E-10, 229.6412452697800006 ) ) ;
#13956 = EDGE_CURVE ( 'NONE', #14873, #10703, #8673, .T. ) ;
#13957 = DIRECTION ( 'NONE',  ( 1.000000000000000000, -3.981000000000000101E-12, 1.940999999999999908E-12 ) ) ;
#13958 = ORIENTED_EDGE ( 'NONE', *, *, #13585, .T. ) ;
#13959 = DIRECTION ( 'NONE',  ( 1.000000000000000000, 0.000000000000000000, 0.000000000000000000 ) ) ;
#13960 = CARTESIAN_POINT ( 'NONE',  ( 4.276011752548591005, -51.11187400310260642, -27.80500476121942199 ) ) ;
#13961 = CARTESIAN_POINT ( 'NONE',  ( 18.15340080560000047, 19.92139761430000178, 229.9929672670000116 ) ) ;
#13962 = CIRCLE ( 'NONE', #7894, 27.92857142820000149 ) ;
#13963 = DIRECTION ( 'NONE',  ( 3.084561942502618954E-12, 0.8902635789277789646, -0.4554456718805243165 ) ) ;
#13964 = CARTESIAN_POINT ( 'NONE',  ( 1.871217339555081960, 11.95683682116809265, 232.0000000000053433 ) ) ;
#13965 = CARTESIAN_POINT ( 'NONE',  ( -0.4702726639020000099, -27.79650200060000031, 226.0025182780000250 ) ) ;
#13966 = TOROIDAL_SURFACE ( 'NONE', #28532, 24.50000000000000000, 4.000000000000000000 ) ;
#13967 = CARTESIAN_POINT ( 'NONE',  ( -15.93711909997440301, 10.34626908942863466, -1.400000000000002132 ) ) ;
#13968 = CARTESIAN_POINT ( 'NONE',  ( 2.097865490181829884, -3.779070126327673140, -55.58172062782499268 ) ) ;
#13969 = CARTESIAN_POINT ( 'NONE',  ( -20.30396346370000060, 20.00000000000000000, 229.0000000000000000 ) ) ;
#13970 = LINE ( 'NONE', #18203, #27372 ) ;
#13971 = CARTESIAN_POINT ( 'NONE',  ( 17.16657240421717390, -9.000000000001264766, -0.6999999999999784173 ) ) ;
#13972 = CIRCLE ( 'NONE', #20029, 2.000000000000000000 ) ;
#13973 = CARTESIAN_POINT ( 'NONE',  ( 11.69999999989999928, -2.055600358200002198, -1.399999999999998579 ) ) ;
#13974 = LINE ( 'NONE', #26243, #10945 ) ;
#13975 = AXIS2_PLACEMENT_3D ( 'NONE', #27911, #26022, #59 ) ;
#13976 = VERTEX_POINT ( 'NONE', #14153 ) ;
#13977 = CARTESIAN_POINT ( 'NONE',  ( 6.136659917679837761, 0.6935318534637759935, -55.01771407622499765 ) ) ;
#13978 = EDGE_LOOP ( 'NONE', ( #9323, #3657, #2645, #16238 ) ) ;
#13979 = EDGE_CURVE ( 'NONE', #8755, #17736, #30053, .T. ) ;
#13980 = CIRCLE ( 'NONE', #5432, 17.61822726820000184 ) ;
#13981 = ITEM_DEFINED_TRANSFORMATION ( 'NONE', 'NONE', #1798,  #17722 ) ;
#13982 = VERTEX_POINT ( 'NONE', #3814 ) ;
#13984 = CARTESIAN_POINT ( 'NONE',  ( -11.83960380690999870, -27.00000000000000000, -28.40000000000771863 ) ) ;
#13983 = AXIS2_PLACEMENT_3D ( 'NONE', #26193, #16434, #25893 ) ;
#13985 = ORIENTED_EDGE ( 'NONE', *, *, #23388, .T. ) ;
#13986 = CARTESIAN_POINT ( 'NONE',  ( 14.47923079777483579, -27.23176631820642868, -22.76030765420599167 ) ) ;
#13987 = DIRECTION ( 'NONE',  ( 0.000000000000000000, 0.000000000000000000, 1.000000000000000000 ) ) ;
#13988 = FACE_OUTER_BOUND ( 'NONE', #1084, .T. ) ;
#13989 = B_SPLINE_CURVE_WITH_KNOTS ( 'NONE', 3,
 ( #5625, #768, #13166, #10513, #20112, #22473, #3109, #22163, #15226, #10660 ),
 .UNSPECIFIED., .F., .F.,
 ( 4, 2, 2, 2, 4 ),
 ( 0.000000000000000000, 0.2499999999999998890, 0.4999999999999997780, 0.7499999999999998890, 1.000000000000000000 ),
 .UNSPECIFIED. ) ;
#13991 = LINE ( 'NONE', #23276, #13826 ) ;
#13990 = B_SPLINE_CURVE_WITH_KNOTS ( 'NONE', 3,
 ( #6479, #13567, #28191, #6329, #9305, #28349 ),
 .UNSPECIFIED., .F., .F.,
 ( 4, 2, 4 ),
 ( 0.000000000000000000, 0.5000000000000000000, 1.000000000000000000 ),
 .UNSPECIFIED. ) ;
#13992 = DIRECTION ( 'NONE',  ( 1.000000000000000000, -3.981000000000000101E-12, 1.940999999999999908E-12 ) ) ;
#13993 = CARTESIAN_POINT ( 'NONE',  ( 27.76135144259999876, -3.399672736709999763E-15, 92.33858589269999584 ) ) ;
#13994 = CARTESIAN_POINT ( 'NONE',  ( 4.528382002446963206, -1.659419471228278375, -4.898605321699998072 ) ) ;
#13995 = CARTESIAN_POINT ( 'NONE',  ( -28.50000000000000000, -3.552713678799999608E-15, 229.0000000000000000 ) ) ;
#13996 = VERTEX_POINT ( 'NONE', #13565 ) ;
#13997 = CARTESIAN_POINT ( 'NONE',  ( 12.77819780750000156, 20.99999999999999645, -56.09999999999999432 ) ) ;
#13998 = CIRCLE ( 'NONE', #8975, 0.2500000000000002220 ) ;
#13999 = CARTESIAN_POINT ( 'NONE',  ( 4.543782907447139863, 1.343478130985185537, -18.47940840230000248 ) ) ;
#14000 = CARTESIAN_POINT ( 'NONE',  ( 0.1546076948784753102, 3.500000000000000000, 230.8358359828806954 ) ) ;
#14001 = CARTESIAN_POINT ( 'NONE',  ( -7.999999999826271413, -29.66236253007011925, -29.83737202115235121 ) ) ;
#14002 = CARTESIAN_POINT ( 'NONE',  ( -24.26052213770000066, -13.57583965319999919, 223.9574921340000060 ) ) ;
#14003 = CARTESIAN_POINT ( 'NONE',  ( -7.999999999631178582, -20.24958040245157420, -40.81349356744964751 ) ) ;
#14004 = LINE ( 'NONE', #25336, #12801 ) ;
#14005 = CARTESIAN_POINT ( 'NONE',  ( 28.26943722656857716, 5.193656719585778347, 0.2374258030000131470 ) ) ;
#14006 = DIRECTION ( 'NONE',  ( -0.7071067811865475727, -0.7071067811865475727, 0.000000000000000000 ) ) ;
#14007 = CARTESIAN_POINT ( 'NONE',  ( -9.999999999879573664, 20.00000000000001066, -42.66179938841035124 ) ) ;
#14008 = VECTOR ( 'NONE', #14224, 1000.000000000000000 ) ;
#14009 = EDGE_CURVE ( 'NONE', #27171, #21717, #17289, .T. ) ;
#14010 = ADVANCED_FACE ( 'NONE', ( #15763 ), #10495, .T. ) ;
#14011 = CARTESIAN_POINT ( 'NONE',  ( -12.84240556079365270, 21.69999999994267270, -69.50012576675229070 ) ) ;
#14012 = EDGE_LOOP ( 'NONE', ( #3040, #743, #3091, #26284 ) ) ;
#14013 = CARTESIAN_POINT ( 'NONE',  ( 8.700000000241654874, -24.19757157926353486, -27.32949869323976699 ) ) ;
#14014 = DIRECTION ( 'NONE',  ( 1.000000000000000000, 0.000000000000000000, 0.000000000000000000 ) ) ;
#14015 = DIRECTION ( 'NONE',  ( 0.000000000000000000, 0.000000000000000000, 1.000000000000000000 ) ) ;
#14016 = CARTESIAN_POINT ( 'NONE',  ( 1.211329632739529982, -4.999378637410044846, -0.6999988961696247403 ) ) ;
#14017 = ORIENTED_EDGE ( 'NONE', *, *, #3871, .F. ) ;
#14018 = FACE_OUTER_BOUND ( 'NONE', #1156, .T. ) ;
#14019 = ORIENTED_EDGE ( 'NONE', *, *, #18210, .T. ) ;
#14020 = EDGE_CURVE ( 'NONE', #17448, #12574, #18018, .T. ) ;
#14021 = VERTEX_POINT ( 'NONE', #11938 ) ;
#14022 = VECTOR ( 'NONE', #10471, 1000.000000000000000 ) ;
#14023 = ORIENTED_EDGE ( 'NONE', *, *, #12640, .T. ) ;
#14024 = CARTESIAN_POINT ( 'NONE',  ( -0.3831792618930000005, -28.49793954440000121, 223.9576764909999724 ) ) ;
#14025 = EDGE_LOOP ( 'NONE', ( #13035, #1675, #23904, #25263 ) ) ;
#14026 = CARTESIAN_POINT ( 'NONE',  ( 10.69999999996929141, -30.00000000000000355, -28.79453140544987377 ) ) ;
#14027 =( NAMED_UNIT ( * ) PLANE_ANGLE_UNIT ( ) SI_UNIT ( $, .RADIAN. ) );
#14028 = CARTESIAN_POINT ( 'NONE',  ( -23.94466870085087606, -15.45669659436210175, 4.319305392000011068 ) ) ;
#14029 = FACE_OUTER_BOUND ( 'NONE', #22082, .T. ) ;
#14030 = CARTESIAN_POINT ( 'NONE',  ( 20.03591075579414849, 19.99999599181853682, 0.2184197934767622973 ) ) ;
#14031 = AXIS2_PLACEMENT_3D ( 'NONE', #10280, #25057, #27261 ) ;
#14032 = CARTESIAN_POINT ( 'NONE',  ( 14.84786676130553573, -21.99999999999998934, -27.95750568651506995 ) ) ;
#14033 = CYLINDRICAL_SURFACE ( 'NONE', #30191, 1.099999999999999201 ) ;
#14034 = CARTESIAN_POINT ( 'NONE',  ( -18.22457532099999611, 20.00000143240000128, 230.6880575950000036 ) ) ;
#14035 = EDGE_CURVE ( 'NONE', #10061, #1204, #30846, .T. ) ;
#14036 = B_SPLINE_CURVE_WITH_KNOTS ( 'NONE', 3,
 ( #3636, #3961, #25686, #15754, #17945, #29763 ),
 .UNSPECIFIED., .F., .F.,
 ( 4, 2, 4 ),
 ( 0.000000000000000000, 0.5000000000000000000, 1.000000000000000000 ),
 .UNSPECIFIED. ) ;
#14037 = CARTESIAN_POINT ( 'NONE',  ( 2.032938288397245330, -5.563452252945958243, -7.260585232200002181 ) ) ;
#14038 = CARTESIAN_POINT ( 'NONE',  ( -3.834000099192893973, 2.652495916366584439, -25.46779765530001072 ) ) ;
#14039 = DIRECTION ( 'NONE',  ( 0.000000000000000000, 0.000000000000000000, 1.000000000000000000 ) ) ;
#14040 = CARTESIAN_POINT ( 'NONE',  ( -1.861312627829582400, -21.81692582113286960, -30.17614928725744150 ) ) ;
#14041 = DIRECTION ( 'NONE',  ( 0.000000000000000000, 0.000000000000000000, -1.000000000000000000 ) ) ;
#14042 = DIRECTION ( 'NONE',  ( 0.000000000000000000, 1.000000000000000000, 0.000000000000000000 ) ) ;
#14043 = DIRECTION ( 'NONE',  ( 0.3633921898465289901, 0.9316362575375348731, 4.336808689942014581E-15 ) ) ;
#14044 = CIRCLE ( 'NONE', #1975, 3.000000000000001332 ) ;
#14045 = CARTESIAN_POINT ( 'NONE',  ( 27.71720220739999974, 1.975538407690000167E-11, 229.4485730569999760 ) ) ;
#14046 = CARTESIAN_POINT ( 'NONE',  ( 1.344125205538966084, -28.46870209102001326, 5.759639119000015128 ) ) ;
#14047 = DIRECTION ( 'NONE',  ( -1.000000000000000000, -1.750660885084214717E-48, 4.045530494348897360E-18 ) ) ;
#14048 = EDGE_LOOP ( 'NONE', ( #30545, #9052, #18056, #26099 ) ) ;
#14049 = CARTESIAN_POINT ( 'NONE',  ( 4.508719565894415915, 1.847421675581904843, -60.89141554682500157 ) ) ;
#14050 = FACE_OUTER_BOUND ( 'NONE', #13913, .T. ) ;
#14051 = ORIENTED_EDGE ( 'NONE', *, *, #29648, .T. ) ;
#14052 = CARTESIAN_POINT ( 'NONE',  ( 17.95841148948556310, 10.23646161652002817, 0.000000000000000000 ) ) ;
#14053 = CARTESIAN_POINT ( 'NONE',  ( 4.420334067734101424, -4.199682076162645217, -30.05126389020000488 ) ) ;
#14054 = VECTOR ( 'NONE', #20680, 1000.000000000000114 ) ;
#14055 = EDGE_LOOP ( 'NONE', ( #4007, #30185, #20237, #1486 ) ) ;
#14056 = DIRECTION ( 'NONE',  ( 1.000000000000000000, 0.000000000000000000, 0.000000000000000000 ) ) ;
#14057 = FACE_OUTER_BOUND ( 'NONE', #3215, .T. ) ;
#14058 = ORIENTED_EDGE ( 'NONE', *, *, #30478, .F. ) ;
#14059 = VERTEX_POINT ( 'NONE', #7827 ) ;
#14060 = EDGE_CURVE ( 'NONE', #22441, #5682, #22012, .T. ) ;
#14061 = ORIENTED_EDGE ( 'NONE', *, *, #16777, .T. ) ;
#14062 = ORIENTED_EDGE ( 'NONE', *, *, #30416, .F. ) ;
#14063 = CARTESIAN_POINT ( 'NONE',  ( -12.29999999993107096, -25.38841926281313377, -31.19611644274446860 ) ) ;
#14064 = LINE ( 'NONE', #21143, #27716 ) ;
#14065 = CARTESIAN_POINT ( 'NONE',  ( 0.2444022557069394641, 3.892334458579130185, -69.35875473022500159 ) ) ;
#14066 = SURFACE_STYLE_USAGE ( .BOTH. , #4467 ) ;
#14067 = CARTESIAN_POINT ( 'NONE',  ( 24.60666973300000038, -12.93650480179999995, 225.0000014190000002 ) ) ;
#14068 = CARTESIAN_POINT ( 'NONE',  ( -18.90269220160000430, -21.67466784369999644, 222.0000000000000000 ) ) ;
#14069 = ADVANCED_FACE ( 'NONE', ( #618 ), #26572, .T. ) ;
#14070 = CARTESIAN_POINT ( 'NONE',  ( 5.228794157972393997, -0.4992892829921782849, -35.69999999999999574 ) ) ;
#14071 = ORIENTED_EDGE ( 'NONE', *, *, #1945, .T. ) ;
#14072 = CARTESIAN_POINT ( 'NONE',  ( -20.14786743110572687, 20.00017459112578067, 0.3952317461953371303 ) ) ;
#14073 = EDGE_CURVE ( 'NONE', #16100, #21330, #19338, .T. ) ;
#14074 = CIRCLE ( 'NONE', #25625, 26.80000000000000071 ) ;
#14075 = CARTESIAN_POINT ( 'NONE',  ( 1.387648159808044790, -4.113210426322153168, -14.76414732020000287 ) ) ;
#14076 = CARTESIAN_POINT ( 'NONE',  ( 23.26050567054135243, -13.42703864535239155, -0.000000000000000000 ) ) ;
#14077 = ADVANCED_FACE ( 'NONE', ( #2809 ), #18532, .F. ) ;
#14078 = CARTESIAN_POINT ( 'NONE',  ( -10.69999999968668192, -29.55943383853203699, -30.36614888214831609 ) ) ;
#14079 = VERTEX_POINT ( 'NONE', #15224 ) ;
#14080 = CARTESIAN_POINT ( 'NONE',  ( -23.81866442513186755, -14.33570206443695838, 3.899998581000013509 ) ) ;
#14081 = DIRECTION ( 'NONE',  ( -1.000000000000000000, 0.000000000000000000, -6.771000000000000128E-12 ) ) ;
#14082 = CARTESIAN_POINT ( 'NONE',  ( -8.699999999684717267, -16.53542210648553024, -33.08054445275527655 ) ) ;
#14083 = EDGE_CURVE ( 'NONE', #29242, #15627, #14687, .T. ) ;
#14084 = CARTESIAN_POINT ( 'NONE',  ( -23.81569860410000317, -13.75000000000000000, 3.900000000369999942 ) ) ;
#14085 = CARTESIAN_POINT ( 'NONE',  ( -4.069925668896384963, 4.914984763948436530, -62.99933298482500277 ) ) ;
#14086 = CARTESIAN_POINT ( 'NONE',  ( 9.999999999959999997, -24.97510463849999951, -26.18619911149999879 ) ) ;
#14087 = FACE_OUTER_BOUND ( 'NONE', #16090, .T. ) ;
#14088 = ORIENTED_EDGE ( 'NONE', *, *, #15585, .T. ) ;
#14089 = CARTESIAN_POINT ( 'NONE',  ( -10.69999999999999929, -24.09288384250000092, -29.20409973919999658 ) ) ;
#14090 = CARTESIAN_POINT ( 'NONE',  ( -7.999999999662342987, -18.41955439558022078, -35.96306069475997447 ) ) ;
#14091 = CARTESIAN_POINT ( 'NONE',  ( 0.3358324584398617585, -5.008269611061795246, -68.10000000002501963 ) ) ;
#14092 = EDGE_CURVE ( 'NONE', #11652, #30584, #18057, .T. ) ;
#14093 = CARTESIAN_POINT ( 'NONE',  ( -7.163948298641449774, 5.500083906749039464, -40.16173933229066506 ) ) ;
#14094 = AXIS2_PLACEMENT_3D ( 'NONE', #30119, #18147, #27751 ) ;
#14095 = DIRECTION ( 'NONE',  ( 0.000000000000000000, 0.000000000000000000, 1.000000000000000000 ) ) ;
#14096 = CARTESIAN_POINT ( 'NONE',  ( 5.480456702449999717, 10.74539518949999994, 230.6412452697800006 ) ) ;
#14097 = ORIENTED_EDGE ( 'NONE', *, *, #23384, .F. ) ;
#14098 = CARTESIAN_POINT ( 'NONE',  ( 3.063879268240000009, 1.673804873600000187, 227.6412452699999847 ) ) ;
#14099 = CARTESIAN_POINT ( 'NONE',  ( -1.895255389310859684, 5.229048247678121264, -69.15099036452500059 ) ) ;
#14100 = EDGE_LOOP ( 'NONE', ( #2145, #30663, #24232, #9768 ) ) ;
#14101 = EDGE_CURVE ( 'NONE', #18566, #27661, #12867, .T. ) ;
#14102 = CYLINDRICAL_SURFACE ( 'NONE', #10404, 8.000000000000000000 ) ;
#14103 = CARTESIAN_POINT ( 'NONE',  ( -27.71261514784184499, -0.5042418799608706648, 0.5514269430000329208 ) ) ;
#14104 = EDGE_LOOP ( 'NONE', ( #30543, #22266, #21645, #8523 ) ) ;
#14105 = DIRECTION ( 'NONE',  ( 0.000000000000000000, -1.000000000000000000, 0.000000000000000000 ) ) ;
#14106 = CARTESIAN_POINT ( 'NONE',  ( -23.62421573606080827, -14.65442406347138338, 3.957526371000025023 ) ) ;
#14107 = CARTESIAN_POINT ( 'NONE',  ( -8.699999999667697992, -18.43894776734996910, -35.13584674166673949 ) ) ;
#14108 = CARTESIAN_POINT ( 'NONE',  ( -10.69999999999999929, -24.00000000000000000, -28.06060480569999882 ) ) ;
#14109 = B_SPLINE_CURVE_WITH_KNOTS ( 'NONE', 3,
 ( #10705, #3156, #10873, #29905, #12757, #3462 ),
 .UNSPECIFIED., .F., .F.,
 ( 4, 2, 4 ),
 ( 0.000000000000000000, 0.5000000000000000000, 1.000000000000000000 ),
 .UNSPECIFIED. ) ;
#14110 = DIRECTION ( 'NONE',  ( 0.000000000000000000, 0.3420201433259318358, -0.9396926207858125046 ) ) ;
#14111 = FACE_OUTER_BOUND ( 'NONE', #21884, .T. ) ;
#14112 = ORIENTED_EDGE ( 'NONE', *, *, #412, .F. ) ;
#14113 = CARTESIAN_POINT ( 'NONE',  ( -7.707106781243226123, -115.2381289094444128, 21.69251968763726879 ) ) ;
#14114 = CARTESIAN_POINT ( 'NONE',  ( -10.69999999969999926, -33.00000000000000000, -28.40000000000000213 ) ) ;
#14115 = CARTESIAN_POINT ( 'NONE',  ( 18.62327035899999572, 19.80375215579999804, 229.9327584799999897 ) ) ;
#14116 = DIRECTION ( 'NONE',  ( 0.000000000000000000, 0.000000000000000000, 1.000000000000000000 ) ) ;
#14117 = DIRECTION ( 'NONE',  ( 1.000000000000000000, 0.000000000000000000, 0.000000000000000000 ) ) ;
#14118 = CARTESIAN_POINT ( 'NONE',  ( -0.1033151399490000039, -27.80006701330000141, 226.0959516479999820 ) ) ;
#14119 = CARTESIAN_POINT ( 'NONE',  ( -24.93720648713954446, 13.79881813474513486, 3.899998581000013509 ) ) ;
#14120 = CARTESIAN_POINT ( 'NONE',  ( 23.79608325624482745, -14.37377491939586349, 225.9639575250533881 ) ) ;
#14121 = CARTESIAN_POINT ( 'NONE',  ( -0.9606962270921406422, -4.447130805931738706, -55.93033560642499680 ) ) ;
#14122 = VECTOR ( 'NONE', #2929, 1000.000000000000000 ) ;
#14123 = CARTESIAN_POINT ( 'NONE',  ( -7.999999999727738675, -29.19518467809294293, -26.31283570863942245 ) ) ;
#14124 = CARTESIAN_POINT ( 'NONE',  ( 10.70000000009999930, -30.05766787393000072, -27.53807693019799530 ) ) ;
#14125 = DIRECTION ( 'NONE',  ( 0.6941258031311203780, 0.7198537139083029945, 0.000000000000000000 ) ) ;
#14126 = EDGE_CURVE ( 'NONE', #23934, #29406, #22207, .T. ) ;
#14127 = ORIENTED_EDGE ( 'NONE', *, *, #9235, .F. ) ;
#14128 = DIRECTION ( 'NONE',  ( -0.000000000000000000, -0.000000000000000000, 1.000000000000000000 ) ) ;
#14129 = ADVANCED_FACE ( 'NONE', ( #26881 ), #9486, .T. ) ;
#14130 = EDGE_CURVE ( 'NONE', #6068, #11650, #12063, .T. ) ;
#14131 = CARTESIAN_POINT ( 'NONE',  ( -17.49999999932747130, -27.00000000000000000, -28.40000000020000215 ) ) ;
#14132 = ADVANCED_FACE ( 'NONE', ( #22314 ), #7374, .T. ) ;
#14133 = CARTESIAN_POINT ( 'NONE',  ( 0.8668428795360779704, 5.445660658769813089, -55.21500058692499380 ) ) ;
#14134 = VERTEX_POINT ( 'NONE', #10359 ) ;
#14135 = ITEM_DEFINED_TRANSFORMATION ( 'NONE', 'NONE', #25403,  #17722 ) ;
#14136 = B_SPLINE_CURVE_WITH_KNOTS ( 'NONE', 5,
 ( #9652, #14692, #19254, #7298, #24136, #14854, #18939, #16886, #24282 ),
 .UNSPECIFIED., .F., .F.,
 ( 6, 3, 6 ),
 ( 0.000000000000000000, 1.646696146280000050, 2.782752056640000138 ),
 .UNSPECIFIED. ) ;
#14137 = ORIENTED_EDGE ( 'NONE', *, *, #25816, .F. ) ;
#14138 = DIRECTION ( 'NONE',  ( 1.734723475976806503E-15, 1.000000000000000000, 0.000000000000000000 ) ) ;
#14139 = EDGE_LOOP ( 'NONE', ( #29744, #26469, #30757, #18416 ) ) ;
#14140 = CARTESIAN_POINT ( 'NONE',  ( -28.35945636591989683, -7.983396444576476902, 1.000000000000000888 ) ) ;
#14141 = CARTESIAN_POINT ( 'NONE',  ( -8.699999999668209583, -9.149979920083866958, -35.02638174926116221 ) ) ;
#14142 = CARTESIAN_POINT ( 'NONE',  ( -25.38146355688813216, 12.59839640969179975, 5.200000000000009948 ) ) ;
#14143 = CIRCLE ( 'NONE', #14665, 1.700000000000000178 ) ;
#14144 = CARTESIAN_POINT ( 'NONE',  ( -5.408100974049999898, -10.71225608600000001, 231.9999991140000191 ) ) ;
#14145 = CARTESIAN_POINT ( 'NONE',  ( -20.26572724632349320, -21.15151735177849091, 1.000000000000000888 ) ) ;
#14146 = DIRECTION ( 'NONE',  ( 2.764840495839172918E-12, 0.9128796883888953273, -0.4082287037029531107 ) ) ;
#14147 = CARTESIAN_POINT ( 'NONE',  ( 3.530284718056032833, 5.524446756132658898, -4.600967428500004175 ) ) ;
#14148 = CARTESIAN_POINT ( 'NONE',  ( 20.47082308819999952, -20.60185879389999997, 230.5592437530000041 ) ) ;
#14149 = ORIENTED_EDGE ( 'NONE', *, *, #17683, .F. ) ;
#14150 = CARTESIAN_POINT ( 'NONE',  ( -24.43799431780000120, -14.66523353630000059, 223.9971937000000253 ) ) ;
#14151 = CARTESIAN_POINT ( 'NONE',  ( 1.387648159808060999, -4.113210426322157609, -15.26414732020000464 ) ) ;
#14152 = CARTESIAN_POINT ( 'NONE',  ( 27.22264131787285990, 6.256663103294479278, 8.000000000000007105 ) ) ;
#14153 = CARTESIAN_POINT ( 'NONE',  ( 16.37473331892315542, -8.236461616552139375, 0.000000000000000000 ) ) ;
#14154 = FACE_BOUND ( 'NONE', #19967, .T. ) ;
#14155 = CARTESIAN_POINT ( 'NONE',  ( 16.37473331892315542, -8.236461616552139375, -0.6999999999999784173 ) ) ;
#14156 = CARTESIAN_POINT ( 'NONE',  ( -6.005838698572866008, -2.164963525412170853, -44.41497819512499490 ) ) ;
#14157 = CARTESIAN_POINT ( 'NONE',  ( 28.49528339128749366, 0.5184828350247226991, 1.000000000000000888 ) ) ;
#14158 = B_SPLINE_CURVE_WITH_KNOTS ( 'NONE', 3,
 ( #23598, #8945, #23444, #4541, #25798, #9096 ),
 .UNSPECIFIED., .F., .F.,
 ( 4, 2, 4 ),
 ( 0.000000000000000000, 0.5000000000000000000, 1.000000000000000000 ),
 .UNSPECIFIED. ) ;
#14159 = DIRECTION ( 'NONE',  ( -0.8775825618903718706, 0.4794255386042047262, 0.000000000000000000 ) ) ;
#14160 = CARTESIAN_POINT ( 'NONE',  ( -24.86822223968197321, -13.92223202027371975, 5.680679499000030219 ) ) ;
#14161 = CARTESIAN_POINT ( 'NONE',  ( 27.76135143710000008, -3.399672736040000081E-15, 187.6614141010000196 ) ) ;
#14162 = ORIENTED_EDGE ( 'NONE', *, *, #21912, .F. ) ;
#14163 = B_SPLINE_CURVE_WITH_KNOTS ( 'NONE', 5,
 ( #29743, #29433, #24878, #15569, #27684, #25027 ),
 .UNSPECIFIED., .F., .F.,
 ( 6, 6 ),
 ( 0.000000000000000000, 1.000000000000000000 ),
 .UNSPECIFIED. ) ;
#14164 = DIRECTION ( 'NONE',  ( 5.962915006522623408E-16, 0.4383711467890811231, 0.8987940462991652613 ) ) ;
#14165 = CARTESIAN_POINT ( 'NONE',  ( -15.73094807329767519, -9.126265404193597774, -0.6999999999999784173 ) ) ;
#14166 = CARTESIAN_POINT ( 'NONE',  ( 7.638687372290000610, 2.450513428906772706, -42.01217025054418741 ) ) ;
#14167 = AXIS2_PLACEMENT_3D ( 'NONE', #14530, #28682, #24270 ) ;
#14168 = ORIENTED_EDGE ( 'NONE', *, *, #16542, .T. ) ;
#14169 = VECTOR ( 'NONE', #28687, 1000.000000000000000 ) ;
#14170 = CARTESIAN_POINT ( 'NONE',  ( -2.577814338686791107, 4.205191132749348526, -45.80531229042500030 ) ) ;
#14171 = EDGE_LOOP ( 'NONE', ( #25190, #6926, #30218, #28392 ) ) ;
#14172 = VERTEX_POINT ( 'NONE', #19950 ) ;
#14173 = DIRECTION ( 'NONE',  ( 0.000000000000000000, 0.000000000000000000, 1.000000000000000000 ) ) ;
#14174 = ORIENTED_EDGE ( 'NONE', *, *, #12266, .F. ) ;
#14175 = CARTESIAN_POINT ( 'NONE',  ( -0.1058797546490000130, -28.50006311429999784, 223.9040511909999793 ) ) ;
#14176 = ORIENTED_EDGE ( 'NONE', *, *, #27627, .F. ) ;
#14177 = CARTESIAN_POINT ( 'NONE',  ( 9.000000000029999114, 21.00000000060000360, -70.09999999999999432 ) ) ;
#14178 = CARTESIAN_POINT ( 'NONE',  ( 23.80092420482279891, 14.36517094565843777, 3.899998581000013509 ) ) ;
#14179 = CARTESIAN_POINT ( 'NONE',  ( -24.41841039498785193, -14.69667350221323865, 3.899998581000013509 ) ) ;
#14180 = CARTESIAN_POINT ( 'NONE',  ( 1.112302519808859858, 4.726259607321323664, -35.70000000000000284 ) ) ;
#14181 = CARTESIAN_POINT ( 'NONE',  ( 8.700000000277558598, -14.62893623595633485, -33.38447208503446006 ) ) ;
#14182 = DIRECTION ( 'NONE',  ( 1.595945597898660305E-12, -0.7071067811865475727, -0.7071067811865475727 ) ) ;
#14183 = DIRECTION ( 'NONE',  ( 0.000000000000000000, 0.000000000000000000, 1.000000000000000000 ) ) ;
#14184 = AXIS2_PLACEMENT_3D ( 'NONE', #28728, #16310, #13959 ) ;
#14185 = CARTESIAN_POINT ( 'NONE',  ( -20.30397143369999924, 20.00000785070000120, 229.0000000000000000 ) ) ;
#14186 = EDGE_CURVE ( 'NONE', #25078, #4771, #25578, .T. ) ;
#14187 = ORIENTED_EDGE ( 'NONE', *, *, #2318, .F. ) ;
#14188 = CARTESIAN_POINT ( 'NONE',  ( -5.082228009654736312, -3.365126390422853220, -7.489929326000003940 ) ) ;
#14189 = CARTESIAN_POINT ( 'NONE',  ( 1.566980368899936193, 4.067530462867746444, -25.59462237480000724 ) ) ;
#14190 = CARTESIAN_POINT ( 'NONE',  ( 3.547887315624699056, -0.01749626818330200437, 0.000000000000000000 ) ) ;
#14191 = CARTESIAN_POINT ( 'NONE',  ( 23.73988791505310303, -12.43614577697740486, 225.1459679062442660 ) ) ;
#14192 = CARTESIAN_POINT ( 'NONE',  ( 24.97472003062369694, 13.73006752330286595, 5.208359080000030339 ) ) ;
#14193 = CARTESIAN_POINT ( 'NONE',  ( -25.33388805469397198, 13.05639290202442204, 5.735287127840217991 ) ) ;
#14194 = CARTESIAN_POINT ( 'NONE',  ( -2.322678811625143780, -3.635533071076384015, -21.70891267860000795 ) ) ;
#14195 = EDGE_CURVE ( 'NONE', #17360, #23934, #24210, .T. ) ;
#14196 = B_SPLINE_CURVE_WITH_KNOTS ( 'NONE', 3,
 ( #873, #10930, #17675, #10768, #3216, #8086, #3367, #15339, #12973, #29802, #20369, #13282 ),
 .UNSPECIFIED., .F., .F.,
 ( 4, 2, 2, 2, 2, 4 ),
 ( 0.000000000000000000, 0.2500000000000013878, 0.3750000000000012212, 0.5000000000000011102, 0.7500000000000005551, 1.000000000000000000 ),
 .UNSPECIFIED. ) ;
#14197 = CARTESIAN_POINT ( 'NONE',  ( 17.74448149004798481, 10.05302898057284899, -1.400000000000001688 ) ) ;
#14198 = CARTESIAN_POINT ( 'NONE',  ( 14.85000000009999788, -27.00000000000000000, -28.39999999989999679 ) ) ;
#14199 = CARTESIAN_POINT ( 'NONE',  ( -26.43116876448085861, -4.566970306898999965, -1.399999999999998579 ) ) ;
#14200 = VERTEX_POINT ( 'NONE', #5624 ) ;
#14201 = ORIENTED_EDGE ( 'NONE', *, *, #6352, .F. ) ;
#14202 = DIRECTION ( 'NONE',  ( 0.000000000000000000, 0.000000000000000000, -1.000000000000000000 ) ) ;
#14203 = DIRECTION ( 'NONE',  ( 0.8687154346624373913, 0.4953115116563036602, 0.000000000000000000 ) ) ;
#14204 = VERTEX_POINT ( 'NONE', #20111 ) ;
#14205 = CARTESIAN_POINT ( 'NONE',  ( -2.020725942109999895, 3.500000000090000007, 230.5235986622430175 ) ) ;
#14206 = CARTESIAN_POINT ( 'NONE',  ( 0.000000000000000000, 4.811145170119999648, -67.12721591429999535 ) ) ;
#14208 = ORIENTED_EDGE ( 'NONE', *, *, #4018, .F. ) ;
#14207 = AXIS2_PLACEMENT_3D ( 'NONE', #28703, #6677, #26350 ) ;
#14209 = EDGE_LOOP ( 'NONE', ( #21214, #12011, #13861, #8494 ) ) ;
#14210 = ORIENTED_EDGE ( 'NONE', *, *, #4098, .T. ) ;
#14211 = SURFACE_SIDE_STYLE ('',( #4604 ) ) ;
#14212 = ORIENTED_EDGE ( 'NONE', *, *, #24664, .T. ) ;
#14213 = CARTESIAN_POINT ( 'NONE',  ( 7.999999999977091214, -107.4273096626279482, 14.66297538114749344 ) ) ;
#14214 = EDGE_CURVE ( 'NONE', #19036, #18684, #433, .T. ) ;
#14215 = CARTESIAN_POINT ( 'NONE',  ( 18.00000000000000000, -4.408582873759999616E-15, 229.6412452697800006 ) ) ;
#14216 = CARTESIAN_POINT ( 'NONE',  ( 1.814857447021396585E-10, -51.11187400310945605, -27.80500476123474485 ) ) ;
#14217 = ORIENTED_EDGE ( 'NONE', *, *, #27010, .F. ) ;
#14218 = CARTESIAN_POINT ( 'NONE',  ( 26.80000000000000071, -7.020799968500000432, 230.0000000000000000 ) ) ;
#14219 = B_SPLINE_CURVE_WITH_KNOTS ( 'NONE', 5,
 ( #1835, #1996, #21339, #11585, #11734, #14261, #16142, #28418, #30634, #13947, #6853, #2307, #25913, #30939, #1678 ),
 .UNSPECIFIED., .F., .F.,
 ( 6, 3, 3, 3, 6 ),
 ( 0.000000000000000000, 6.476076814690000738, 12.95215362940000325, 19.42823044409999866, 25.90430725880000651 ),
 .UNSPECIFIED. ) ;
#14220 = CARTESIAN_POINT ( 'NONE',  ( 24.40301908004844833, -13.31707607419617112, 225.8857039579157799 ) ) ;
#14221 = CARTESIAN_POINT ( 'NONE',  ( 15.36964893400000065, -24.30838775939999863, 222.0000000000000000 ) ) ;
#14222 = CARTESIAN_POINT ( 'NONE',  ( 0.8260714174469999671, -28.48835664879999996, 225.7596297540000023 ) ) ;
#14223 = ORIENTED_EDGE ( 'NONE', *, *, #9967, .F. ) ;
#14224 = DIRECTION ( 'NONE',  ( -1.000000000000000000, 0.000000000000000000, 0.000000000000000000 ) ) ;
#14225 = CARTESIAN_POINT ( 'NONE',  ( 2.946576500976501478, 4.280162264036399655, -16.21259163649999735 ) ) ;
#14226 = PLANE ( 'NONE',  #18361 ) ;
#14227 = B_SPLINE_CURVE_WITH_KNOTS ( 'NONE', 3,
 ( #17761, #25491, #5817, #3931 ),
 .UNSPECIFIED., .F., .F.,
 ( 4, 4 ),
 ( 0.000000000000000000, 1.000000000000000000 ),
 .UNSPECIFIED. ) ;
#14228 = CARTESIAN_POINT ( 'NONE',  ( 0.4949169532526843107, -27.49533956265200629, 5.993098012594048285 ) ) ;
#14229 = ORIENTED_EDGE ( 'NONE', *, *, #17750, .F. ) ;
#14230 = CARTESIAN_POINT ( 'NONE',  ( -8.000000000050000892, -13.98526668056139144, -73.96855033896248699 ) ) ;
#14231 = CARTESIAN_POINT ( 'NONE',  ( 1.607747500013188446, -28.45491842328731025, 4.689797669000017599 ) ) ;
#14232 = LINE ( 'NONE', #12168, #27844 ) ;
#14233 = EDGE_CURVE ( 'NONE', #26031, #23194, #24978, .T. ) ;
#14234 = FACE_OUTER_BOUND ( 'NONE', #21310, .T. ) ;
#14235 = DIRECTION ( 'NONE',  ( -0.9316362575375349842, 0.3633921898465292122, -0.000000000000000000 ) ) ;
#14236 = DIRECTION ( 'NONE',  ( 1.000000000000000000, 0.000000000000000000, 0.000000000000000000 ) ) ;
#14237 = DIRECTION ( 'NONE',  ( -0.6941258031311203780, -0.7198537139083029945, 0.000000000000000000 ) ) ;
#14238 = ORIENTED_EDGE ( 'NONE', *, *, #29277, .F. ) ;
#14239 = B_SPLINE_CURVE_WITH_KNOTS ( 'NONE', 3,
 ( #11616, #21213, #8940, #18848, #28448, #23271, #6880, #16637, #9399, #3475, #16485, #10717, #26098, #4534, #11466, #13073, #2179, #20316 ),
 .UNSPECIFIED., .F., .F.,
 ( 4, 2, 2, 2, 2, 1, 1, 2, 2, 4 ),
 ( 0.000000000000000000, 0.1249999999999931166, 0.1874999999999897304, 0.2499999999999863443, 0.3749999999999832356, 0.4374999999999815148, 0.4687499999999824585, 0.4843749999999824030, 0.4999999999999824585, 1.000000000000000000 ),
 .UNSPECIFIED. ) ;
#14240 = CARTESIAN_POINT ( 'NONE',  ( -12.75378086759999796, -22.00000000000000000, -25.51324865357000249 ) ) ;
#14241 = CARTESIAN_POINT ( 'NONE',  ( -16.99800965038351919, -7.902812560281212484, -0.6999999999999783062 ) ) ;
#14242 = CARTESIAN_POINT ( 'NONE',  ( -26.79556473285982321, -0.4875557887250189237, 0.000000000000000000 ) ) ;
#14243 = DIRECTION ( 'NONE',  ( -0.8090169943751909232, 0.5877852522921378498, 0.000000000000000000 ) ) ;
#14244 = EDGE_CURVE ( 'NONE', #11498, #4187, #27643, .T. ) ;
#14245 = CIRCLE ( 'NONE', #7205, 1.000000000000000888 ) ;
#14246 = AXIS2_PLACEMENT_3D ( 'NONE', #9932, #26611, #2543 ) ;
#14247 = ADVANCED_FACE ( 'NONE', ( #8437, #15684, #22774 ), #1542, .T. ) ;
#14248 = CARTESIAN_POINT ( 'NONE',  ( 3.521042344302120153, 0.5632927345595589719, -88.52261276242234089 ) ) ;
#14249 = PRODUCT_DEFINITION_SHAPE ( 'NONE', 'NONE',  #31143 ) ;
#14250 = AXIS2_PLACEMENT_3D ( 'NONE', #17627, #5523, #521 ) ;
#14251 = VERTEX_POINT ( 'NONE', #5780 ) ;
#14252 = FACE_OUTER_BOUND ( 'NONE', #1907, .T. ) ;
#14253 = AXIS2_PLACEMENT_3D ( 'NONE', #953, #17457, #19978 ) ;
#14254 = B_SPLINE_CURVE_WITH_KNOTS ( 'NONE', 3,
 ( #29052, #4672, #439, #21984, #17092, #10021, #19616, #29198, #23888, #7645 ),
 .UNSPECIFIED., .F., .F.,
 ( 4, 2, 2, 2, 4 ),
 ( 0.000000000000000000, 0.2500000000000000000, 0.5000000000000000000, 0.7500000000000000000, 1.000000000000000000 ),
 .UNSPECIFIED. ) ;
#14255 = CARTESIAN_POINT ( 'NONE',  ( 1.605176535610508326, -27.75389821387976852, 4.999998581000003384 ) ) ;
#14256 = ORIENTED_EDGE ( 'NONE', *, *, #23476, .F. ) ;
#14257 = FACE_BOUND ( 'NONE', #23067, .T. ) ;
#14258 = EDGE_CURVE ( 'NONE', #10219, #18996, #12002, .T. ) ;
#14259 = CARTESIAN_POINT ( 'NONE',  ( -2.911316102860724175, -3.927725552502973727, -65.13409070562501313 ) ) ;
#14260 = ORIENTED_EDGE ( 'NONE', *, *, #11772, .F. ) ;
#14261 = CARTESIAN_POINT ( 'NONE',  ( -4.288653532660000600, 4.054393014030000408, 226.6412452697800006 ) ) ;
#14262 = CARTESIAN_POINT ( 'NONE',  ( 24.05832192679999793, -13.92979812329999945, 223.9000014189999774 ) ) ;
#14263 = CARTESIAN_POINT ( 'NONE',  ( 8.700000000296432390, -13.70519490899241788, -39.86245227785762779 ) ) ;
#14264 = ADVANCED_FACE ( 'NONE', ( #17723 ), #21061, .F. ) ;
#14265 = CARTESIAN_POINT ( 'NONE',  ( 12.51085694015827521, 20.99999999989886845, -69.72135916545833823 ) ) ;
#14266 = PLANE ( 'NONE',  #7975 ) ;
#14267 = ORIENTED_EDGE ( 'NONE', *, *, #12638, .F. ) ;
#14268 = CARTESIAN_POINT ( 'NONE',  ( 24.32472724076343695, -13.45989056521276872, 3.899998581000013509 ) ) ;
#14269 = CARTESIAN_POINT ( 'NONE',  ( -3.552713678799999608E-15, -3.552713678799999608E-15, 93.21714158839999698 ) ) ;
#14270 = AXIS2_PLACEMENT_3D ( 'NONE', #9902, #4872, #29091 ) ;
#14271 = AXIS2_PLACEMENT_3D ( 'NONE', #2049, #23765, #7070 ) ;
#14272 = DIRECTION ( 'NONE',  ( 0.000000000000000000, -1.000000000000000000, 0.000000000000000000 ) ) ;
#14273 = CARTESIAN_POINT ( 'NONE',  ( -25.27355175290000133, 12.75978488059999805, 224.8000000000000114 ) ) ;
#14274 = CARTESIAN_POINT ( 'NONE',  ( -12.38365826779466161, -30.50317931097972846, -32.15094117388489536 ) ) ;
#14275 = VECTOR ( 'NONE', #5598, 1000.000000000000114 ) ;
#14276 = LINE ( 'NONE', #23879, #25072 ) ;
#14277 = DIRECTION ( 'NONE',  ( 5.962915006522623408E-16, 0.4383711467890811231, 0.8987940462991652613 ) ) ;
#14278 = CARTESIAN_POINT ( 'NONE',  ( -25.44662322720032677, 12.83524168051548564, 4.689351480999998323 ) ) ;
#14279 = PLANE ( 'NONE',  #11605 ) ;
#14280 = EDGE_CURVE ( 'NONE', #9281, #29912, #13165, .T. ) ;
#14281 = B_SPLINE_SURFACE_WITH_KNOTS ( 'NONE', 5, 1, ( 
 ( #4828, #7339 ),
 ( #5287, #269 ),
 ( #16924, #12512 ),
 ( #29346, #581 ),
 ( #26993, #10162 ),
 ( #15042, #14425 ),
 ( #26532, #9850 ),
 ( #26681, #19606 ),
 ( #1183, #3223 ),
 ( #3373, #17842 ),
 ( #3853, #27763 ),
 ( #13443, #8558 ),
 ( #10322, #8242 ),
 ( #10475, #6207 ),
 ( #15184, #15344 ) ),
 .UNSPECIFIED., .F., .F., .F.,
 ( 6, 3, 3, 3, 6 ),
 ( 2, 2 ),
 ( 0.000000000000000000, 0.5238999881920000101, 1.047799976390000110, 1.571699964580000053, 1.746333293980000034 ),
 ( -0.7000000000009999335, 2.555864960449999711E-06 ),
 .UNSPECIFIED. ) ;
#14282 = CARTESIAN_POINT ( 'NONE',  ( 10.46457122910000059, 21.70000000000000284, -54.63542873130000288 ) ) ;
#14283 = CARTESIAN_POINT ( 'NONE',  ( -16.85343921422224156, -7.900182044607009679, 0.000000000000000000 ) ) ;
#14284 = CARTESIAN_POINT ( 'NONE',  ( 24.97472003062369694, 13.73006752330286595, 5.208359080000030339 ) ) ;
#14285 = ORIENTED_EDGE ( 'NONE', *, *, #2083, .T. ) ;
#14286 = DIRECTION ( 'NONE',  ( 1.000000000000000000, -1.843431230200084908E-12, 2.650498504963248473E-12 ) ) ;
#14287 = ORIENTED_EDGE ( 'NONE', *, *, #7317, .F. ) ;
#14288 = CARTESIAN_POINT ( 'NONE',  ( 8.000000000000000000, -17.05999687705277879, -77.21601615383784178 ) ) ;
#14289 = AXIS2_PLACEMENT_3D ( 'NONE', #30133, #1037, #13448 ) ;
#14290 = CARTESIAN_POINT ( 'NONE',  ( 4.569612387855602087, -0.08076758077263958280, -58.49793411332501591 ) ) ;
#14291 = EDGE_LOOP ( 'NONE', ( #28284, #1322, #5221, #7058 ) ) ;
#14292 = AXIS2_PLACEMENT_3D ( 'NONE', #3008, #24721, #514 ) ;
#14293 = AXIS2_PLACEMENT_3D ( 'NONE', #4435, #14039, #23792 ) ;
#14294 = CONTEXT_DEPENDENT_SHAPE_REPRESENTATION ( #1954, #19961 ) ;
#14295 = ORIENTED_EDGE ( 'NONE', *, *, #9589, .T. ) ;
#14296 = CARTESIAN_POINT ( 'NONE',  ( 8.700000000232341435, -25.77531388888509056, -25.66136093477824431 ) ) ;
#14297 = ORIENTED_EDGE ( 'NONE', *, *, #14976, .F. ) ;
#14298 = B_SPLINE_CURVE_WITH_KNOTS ( 'NONE', 5,
 ( #19278, #7322, #19432, #24306, #16907, #29023, #28869, #12349, #2140, #26058, #11729, #18964, #7011, #4644, #14255 ),
 .UNSPECIFIED., .F., .F.,
 ( 6, 3, 3, 3, 6 ),
 ( -1.746338520749999956, -1.571704668670000027, -1.047803112450000018, -0.5239015562239999202, 0.000000000000000000 ),
 .UNSPECIFIED. ) ;
#14299 = DIRECTION ( 'NONE',  ( 0.000000000000000000, 1.000000000000000000, 0.000000000000000000 ) ) ;
#14300 = CARTESIAN_POINT ( 'NONE',  ( -27.79539923781684507, -0.5057481689249112566, 1.000000000000000888 ) ) ;
#14301 = CARTESIAN_POINT ( 'NONE',  ( 3.490170497419999851, -11.55197646250000076, 231.9999991140000191 ) ) ;
#14302 = CARTESIAN_POINT ( 'NONE',  ( -10.69999999999999929, -120.5233595621999996, -31.26042064940000387 ) ) ;
#14303 = EDGE_CURVE ( 'NONE', #8486, #26548, #26581, .T. ) ;
#14304 = CARTESIAN_POINT ( 'NONE',  ( -30.50000000000000000, 2.720046410330000188E-15, 36.39444872449999480 ) ) ;
#14305 = CARTESIAN_POINT ( 'NONE',  ( -3.630162863991669209, -2.403661707492378508, -6.889929326000000742 ) ) ;
#14306 = PRESENTATION_LAYER_ASSIGNMENT (  '', '', ( #25351 ) ) ;
#14307 = CARTESIAN_POINT ( 'NONE',  ( 24.50094951250000008, -14.04160150939999951, 230.6999999999999886 ) ) ;
#14308 = ORIENTED_EDGE ( 'NONE', *, *, #2715, .T. ) ;
#14309 = CARTESIAN_POINT ( 'NONE',  ( -24.55841378230000061, -14.46270012129999927, 223.9201349020000009 ) ) ;
#14310 = CARTESIAN_POINT ( 'NONE',  ( -24.66442003930000126, -14.28072947929999970, 223.9000014189999774 ) ) ;
#14311 = ADVANCED_FACE ( 'NONE', ( #1224 ), #8761, .F. ) ;
#14312 = CARTESIAN_POINT ( 'NONE',  ( -4.448701673712585070, 0.6187532242676665462, -19.25159460730001371 ) ) ;
#14313 = LINE ( 'NONE', #7062, #30332 ) ;
#14314 = CARTESIAN_POINT ( 'NONE',  ( 24.60666973300000038, -12.93650480179999995, 225.0000014190000002 ) ) ;
#14315 = ADVANCED_FACE ( 'NONE', ( #1382 ), #10978, .T. ) ;
#14316 = B_SPLINE_CURVE_WITH_KNOTS ( 'NONE', 3,
 ( #13730, #10741, #22705, #25068, #25387, #11214, #6488, #25223, #10906, #1783, #20970, #20341 ),
 .UNSPECIFIED., .F., .F.,
 ( 4, 2, 2, 2, 2, 4 ),
 ( 0.000000000000000000, 0.2499999999999992784, 0.4999999999999985567, 0.6249999999999991118, 0.7499999999999995559, 1.000000000000000000 ),
 .UNSPECIFIED. ) ;
#14317 = B_SPLINE_CURVE_WITH_KNOTS ( 'NONE', 3,
 ( #30378, #4557, #23293, #11487, #28312, #30685 ),
 .UNSPECIFIED., .F., .F.,
 ( 4, 2, 4 ),
 ( 0.000000000000000000, 0.5000000000000000000, 1.000000000000000000 ),
 .UNSPECIFIED. ) ;
#14318 = DIRECTION ( 'NONE',  ( -1.000000000000000000, 0.000000000000000000, 0.000000000000000000 ) ) ;
#14319 = AXIS2_PLACEMENT_3D ( 'NONE', #3741, #10211, #27041 ) ;
#14320 = FACE_OUTER_BOUND ( 'NONE', #2215, .T. ) ;
#14321 = CARTESIAN_POINT ( 'NONE',  ( -18.22442895416311970, 20.00000017544967079, -0.6880553899999974909 ) ) ;
#14322 = VECTOR ( 'NONE', #18439, 1000.000000000000000 ) ;
#14323 = CARTESIAN_POINT ( 'NONE',  ( 8.700000000277906764, -15.94902145836247342, -35.53273252485295330 ) ) ;
#14324 = CARTESIAN_POINT ( 'NONE',  ( 8.000000000270995670, -18.23122067931581114, -34.51216076560703527 ) ) ;
#14325 = CARTESIAN_POINT ( 'NONE',  ( 17.16657240420000008, 10.97998838177520931, -1.972246272986471594 ) ) ;
#14326 = CARTESIAN_POINT ( 'NONE',  ( 8.999999999770000869, 20.19161784319999953, -43.40000000028999949 ) ) ;
#14327 = ORIENTED_EDGE ( 'NONE', *, *, #6199, .T. ) ;
#14328 = CARTESIAN_POINT ( 'NONE',  ( -10.00000000000656186, -14.12326208130076921, -36.34918993207352145 ) ) ;
#14329 = DIRECTION ( 'NONE',  ( 1.000000000000000000, -1.843431230208684274E-12, 2.650498504958264790E-12 ) ) ;
#14330 = CIRCLE ( 'NONE', #759, 3.750000000000000000 ) ;
#14331 = CARTESIAN_POINT ( 'NONE',  ( -7.999999999654833438, -13.70282216375966300, -36.63380720155397086 ) ) ;
#14332 = PRESENTATION_LAYER_ASSIGNMENT (  '', '', ( #25377 ) ) ;
#14333 = ORIENTED_EDGE ( 'NONE', *, *, #1225, .T. ) ;
#14334 = CYLINDRICAL_SURFACE ( 'NONE', #16771, 10.00000000000000355 ) ;
#14335 = CARTESIAN_POINT ( 'NONE',  ( -3.099154212379724882, 4.549648463301534385, -48.85391720692500428 ) ) ;
#14336 = ORIENTED_EDGE ( 'NONE', *, *, #17500, .T. ) ;
#14337 = ORIENTED_EDGE ( 'NONE', *, *, #7121, .F. ) ;
#14338 = DIRECTION ( 'NONE',  ( 0.000000000000000000, 0.000000000000000000, 1.000000000000000000 ) ) ;
#14339 = ORIENTED_EDGE ( 'NONE', *, *, #27638, .F. ) ;
#14340 = LINE ( 'NONE', #28486, #7940 ) ;
#14341 = VERTEX_POINT ( 'NONE', #8598 ) ;
#14342 = CARTESIAN_POINT ( 'NONE',  ( 24.15870318760000046, -15.11998207899999969, 225.5069924249999929 ) ) ;
#14343 = CARTESIAN_POINT ( 'NONE',  ( 3.072394438959999974, 1.678456730820000020, 227.6468472915199754 ) ) ;
#14344 = LINE ( 'NONE', #23943, #10454 ) ;
#14345 = CARTESIAN_POINT ( 'NONE',  ( 0.9773263286493246715, 4.731305334447203137, -35.69999999999999574 ) ) ;
#14346 = CARTESIAN_POINT ( 'NONE',  ( 8.700000000281731261, -13.73096375760723653, -34.33359398852594069 ) ) ;
#14347 = CARTESIAN_POINT ( 'NONE',  ( 9.499999999998065547, -18.19953924290990344, -36.00725302081955448 ) ) ;
#14348 = CARTESIAN_POINT ( 'NONE',  ( 17.16657240419154462, 10.99999999996915179, -0.6999999999999784173 ) ) ;
#14349 = CARTESIAN_POINT ( 'NONE',  ( 17.47393819615788502, -10.06595463928881884, -4.336808689942018722E-16 ) ) ;
#14350 = ORIENTED_EDGE ( 'NONE', *, *, #24288, .T. ) ;
#14351 = EDGE_CURVE ( 'NONE', #9711, #27663, #3958, .T. ) ;
#14352 = CARTESIAN_POINT ( 'NONE',  ( -4.338779899226326009, -4.343559731693466652, -9.813991631000003935 ) ) ;
#14353 = CARTESIAN_POINT ( 'NONE',  ( 5.307277461537168506, -2.951504967840870464, -26.93037294500000201 ) ) ;
#14354 = PLANE ( 'NONE',  #7258 ) ;
#14355 = EDGE_CURVE ( 'NONE', #9797, #25869, #7921, .T. ) ;
#14356 = AXIS2_PLACEMENT_3D ( 'NONE', #13237, #8511, #7103 ) ;
#14357 = STYLED_ITEM ( 'NONE', ( #16063 ), #4675 ) ;
#14358 = LINE ( 'NONE', #25847, #21232 ) ;
#14359 = CARTESIAN_POINT ( 'NONE',  ( 19.80526555972147307, 19.50877392102524155, 0.9999999989999952543 ) ) ;
#14360 = SURFACE_SIDE_STYLE ('',( #26763 ) ) ;
#14361 = CARTESIAN_POINT ( 'NONE',  ( -2.183849900456023896, 3.899926742306373928, -16.67761783620000315 ) ) ;
#14362 = CARTESIAN_POINT ( 'NONE',  ( 17.61443111645372639, 9.985034189246265512, -1.400000000000002132 ) ) ;
#14363 = CARTESIAN_POINT ( 'NONE',  ( 1.186786632855649781, -28.47586096820935353, 5.900907654000003610 ) ) ;
#14364 = DIRECTION ( 'NONE',  ( 1.000000000000000000, 0.000000000000000000, 0.000000000000000000 ) ) ;
#14365 = ORIENTED_EDGE ( 'NONE', *, *, #26192, .F. ) ;
#14366 = DIRECTION ( 'NONE',  ( -1.000000000000000000, 0.000000000000000000, 0.000000000000000000 ) ) ;
#14367 = CARTESIAN_POINT ( 'NONE',  ( 17.14656078599760392, 12.09981795542235439, -1.000005633855494125E-09 ) ) ;
#14368 = ORIENTED_EDGE ( 'NONE', *, *, #9513, .F. ) ;
#14369 = CARTESIAN_POINT ( 'NONE',  ( 25.00924755590000004, -13.66774365989999929, 225.9012973829999851 ) ) ;
#14370 = PLANE ( 'NONE',  #11277 ) ;
#14371 = ORIENTED_EDGE ( 'NONE', *, *, #21478, .F. ) ;
#14372 = ORIENTED_EDGE ( 'NONE', *, *, #14640, .F. ) ;
#14373 = ORIENTED_EDGE ( 'NONE', *, *, #18727, .T. ) ;
#14374 = PRESENTATION_STYLE_ASSIGNMENT (( #9483 ) ) ;
#14375 = ORIENTED_EDGE ( 'NONE', *, *, #12099, .T. ) ;
#14376 = CARTESIAN_POINT ( 'NONE',  ( -17.49999999969999820, -27.39748944249814855, -31.39993271324557256 ) ) ;
#14377 = CARTESIAN_POINT ( 'NONE',  ( 26.80000000069999899, -3.281945028320000125E-15, 230.0000000000000000 ) ) ;
#14378 = FACE_OUTER_BOUND ( 'NONE', #26286, .T. ) ;
#14379 = ADVANCED_FACE ( 'NONE', ( #15380 ), #30002, .F. ) ;
#14380 = VERTEX_POINT ( 'NONE', #8125 ) ;
#14381 = DIRECTION ( 'NONE',  ( -1.000000000000000000, 0.000000000000000000, 0.000000000000000000 ) ) ;
#14382 = CARTESIAN_POINT ( 'NONE',  ( 17.99591112602217891, 19.96082062028142090, 0.000000000000000000 ) ) ;
#14383 = CARTESIAN_POINT ( 'NONE',  ( 3.078268752310275858, -3.892570190047870415, -0.6999653576749226280 ) ) ;
#14384 = ORIENTED_EDGE ( 'NONE', *, *, #16439, .T. ) ;
#14385 = CARTESIAN_POINT ( 'NONE',  ( -19.42687617620407892, 20.00000591289990481, -0.3112909302383543575 ) ) ;
#14386 = CARTESIAN_POINT ( 'NONE',  ( 4.190083271568243894, -3.954132654168471817, -18.03565260999999964 ) ) ;
#14387 = B_SPLINE_CURVE_WITH_KNOTS ( 'NONE', 5,
 ( #30681, #6753, #9262, #9109, #25961, #14002, #2045, #11635, #21234, #18869, #23760, #24211, #14621, #21864, #9731 ),
 .UNSPECIFIED., .F., .F.,
 ( 6, 3, 3, 3, 6 ),
 ( 0.000000000000000000, 0.1000000000017179230, 0.4000000000011452173, 0.7000000000005726086, 1.000000000000000000 ),
 .UNSPECIFIED. ) ;
#14388 = CARTESIAN_POINT ( 'NONE',  ( -7.861312627756135818, -5.597492073231208565, -34.74908987276850780 ) ) ;
#14389 = CARTESIAN_POINT ( 'NONE',  ( 0.9877995823961871480, -27.48272658602460083, 5.490987494730114271 ) ) ;
#14390 = VERTEX_POINT ( 'NONE', #27805 ) ;
#14391 = DIRECTION ( 'NONE',  ( 0.000000000000000000, 0.000000000000000000, 1.000000000000000000 ) ) ;
#14392 = DIRECTION ( 'NONE',  ( 0.000000000000000000, 1.000000000000000000, 0.000000000000000000 ) ) ;
#14393 = CARTESIAN_POINT ( 'NONE',  ( -8.999999999699999975, 20.99999999990000887, -70.09999999999999432 ) ) ;
#14394 = CARTESIAN_POINT ( 'NONE',  ( 8.903108651239925564, -22.82508830966962421, 140.0000000000000000 ) ) ;
#14395 = CARTESIAN_POINT ( 'NONE',  ( -1.421085471519999843E-14, -1.421085471519999843E-14, 37.93968498539999956 ) ) ;
#14396 = CARTESIAN_POINT ( 'NONE',  ( 27.53132593009999951, -1.219023768970000058E-11, 229.7313259299999686 ) ) ;
#14397 = CARTESIAN_POINT ( 'NONE',  ( -13.39962415728801304, 21.69999999994393036, -68.94292916387466619 ) ) ;
#14398 = ORIENTED_EDGE ( 'NONE', *, *, #7964, .T. ) ;
#14399 = CARTESIAN_POINT ( 'NONE',  ( -10.69999999999999929, -24.00010364340000280, -28.42731455210000036 ) ) ;
#14400 = CARTESIAN_POINT ( 'NONE',  ( -17.13980697812163712, -7.934232311348328182, -0.6999999999999785283 ) ) ;
#14401 = CARTESIAN_POINT ( 'NONE',  ( -0.4042037169903076044, -5.063438148506004488, -68.10000000002501963 ) ) ;
#14402 = CARTESIAN_POINT ( 'NONE',  ( -7.813316244716991932, 4.375724744151460399, -39.61335272743919944 ) ) ;
#14403 = ORIENTED_EDGE ( 'NONE', *, *, #24459, .F. ) ;
#14404 = ADVANCED_FACE ( 'NONE', ( #22627 ), #8476, .T. ) ;
#14405 = CARTESIAN_POINT ( 'NONE',  ( 10.00000000000000000, -55.00000000000000000, -42.39999999999999858 ) ) ;
#14406 = SURFACE_STYLE_FILL_AREA ( #9522 ) ;
#14407 = ORIENTED_EDGE ( 'NONE', *, *, #9438, .F. ) ;
#14408 = CARTESIAN_POINT ( 'NONE',  ( 23.81776757408896472, 15.65134803726520296, 5.147520328545557078 ) ) ;
#14409 = CARTESIAN_POINT ( 'NONE',  ( 1.515105966933908421, -5.232275150211489922, -68.50367649352499200 ) ) ;
#14410 = EDGE_LOOP ( 'NONE', ( #5526, #24728, #21753, #13059 ) ) ;
#14411 = CARTESIAN_POINT ( 'NONE',  ( -1.611722395286938170, -6.291674585240492057, -28.14882611459999850 ) ) ;
#14412 = EDGE_CURVE ( 'NONE', #18576, #22920, #12506, .T. ) ;
#14413 = CARTESIAN_POINT ( 'NONE',  ( 1.030019577584204020E-10, -42.94729992905040206, -9.547410993456834305 ) ) ;
#14414 = CARTESIAN_POINT ( 'NONE',  ( 4.421972129926212247, 1.961202595004083005, -51.87998794302499306 ) ) ;
#14415 = CARTESIAN_POINT ( 'NONE',  ( -349323.8516741809435, 54523.81728493721312, -353320.2493477302487 ) ) ;
#14416 = CARTESIAN_POINT ( 'NONE',  ( -23.98258507372315051, -15.39789217239198571, 4.239862999000004962 ) ) ;
#14417 = DIRECTION ( 'NONE',  ( -0.9316362575375349842, 0.3633921898465292122, -0.000000000000000000 ) ) ;
#14418 = UNCERTAINTY_MEASURE_WITH_UNIT (LENGTH_MEASURE( 1.000000000000000082E-05 ), #17974, 'distance_accuracy_value', 'NONE');
#14419 = DIRECTION ( 'NONE',  ( -1.000000000000000000, -1.091125017015992317E-13, -6.718390282834052461E-12 ) ) ;
#14420 = CARTESIAN_POINT ( 'NONE',  ( -17.38918303935042431, -22.00020377080068812, -27.04753824768668835 ) ) ;
#14421 = VERTEX_POINT ( 'NONE', #23419 ) ;
#14422 = CARTESIAN_POINT ( 'NONE',  ( 1.100000000000000089, -17.25771824079999917, 5.000000000000000000 ) ) ;
#14423 = EDGE_CURVE ( 'NONE', #4792, #23036, #21096, .T. ) ;
#14424 = CARTESIAN_POINT ( 'NONE',  ( 3.540874049123775791, -2.351920722568056732, -35.09901165280005841 ) ) ;
#14425 = CARTESIAN_POINT ( 'NONE',  ( -23.35655559443967988, -15.07705663931308671, 5.680691770000024121 ) ) ;
#14426 = ADVANCED_FACE ( 'NONE', ( #6714 ), #29217, .F. ) ;
#14427 = CARTESIAN_POINT ( 'NONE',  ( -27.79999999990000248, 4.328052761030000362, 229.0000000000000000 ) ) ;
#14428 = LINE ( 'NONE', #9377, #26226 ) ;
#14429 = CARTESIAN_POINT ( 'NONE',  ( 3.150050076769718377, -21.47638757757964711, -30.34224088629133576 ) ) ;
#14430 = CARTESIAN_POINT ( 'NONE',  ( 8.999999999770000869, 20.26086086378412432, -44.12622114747841096 ) ) ;
#14431 = CARTESIAN_POINT ( 'NONE',  ( -24.35797963555383205, 13.39969403207715892, 3.901342130000013064 ) ) ;
#14432 = CARTESIAN_POINT ( 'NONE',  ( -10.69999999930000101, -27.00000000000000000, -31.39999999999999858 ) ) ;
#14433 = CIRCLE ( 'NONE', #28999, 4.276011752367102403 ) ;
#14434 = CARTESIAN_POINT ( 'NONE',  ( -6.000000000000000000, -17.49450075019272433, -75.24580708538225338 ) ) ;
#14435 = CARTESIAN_POINT ( 'NONE',  ( 4.175165894169885483, -50.49316738903675628, -63.39999999999999858 ) ) ;
#14436 = CARTESIAN_POINT ( 'NONE',  ( 24.98081130624543889, 13.71897605842228529, 4.999998581000003384 ) ) ;
#14437 = ADVANCED_BREP_SHAPE_REPRESENTATION ( '', ( #540, #17722 ), #14741 ) ;
#14438 = COLOUR_RGB ( '', 0.08235294, 0.09019608, 0.10196078) ;
#14439 = VERTEX_POINT ( 'NONE', #4666 ) ;
#14440 = FACE_OUTER_BOUND ( 'NONE', #8725, .T. ) ;
#14441 = ORIENTED_EDGE ( 'NONE', *, *, #2908, .T. ) ;
#14442 = B_SPLINE_CURVE_WITH_KNOTS ( 'NONE', 3,
 ( #19348, #16978, #26583, #13342, #24987, #19814, #17888, #27350, #17587, #1077, #3272, #10668, #10523, #27197, #15539, #17733, #20263, #13025, #3746, #24683, #5792, #29860, #3117, #22634 ),
 .UNSPECIFIED., .F., .F.,
 ( 4, 2, 2, 2, 2, 2, 2, 2, 2, 2, 2, 4 ),
 ( 6.505213034913026604E-19, 0.001577043753785921246, 0.002365565630678883279, 0.003154087507571844660, 0.004731131261357764822, 0.005519653138250724470, 0.006308175015143684117, 0.007885218768929599942, 0.009462262522715517502, 0.01025078439960847194, 0.01103930627650142639, 0.01261635003028733874 ),
 .UNSPECIFIED. ) ;
#14443 = CARTESIAN_POINT ( 'NONE',  ( 24.18127824746914811, -15.08370905573474374, 224.4394645126975547 ) ) ;
#14444 = EDGE_CURVE ( 'NONE', #3666, #23754, #14276, .T. ) ;
#14445 = CARTESIAN_POINT ( 'NONE',  ( 0.9634065801723908917, -5.189854773623245876, -59.49125695792500323 ) ) ;
#14446 = VERTEX_POINT ( 'NONE', #9546 ) ;
#14447 = EDGE_CURVE ( 'NONE', #23530, #25602, #19144, .T. ) ;
#14448 = EDGE_LOOP ( 'NONE', ( #24891, #13309, #23622, #3904 ) ) ;
#14449 = CARTESIAN_POINT ( 'NONE',  ( -27.63652367459999937, 8.874065151940001783, 229.0000000000000000 ) ) ;
#14450 = ORIENTED_EDGE ( 'NONE', *, *, #24083, .F. ) ;
#14451 = CARTESIAN_POINT ( 'NONE',  ( 1.850829058368556268, -2.615810859427025736, -36.20335296945545167 ) ) ;
#14452 = CARTESIAN_POINT ( 'NONE',  ( -10.46447140189999914, 20.99999999999999645, -54.63552859760000047 ) ) ;
#14453 = CARTESIAN_POINT ( 'NONE',  ( -27.87609112763790975, 3.928995115430390150, 3.799999999999998046 ) ) ;
#14454 = CIRCLE ( 'NONE', #19480, 27.23548387100000312 ) ;
#14455 = CIRCLE ( 'NONE', #27003, 4.000000004070001225 ) ;
#14456 = CARTESIAN_POINT ( 'NONE',  ( 16.71871369222880688, 12.01496581087208249, -1.400000000000002132 ) ) ;
#14457 = FACE_BOUND ( 'NONE', #3007, .T. ) ;
#14458 = DIRECTION ( 'NONE',  ( -1.000000000000000000, 5.063197467949062204E-16, -2.257212216284997029E-12 ) ) ;
#14459 = CARTESIAN_POINT ( 'NONE',  ( 5.763395275750641922, -2.111988417859953504, -5.236105321699997539 ) ) ;
#14460 = CARTESIAN_POINT ( 'NONE',  ( 28.50000000000000000, -3.552713678799999608E-15, 229.2404163060000144 ) ) ;
#14461 = ORIENTED_EDGE ( 'NONE', *, *, #4289, .F. ) ;
#14462 = LINE ( 'NONE', #2040, #17998 ) ;
#14463 = EDGE_CURVE ( 'NONE', #3949, #6922, #11292, .T. ) ;
#14464 = CARTESIAN_POINT ( 'NONE',  ( -2.879958020441473199, 3.829670441245457191, -20.56814294429999990 ) ) ;
#14465 = CARTESIAN_POINT ( 'NONE',  ( 26.79556473285982321, 0.4875557887249620803, 0.000000000000000000 ) ) ;
#14466 = CARTESIAN_POINT ( 'NONE',  ( -26.80000000000000071, 4.518892556970000030, 230.6999999999999886 ) ) ;
#14467 = ADVANCED_FACE ( 'NONE', ( #12061 ), #10012, .T. ) ;
#14468 = CARTESIAN_POINT ( 'NONE',  ( -4.198625225940000760, -11.29386252790000000, 230.6412452697800006 ) ) ;
#14469 = DIRECTION ( 'NONE',  ( -1.000000000000000000, 0.000000000000000000, 0.000000000000000000 ) ) ;
#14470 = PRODUCT_RELATED_PRODUCT_CATEGORY ( 'part', '', ( #18097 ) ) ;
#14471 = CARTESIAN_POINT ( 'NONE',  ( -6.005838698572866008, -2.164963525412170853, -43.93497819512499802 ) ) ;
#14472 = CARTESIAN_POINT ( 'NONE',  ( -10.69999999999999929, -125.6542114415999976, -32.94738679099999956 ) ) ;
#14473 = CARTESIAN_POINT ( 'NONE',  ( -16.06988921231594603, 11.79183908526949054, 0.000000000000000000 ) ) ;
#14474 = CARTESIAN_POINT ( 'NONE',  ( -24.66346748865669625, -14.28208995890502564, 6.002748559000014694 ) ) ;
#14475 = VECTOR ( 'NONE', #8818, 1000.000000000000000 ) ;
#14476 = CARTESIAN_POINT ( 'NONE',  ( 0.000000000000000000, 0.000000000000000000, 190.0000000000000000 ) ) ;
#14477 = ORIENTED_EDGE ( 'NONE', *, *, #30355, .T. ) ;
#14478 = CARTESIAN_POINT ( 'NONE',  ( 5.097421258188004067, 0.5103876169533114737, -30.56866556700000359 ) ) ;
#14479 = EDGE_CURVE ( 'NONE', #5034, #16422, #25943, .T. ) ;
#14480 = CARTESIAN_POINT ( 'NONE',  ( 0.000000000000000000, 0.000000000000000000, 115.0000000000000000 ) ) ;
#14481 = ORIENTED_EDGE ( 'NONE', *, *, #25585, .T. ) ;
#14482 = PLANE ( 'NONE',  #1195 ) ;
#14483 = CARTESIAN_POINT ( 'NONE',  ( 5.461196134307610528, -0.8102654170096962316, -46.93818262062499969 ) ) ;
#14484 = ORIENTED_EDGE ( 'NONE', *, *, #2406, .T. ) ;
#14485 = EDGE_LOOP ( 'NONE', ( #25669, #21486, #2598, #12929 ) ) ;
#14486 = EDGE_CURVE ( 'NONE', #4237, #15963, #13564, .T. ) ;
#14487 = DIRECTION ( 'NONE',  ( 0.000000000000000000, 0.000000000000000000, 1.000000000000000000 ) ) ;
#14488 = B_SPLINE_CURVE_WITH_KNOTS ( 'NONE', 3,
 ( #3662, #16665, #10, #28634, #14165, #21560 ),
 .UNSPECIFIED., .F., .F.,
 ( 4, 2, 4 ),
 ( 0.000000000000000000, 0.5000000000000000000, 1.000000000000000000 ),
 .UNSPECIFIED. ) ;
#14489 = VERTEX_POINT ( 'NONE', #24636 ) ;
#14490 = CARTESIAN_POINT ( 'NONE',  ( 8.700000000277906764, -15.94902145836247342, -35.53273252485295330 ) ) ;
#14491 = ORIENTED_EDGE ( 'NONE', *, *, #22912, .T. ) ;
#14492 = DIRECTION ( 'NONE',  ( 0.3633921898465292122, 0.9316362575375348731, -1.387778780781445360E-14 ) ) ;
#14493 = CARTESIAN_POINT ( 'NONE',  ( -9.993285220779425160, -25.61999708228226069, 115.0000000000000000 ) ) ;
#14494 = EDGE_CURVE ( 'NONE', #20670, #28644, #25208, .T. ) ;
#14495 = CARTESIAN_POINT ( 'NONE',  ( 21.28666574344908469, 18.00484885041732142, 1.000000000000000888 ) ) ;
#14496 = CARTESIAN_POINT ( 'NONE',  ( 0.8905567152654183527, 4.062885351561556391, -35.69999999999999574 ) ) ;
#14497 = CARTESIAN_POINT ( 'NONE',  ( -2.744417411265728912, -4.298957096598221561, -44.10000000002499121 ) ) ;
#14498 = CARTESIAN_POINT ( 'NONE',  ( -24.37821945910799926, 14.76389285725497125, 5.208432825000025801 ) ) ;
#14499 = CARTESIAN_POINT ( 'NONE',  ( 12.80098767942999771, -32.00000000058999916, -25.51324865428999900 ) ) ;
#14500 = DIRECTION ( 'NONE',  ( 0.000000000000000000, 0.000000000000000000, -1.000000000000000000 ) ) ;
#14501 = EDGE_LOOP ( 'NONE', ( #10941, #629, #23539, #17716 ) ) ;
#14502 = CARTESIAN_POINT ( 'NONE',  ( -4.484282906631563925, 1.269983465873031347, -7.810827254900003069 ) ) ;
#14503 = CARTESIAN_POINT ( 'NONE',  ( -4.781258647701263520, -0.007971864669480827059, -27.23106466010000304 ) ) ;
#14504 = CARTESIAN_POINT ( 'NONE',  ( 1.074123786107241241, -3.361570641823106165, 0.000000000000000000 ) ) ;
#14505 = B_SPLINE_CURVE_WITH_KNOTS ( 'NONE', 5,
 ( #13681, #1728, #8954, #28155, #25329, #11481, #21082, #9106, #18706 ),
 .UNSPECIFIED., .F., .F.,
 ( 6, 3, 6 ),
 ( 0.000000000000000000, 2.405120303519999947, 3.339306056889999930 ),
 .UNSPECIFIED. ) ;
#14506 = DIRECTION ( 'NONE',  ( 0.5000000000001898481, -0.8660254037843291286, 0.000000000000000000 ) ) ;
#14507 = CARTESIAN_POINT ( 'NONE',  ( 24.00926693399461342, 14.01467022386263395, 6.042472827000016977 ) ) ;
#14508 = CARTESIAN_POINT ( 'NONE',  ( -23.24663841807413434, -14.69162354064478215, 225.0964597109269221 ) ) ;
#14509 = DIRECTION ( 'NONE',  ( -1.000000000000000000, 0.000000000000000000, 0.000000000000000000 ) ) ;
#14510 = CARTESIAN_POINT ( 'NONE',  ( 1.265035515811502309, -4.453021097817297047, -21.29535708919999593 ) ) ;
#14511 = DIRECTION ( 'NONE',  ( 1.000000000000000000, 0.000000000000000000, 0.000000000000000000 ) ) ;
#14512 = CARTESIAN_POINT ( 'NONE',  ( 4.638687372203637693, -13.76085703354776335, -30.76755074926543898 ) ) ;
#14513 = CARTESIAN_POINT ( 'NONE',  ( -12.47330046629999956, 20.99999999999999645, -55.90292611659999977 ) ) ;
#14514 = ORIENTED_EDGE ( 'NONE', *, *, #21227, .F. ) ;
#14515 = VECTOR ( 'NONE', #8011, 1000.000000000000000 ) ;
#14516 = FACE_OUTER_BOUND ( 'NONE', #23773, .T. ) ;
#14517 = CARTESIAN_POINT ( 'NONE',  ( -12.67459614424497794, -32.00000000000000711, -31.01244741568594776 ) ) ;
#14518 = ORIENTED_EDGE ( 'NONE', *, *, #15191, .T. ) ;
#14519 = CARTESIAN_POINT ( 'NONE',  ( 26.80000000069999899, -3.281945028320000125E-15, 136.7828584130000138 ) ) ;
#14520 = CARTESIAN_POINT ( 'NONE',  ( 21.81274943930000276, 17.27884304029999640, 223.9999999570000000 ) ) ;
#14521 = EDGE_CURVE ( 'NONE', #145, #15176, #6427, .T. ) ;
#14522 = ORIENTED_EDGE ( 'NONE', *, *, #24701, .T. ) ;
#14523 = ORIENTED_EDGE ( 'NONE', *, *, #6006, .F. ) ;
#14524 = ORIENTED_EDGE ( 'NONE', *, *, #17758, .T. ) ;
#14525 = EDGE_LOOP ( 'NONE', ( #8689, #27169, #11181, #3797, #12986, #23033, #19234, #15400 ) ) ;
#14526 = DIRECTION ( 'NONE',  ( -2.966217977826874882E-25, -1.000000000000000000, 2.257145581549900232E-12 ) ) ;
#14527 = EDGE_CURVE ( 'NONE', #8329, #29142, #30465, .T. ) ;
#14528 = VECTOR ( 'NONE', #26114, 1000.000000000000114 ) ;
#14529 = ADVANCED_FACE ( 'NONE', ( #19299 ), #15513, .T. ) ;
#14530 = CARTESIAN_POINT ( 'NONE',  ( -3.552713678799999608E-15, -3.552713678799999608E-15, 93.21714158839999698 ) ) ;
#14531 = CARTESIAN_POINT ( 'NONE',  ( -24.98081131316241255, -13.71897606304888662, 4.999998581000003384 ) ) ;
#14532 = ORIENTED_EDGE ( 'NONE', *, *, #23823, .F. ) ;
#14533 = LINE ( 'NONE', #21457, #9911 ) ;
#14534 = CARTESIAN_POINT ( 'NONE',  ( -10.00000000000000000, -13.64324653723545921, -74.90824295974830704 ) ) ;
#14535 = CARTESIAN_POINT ( 'NONE',  ( -17.40556230546876648, -31.99979043241261323, -27.16013815127665154 ) ) ;
#14536 = CARTESIAN_POINT ( 'NONE',  ( 8.000000000000000000, -17.74403716370463968, -75.33663091226621589 ) ) ;
#14537 = CARTESIAN_POINT ( 'NONE',  ( 3.543796088487663809, -3.315250500659660648, -0.6997944144658480026 ) ) ;
#14538 = ORIENTED_EDGE ( 'NONE', *, *, #13884, .F. ) ;
#14539 = DIRECTION ( 'NONE',  ( -0.000000000000000000, 1.000000000000000000, -2.258510841069999963E-12 ) ) ;
#14540 = VECTOR ( 'NONE', #9539, 1000.000000000000114 ) ;
#14541 = B_SPLINE_SURFACE_WITH_KNOTS ( 'NONE', 5, 1, ( 
 ( #6243, #12694 ),
 ( #10811, #22929 ),
 ( #20560, #8117 ),
 ( #5614, #6077 ),
 ( #29991, #15674 ),
 ( #12859, #22461 ),
 ( #30155, #15846 ),
 ( #3404, #22306 ),
 ( #24820, #25450 ) ),
 .UNSPECIFIED., .F., .F., .F.,
 ( 6, 3, 6 ),
 ( 2, 2 ),
 ( 0.000000000000000000, 12.04044600379999963, 17.39568165169999858 ),
 ( -4.097259680450000872E-15, 0.7017616274569999923 ),
 .UNSPECIFIED. ) ;
#14542 = CARTESIAN_POINT ( 'NONE',  ( 2.326244606069574505, 3.379075471592551949, -17.21259163650000446 ) ) ;
#14543 = CARTESIAN_POINT ( 'NONE',  ( -7.746287188306563820, -6.291484674763839102, -34.41060706477745157 ) ) ;
#14544 = DIRECTION ( 'NONE',  ( 0.000000000000000000, 0.000000000000000000, 1.000000000000000000 ) ) ;
#14545 = LINE ( 'NONE', #29154, #6148 ) ;
#14546 = CARTESIAN_POINT ( 'NONE',  ( 17.95841148948556310, 10.23646161652002817, -0.6999999999999784173 ) ) ;
#14547 = CARTESIAN_POINT ( 'NONE',  ( 22.64694720651011650, -14.33102249085027680, 5.218051573047087111 ) ) ;
#14548 = CIRCLE ( 'NONE', #12046, 3.199999999250000560 ) ;
#14549 = LINE ( 'NONE', #22092, #11465 ) ;
#14550 = CARTESIAN_POINT ( 'NONE',  ( 10.00000000000000000, 21.69999999990000106, -70.10000000019999788 ) ) ;
#14551 = CARTESIAN_POINT ( 'NONE',  ( 26.80907646719999704, 9.389153233529999198, 229.1414213529999984 ) ) ;
#14552 = CARTESIAN_POINT ( 'NONE',  ( -18.02779420929999787, -3.032264855710000262, 230.6999999999999886 ) ) ;
#14553 = ORIENTED_EDGE ( 'NONE', *, *, #24892, .F. ) ;
#14554 = AXIS2_PLACEMENT_3D ( 'NONE', #4782, #30903, #9805 ) ;
#14555 = EDGE_CURVE ( 'NONE', #3795, #7075, #26536, .T. ) ;
#14556 = CARTESIAN_POINT ( 'NONE',  ( -12.47178235754251219, -22.95684202855160194, -24.96081565149350823 ) ) ;
#14557 = EDGE_CURVE ( 'NONE', #16714, #25254, #11012, .T. ) ;
#14558 = B_SPLINE_CURVE_WITH_KNOTS ( 'NONE', 4,
 ( #945, #29254, #17299, #26907, #17601 ),
 .UNSPECIFIED., .F., .F.,
 ( 5, 5 ),
 ( -0.9817477042459999970, 0.9817477042459999970 ),
 .UNSPECIFIED. ) ;
#14559 = CARTESIAN_POINT ( 'NONE',  ( 2.184925289844788399, -4.318546512737748699, -68.10000000002500542 ) ) ;
#14560 = CARTESIAN_POINT ( 'NONE',  ( -4.894918280844120950, -0.4876114613646642115, -68.10000000002500542 ) ) ;
#14561 = ORIENTED_EDGE ( 'NONE', *, *, #29436, .T. ) ;
#14562 = CARTESIAN_POINT ( 'NONE',  ( 26.80000000069999899, 2.537275649180000148, 230.6999999999999886 ) ) ;
#14563 = ORIENTED_EDGE ( 'NONE', *, *, #8473, .T. ) ;
#14565 = CARTESIAN_POINT ( 'NONE',  ( -3.552713678799999608E-15, 0.000000000000000000, 143.2171415880000040 ) ) ;
#14564 = B_SPLINE_CURVE_WITH_KNOTS ( 'NONE', 3,
 ( #17920, #22519, #10250, #27229, #27530, #8483 ),
 .UNSPECIFIED., .F., .F.,
 ( 4, 2, 4 ),
 ( 0.000000000000000000, 0.5000000000000000000, 1.000000000000000000 ),
 .UNSPECIFIED. ) ;
#14566 = CARTESIAN_POINT ( 'NONE',  ( 1.353924481083393028, -4.675650134241364775, -68.45367649352499484 ) ) ;
#14567 = ORIENTED_EDGE ( 'NONE', *, *, #10296, .T. ) ;
#14568 = CARTESIAN_POINT ( 'NONE',  ( -4.555585884337687297, -4.059738318096004939, -24.84101932450000305 ) ) ;
#14569 = DIRECTION ( 'NONE',  ( -1.224606353819999829E-16, -1.000000000000000000, 0.000000000000000000 ) ) ;
#14570 = AXIS2_PLACEMENT_3D ( 'NONE', #27787, #6854, #23088 ) ;
#14571 = VECTOR ( 'NONE', #1289, 1000.000000000000000 ) ;
#14572 = B_SPLINE_SURFACE_WITH_KNOTS ( 'NONE', 5, 1, ( 
 ( #24481, #7938 ),
 ( #12511, #9849 ),
 ( #19448, #7787 ),
 ( #17539, #17389 ),
 ( #15183, #24787 ),
 ( #3220, #12831 ),
 ( #22433, #29039 ),
 ( #23059, #25422 ),
 ( #20215, #8557 ),
 ( #15811, #17841 ),
 ( #11094, #15645 ),
 ( #5887, #25098 ),
 ( #23212, #5738 ),
 ( #24941, #20071 ),
 ( #12977, #3372 ) ),
 .UNSPECIFIED., .F., .F., .F.,
 ( 6, 3, 3, 3, 6 ),
 ( 2, 2 ),
 ( 0.000000000000000000, 0.5239010160280000994, 1.047802032050000109, 1.571703048080000054, 1.746336720089999961 ),
 ( -0.7000000000009999335, 2.556023394720000151E-06 ),
 .UNSPECIFIED. ) ;
#14573 = CARTESIAN_POINT ( 'NONE',  ( 4.003591150705129387, -2.204345408526039218, -58.30843849682500490 ) ) ;
#14574 = CARTESIAN_POINT ( 'NONE',  ( 6.438687372205746051, -7.245008774204572788, -33.94554228705224830 ) ) ;
#14575 = FACE_OUTER_BOUND ( 'NONE', #23245, .T. ) ;
#14576 = CARTESIAN_POINT ( 'NONE',  ( -10.70000000000015206, -26.27037943353427707, -25.46729144951078183 ) ) ;
#14577 = DIRECTION ( 'NONE',  ( 0.000000000000000000, 0.000000000000000000, 1.000000000000000000 ) ) ;
#14578 = CARTESIAN_POINT ( 'NONE',  ( 8.700000000295537106, -10.55542841719123537, -37.33290089570849801 ) ) ;
#14579 = FACE_OUTER_BOUND ( 'NONE', #29782, .T. ) ;
#14580 = ORIENTED_EDGE ( 'NONE', *, *, #22334, .F. ) ;
#14581 = CARTESIAN_POINT ( 'NONE',  ( 22.41261198964086176, 16.47772013495439225, 7.000000000000006217 ) ) ;
#14582 = EDGE_CURVE ( 'NONE', #10785, #19471, #1168, .T. ) ;
#14583 = CYLINDRICAL_SURFACE ( 'NONE', #18797, 3.000000000000001776 ) ;
#14584 = CARTESIAN_POINT ( 'NONE',  ( -4.775507269660000276, 11.08259804160000073, 231.9999989789999972 ) ) ;
#14585 = CARTESIAN_POINT ( 'NONE',  ( -19.80526803549999926, 19.50877411520000138, 226.2000000000000171 ) ) ;
#14586 = CARTESIAN_POINT ( 'NONE',  ( -8.699999999724179034, -29.73863906514459643, -27.17531388891805477 ) ) ;
#14587 = CARTESIAN_POINT ( 'NONE',  ( 1.638687372170417822, -21.81692582114680334, -30.17614928725064161 ) ) ;
#14588 = CARTESIAN_POINT ( 'NONE',  ( 24.59318164545437924, -12.96225840978618571, 224.7106956858033584 ) ) ;
#14589 = CARTESIAN_POINT ( 'NONE',  ( 8.000000000229924524, -28.07052495763006661, -25.59750966822355522 ) ) ;
#14590 = CARTESIAN_POINT ( 'NONE',  ( -0.8178280288081285487, -26.78758467685877775, 225.7372270131871517 ) ) ;
#14591 = CARTESIAN_POINT ( 'NONE',  ( -24.83827471527357744, 12.48687850854618198, 4.895780543000022078 ) ) ;
#14592 = FACE_OUTER_BOUND ( 'NONE', #9601, .T. ) ;
#14593 = EDGE_CURVE ( 'NONE', #6349, #6970, #36, .T. ) ;
#14594 = CARTESIAN_POINT ( 'NONE',  ( 11.76275999642616199, 2.846903786951354931, 232.0000002394077399 ) ) ;
#14595 = PLANE ( 'NONE',  #22865 ) ;
#14596 = CARTESIAN_POINT ( 'NONE',  ( 18.13627779908860305, 10.46175468807264863, -0.6999999999999785283 ) ) ;
#14597 = EDGE_LOOP ( 'NONE', ( #21225, #3013, #23156, #8897 ) ) ;
#14598 = CARTESIAN_POINT ( 'NONE',  ( 19.80526555972147307, 19.50877392102524155, 1.400000000000012346 ) ) ;
#14599 = SURFACE_SIDE_STYLE ('',( #21095 ) ) ;
#14600 = ORIENTED_EDGE ( 'NONE', *, *, #3677, .F. ) ;
#14601 = CYLINDRICAL_SURFACE ( 'NONE', #12440, 4.276011752367109509 ) ;
#14602 = CARTESIAN_POINT ( 'NONE',  ( -5.623491485972666126, 3.092612689740418919, -59.81908057272499946 ) ) ;
#14603 = ORIENTED_EDGE ( 'NONE', *, *, #12881, .F. ) ;
#14604 = VERTEX_POINT ( 'NONE', #5743 ) ;
#14605 = CARTESIAN_POINT ( 'NONE',  ( 7.453090060300407771, -2.907137518772282991, 27.99999999999999645 ) ) ;
#14606 = ORIENTED_EDGE ( 'NONE', *, *, #15024, .F. ) ;
#14607 = EDGE_CURVE ( 'NONE', #3906, #10703, #15037, .T. ) ;
#14608 = ORIENTED_EDGE ( 'NONE', *, *, #27578, .F. ) ;
#14609 = FACE_OUTER_BOUND ( 'NONE', #10561, .T. ) ;
#14610 = CARTESIAN_POINT ( 'NONE',  ( 9.707106781189999367, 19.99999999999999645, -43.10710678118599759 ) ) ;
#14611 = CYLINDRICAL_SURFACE ( 'NONE', #16826, 2.100000000000000977 ) ;
#14612 = CARTESIAN_POINT ( 'NONE',  ( -9.993285220779547728, -25.61999708228220030, 43.60555127550000520 ) ) ;
#14613 = CARTESIAN_POINT ( 'NONE',  ( -4.273751495587445604, 4.364932658710685587, -4.568732180600005854 ) ) ;
#14614 = CYLINDRICAL_SURFACE ( 'NONE', #15487, 4.439999999999999503 ) ;
#14615 = ORIENTED_EDGE ( 'NONE', *, *, #15641, .T. ) ;
#14616 = CARTESIAN_POINT ( 'NONE',  ( -0.07854999671243234616, -5.046990879750716807, -44.10000000002500542 ) ) ;
#14617 = CARTESIAN_POINT ( 'NONE',  ( 24.86822223037987456, 13.92223202030449691, 4.319317656000021266 ) ) ;
#14618 = CARTESIAN_POINT ( 'NONE',  ( -3.664565019602479268, -2.682238183793479447, -19.81004627010000618 ) ) ;
#14619 = DIRECTION ( 'NONE',  ( 0.000000000000000000, 0.3420201433259318358, -0.9396926207858125046 ) ) ;
#14620 = DIRECTION ( 'NONE',  ( 0.3633921898465289901, 0.9316362575375348731, -2.168404344971007290E-15 ) ) ;
#14621 = CARTESIAN_POINT ( 'NONE',  ( -24.60124998910000116, -12.94761260449999973, 224.7915656799999908 ) ) ;
#14622 = DIRECTION ( 'NONE',  ( 0.000000000000000000, 0.000000000000000000, -1.000000000000000000 ) ) ;
#14623 = CARTESIAN_POINT ( 'NONE',  ( 2.295476649252891743, -3.592865671589301257, -43.16966640442500847 ) ) ;
#14624 = EDGE_CURVE ( 'NONE', #22582, #23024, #15016, .T. ) ;
#14625 = CARTESIAN_POINT ( 'NONE',  ( 4.038813138129719427, -20.77648683177044475, -30.68360528878402960 ) ) ;
#14626 = CARTESIAN_POINT ( 'NONE',  ( -15.73622915490642526, 11.16397745117368245, -4.336808689942018722E-16 ) ) ;
#14627 = CARTESIAN_POINT ( 'NONE',  ( -3.982632971385690279, -21.02717377734789039, -30.56133709589786207 ) ) ;
#14628 = CARTESIAN_POINT ( 'NONE',  ( -17.93345241809999990, 20.10553870999999759, 230.0000000000000000 ) ) ;
#14629 = B_SPLINE_CURVE_WITH_KNOTS ( 'NONE', 3,
 ( #8862, #13596, #13909, #30117, #1643, #25721, #8546, #11233, #23364, #30742, #27748, #20837 ),
 .UNSPECIFIED., .F., .F.,
 ( 4, 2, 2, 2, 2, 4 ),
 ( 0.000000000000000000, 0.2499999999999830136, 0.3749999999999746314, 0.4999999999999662492, 0.7499999999999830136, 1.000000000000000000 ),
 .UNSPECIFIED. ) ;
#14630 = DIRECTION ( 'NONE',  ( -1.000000000000000000, 0.000000000000000000, 0.000000000000000000 ) ) ;
#14631 = ORIENTED_EDGE ( 'NONE', *, *, #2021, .T. ) ;
#14632 = CARTESIAN_POINT ( 'NONE',  ( 6.487627055914963137, 0.6495842397260740420, -29.63116556699998938 ) ) ;
#14633 = DIRECTION ( 'NONE',  ( 0.000000000000000000, 0.000000000000000000, 1.000000000000000000 ) ) ;
#14634 = ORIENTED_EDGE ( 'NONE', *, *, #26690, .F. ) ;
#14635 = EDGE_CURVE ( 'NONE', #24995, #61, #9510, .T. ) ;
#14636 = CARTESIAN_POINT ( 'NONE',  ( 7.797918471980000099, -130.0000000000000000, -43.60208152801600079 ) ) ;
#14637 = CARTESIAN_POINT ( 'NONE',  ( 4.315256771988541296, 1.538274589489400990, -46.32627377572500649 ) ) ;
#14638 = ORIENTED_EDGE ( 'NONE', *, *, #2925, .T. ) ;
#14639 = ORIENTED_EDGE ( 'NONE', *, *, #23286, .F. ) ;
#14640 = EDGE_CURVE ( 'NONE', #10748, #1470, #20074, .T. ) ;
#14641 = DIRECTION ( 'NONE',  ( 1.000000000000000000, 0.000000000000000000, 0.000000000000000000 ) ) ;
#14642 = CONICAL_SURFACE ( 'NONE', #3546, 3.491271820449999286, 1.047197551199999799 ) ;
#14643 = VERTEX_POINT ( 'NONE', #13130 ) ;
#14644 = CARTESIAN_POINT ( 'NONE',  ( -7.999999999730130540, -27.01023037466701737, -25.37764016532643652 ) ) ;
#14645 = VERTEX_POINT ( 'NONE', #1185 ) ;
#14646 = CYLINDRICAL_SURFACE ( 'NONE', #6516, 1.100000000000002309 ) ;
#14647 = LINE ( 'NONE', #14951, #4225 ) ;
#14648 = CARTESIAN_POINT ( 'NONE',  ( 8.999999999770000869, 20.70710678120000381, -44.39289321881399530 ) ) ;
#14649 = CARTESIAN_POINT ( 'NONE',  ( 0.3116452112896634929, 4.617848473969027090, -35.69999999999999574 ) ) ;
#14650 = EDGE_CURVE ( 'NONE', #13665, #28711, #17999, .T. ) ;
#14651 = CARTESIAN_POINT ( 'NONE',  ( 18.52668879010899516, 20.00003523974170605, -0.6360013681344631742 ) ) ;
#14652 = CARTESIAN_POINT ( 'NONE',  ( -24.37165444408190851, 14.77472139917419369, 5.104215870000011535 ) ) ;
#14653 = CARTESIAN_POINT ( 'NONE',  ( -22.71671780387977790, -14.21943167064913105, 5.548968161578956781 ) ) ;
#14654 = CARTESIAN_POINT ( 'NONE',  ( 13.00000000000000000, 23.81663212713006672, -62.33813991915980779 ) ) ;
#14655 = CARTESIAN_POINT ( 'NONE',  ( -2.564224011386423641, 5.541743391105337757, -8.331725184300003306 ) ) ;
#14656 = CARTESIAN_POINT ( 'NONE',  ( -5.430430790592723156, -2.746024268427175841, -27.96472909260000606 ) ) ;
#14657 = CARTESIAN_POINT ( 'NONE',  ( -2.664535259099999568E-14, -26.80000000000000071, 20.00000000000000355 ) ) ;
#14658 = ADVANCED_FACE ( 'NONE', ( #10781 ), #6209, .T. ) ;
#14659 = CARTESIAN_POINT ( 'NONE',  ( -8.000000000000000000, -15.86465192213301556, -74.65259062561435144 ) ) ;
#14660 = DIRECTION ( 'NONE',  ( -1.075528555106586974E-13, -0.9622309798138365400, -0.2722343503059523884 ) ) ;
#14661 = CARTESIAN_POINT ( 'NONE',  ( -23.24663841809999809, -14.69162354060000020, 225.0000000000000000 ) ) ;
#14662 = CARTESIAN_POINT ( 'NONE',  ( 2.639254916689341979, -27.37824394259287786, 20.00000000000000711 ) ) ;
#14663 = CARTESIAN_POINT ( 'NONE',  ( -2.227024806490486508, -3.476280271252723431, -18.70544088819999118 ) ) ;
#14664 = B_SPLINE_SURFACE_WITH_KNOTS ( 'NONE', 5, 1, ( 
 ( #27604, #17992 ),
 ( #25255, #12976 ),
 ( #15810, #10933 ),
 ( #1030, #13125 ),
 ( #29805, #17840 ),
 ( #16119, #6205 ),
 ( #30285, #3687 ),
 ( #22734, #27445 ),
 ( #13286, #8716 ),
 ( #20373, #22897 ),
 ( #6521, #25097 ),
 ( #4008, #15493 ),
 ( #1339, #8556 ),
 ( #13441, #18156 ),
 ( #3851, #23057 ) ),
 .UNSPECIFIED., .F., .F., .F.,
 ( 6, 3, 3, 3, 6 ),
 ( 2, 2 ),
 ( 0.000000000000000000, 0.5239010160280000994, 1.047802032050000109, 1.571703048080000054, 1.746336720089999961 ),
 ( -0.7000000000009999335, 2.556023926959999973E-06 ),
 .UNSPECIFIED. ) ;
#14665 = AXIS2_PLACEMENT_3D ( 'NONE', #4244, #6442, #13844 ) ;
#14666 = CARTESIAN_POINT ( 'NONE',  ( -10.69999999999999929, -29.12132034360000077, -30.52132034359999935 ) ) ;
#14667 = CARTESIAN_POINT ( 'NONE',  ( 14.84469677950085398, -24.79650568944878941, -23.89868534099636577 ) ) ;
#14668 = DIRECTION ( 'NONE',  ( 1.000000000000000000, 0.000000000000000000, 0.000000000000000000 ) ) ;
#14669 = ORIENTED_EDGE ( 'NONE', *, *, #19991, .T. ) ;
#14670 = ADVANCED_FACE ( 'NONE', ( #17996 ), #23084, .T. ) ;
#14671 = CARTESIAN_POINT ( 'NONE',  ( 28.50000000000000000, -3.490128108379999702E-15, 90.00000000000000000 ) ) ;
#14672 = CARTESIAN_POINT ( 'NONE',  ( -12.38084235052808246, -32.00000000000000000, -27.25842518461809760 ) ) ;
#14673 = VERTEX_POINT ( 'NONE', #1343 ) ;
#14674 = DIRECTION ( 'NONE',  ( -2.764840495839172918E-12, -0.9128796883888953273, 0.4082287037029530552 ) ) ;
#14675 = CARTESIAN_POINT ( 'NONE',  ( -16.52704821190178208, 9.934232311991996411, -0.6999999999999785283 ) ) ;
#14676 = ORIENTED_EDGE ( 'NONE', *, *, #24737, .T. ) ;
#14677 = CARTESIAN_POINT ( 'NONE',  ( 4.595672992649999955, 11.13819882230000147, 230.6412452697800006 ) ) ;
#14678 = ORIENTED_EDGE ( 'NONE', *, *, #6579, .F. ) ;
#14679 = EDGE_LOOP ( 'NONE', ( #25543, #11933, #5866, #30912 ) ) ;
#14680 = ORIENTED_EDGE ( 'NONE', *, *, #6408, .T. ) ;
#14681 = CYLINDRICAL_SURFACE ( 'NONE', #19990, 26.80000000000002203 ) ;
#14682 = CYLINDRICAL_SURFACE ( 'NONE', #30242, 3.200000000000001510 ) ;
#14683 = CARTESIAN_POINT ( 'NONE',  ( -7.974324478553856288, -5.875456860424912442, -27.70390402236215976 ) ) ;
#14684 = ORIENTED_EDGE ( 'NONE', *, *, #2189, .F. ) ;
#14685 = CIRCLE ( 'NONE', #5122, 4.000000000000001776 ) ;
#14686 = CYLINDRICAL_SURFACE ( 'NONE', #7505, 1.099999999999999867 ) ;
#14687 = B_SPLINE_CURVE_WITH_KNOTS ( 'NONE', 3,
 ( #17273, #12704, #27185, #15076, #10203, #24830 ),
 .UNSPECIFIED., .F., .F.,
 ( 4, 2, 4 ),
 ( 0.000000000000000000, 0.5000000000000000000, 1.000000000000000000 ),
 .UNSPECIFIED. ) ;
#14688 = CARTESIAN_POINT ( 'NONE',  ( 18.15349680648220954, 19.92137135063213549, 0.007031429000020628095 ) ) ;
#14689 = PLANE ( 'NONE',  #9448 ) ;
#14690 = ORIENTED_EDGE ( 'NONE', *, *, #7540, .F. ) ;
#14691 = CARTESIAN_POINT ( 'NONE',  ( 5.782996427689181651, 1.709881257618839356, -16.94190840230000461 ) ) ;
#14692 = CARTESIAN_POINT ( 'NONE',  ( -7.999999999651639548, -16.75746419958745648, -37.90979326505508595 ) ) ;
#14693 = EDGE_CURVE ( 'NONE', #28151, #6267, #30289, .T. ) ;
#14694 = CARTESIAN_POINT ( 'NONE',  ( 26.80000000069999899, -3.281945028320000125E-15, 87.11018146770000214 ) ) ;
#14695 = CARTESIAN_POINT ( 'NONE',  ( 23.24667624907482377, -14.69156368041588934, 225.1456731698967246 ) ) ;
#14696 = CARTESIAN_POINT ( 'NONE',  ( 27.03927834839999989, 7.087470631950000488, 222.0000000000000000 ) ) ;
#14697 = CARTESIAN_POINT ( 'NONE',  ( 22.73383167118559456, -14.19258501486319268, 5.597929191417664541 ) ) ;
#14698 = ADVANCED_FACE ( 'NONE', ( #8561 ), #20692, .F. ) ;
#14699 = DIRECTION ( 'NONE',  ( 0.9316362575375356503, 0.3633921898465274913, 0.000000000000000000 ) ) ;
#14700 = EDGE_CURVE ( 'NONE', #13976, #19663, #15818, .T. ) ;
#14701 = CYLINDRICAL_SURFACE ( 'NONE', #25780, 4.175165894169885483 ) ;
#14702 = CARTESIAN_POINT ( 'NONE',  ( 18.44986304060000037, 20.68447005859999877, 229.4485727809999673 ) ) ;
#14703 = CARTESIAN_POINT ( 'NONE',  ( -13.12132034329999897, 21.69999999990000106, -69.22132034359999864 ) ) ;
#14704 = ORIENTED_EDGE ( 'NONE', *, *, #29581, .T. ) ;
#14705 = CARTESIAN_POINT ( 'NONE',  ( 3.630871288588910506, -4.685987307826644965, -52.50430438132499944 ) ) ;
#14706 = VECTOR ( 'NONE', #2542, 1000.000000000000000 ) ;
#14707 = CARTESIAN_POINT ( 'NONE',  ( -2.299991308520000465E-10, 21.70000000000000284, -64.10000000000000853 ) ) ;
#14708 = CARTESIAN_POINT ( 'NONE',  ( 8.700000000244115128, -26.99999999999395328, -28.39999999994493862 ) ) ;
#14709 = CARTESIAN_POINT ( 'NONE',  ( 9.999999999930961891, -25.59790977665528189, -12.29094066744903557 ) ) ;
#14710 = ORIENTED_EDGE ( 'NONE', *, *, #23489, .T. ) ;
#14711 = B_SPLINE_CURVE_WITH_KNOTS ( 'NONE', 5,
 ( #3760, #29411, #29875, #27210, #8002, #7847, #5649, #14140, #6736 ),
 .UNSPECIFIED., .F., .F.,
 ( 6, 3, 6 ),
 ( 0.000000000000000000, 55.31395627320000585, 94.75474476520000167 ),
 .UNSPECIFIED. ) ;
#14712 = CARTESIAN_POINT ( 'NONE',  ( -27.50000000000000000, 3.367667473009999970E-15, 165.0000000000000000 ) ) ;
#14713 = ORIENTED_EDGE ( 'NONE', *, *, #579, .F. ) ;
#14714 = CARTESIAN_POINT ( 'NONE',  ( 10.69999999999999929, -27.00000000000000000, -28.40000000000000213 ) ) ;
#14715 = CARTESIAN_POINT ( 'NONE',  ( -4.287590041606506475, 1.413705153860729924, -69.14019511502500848 ) ) ;
#14716 = VERTEX_POINT ( 'NONE', #8720 ) ;
#14717 = CARTESIAN_POINT ( 'NONE',  ( 1.566980368899936193, 4.067530462867746444, -26.59462237480001079 ) ) ;
#14718 = CARTESIAN_POINT ( 'NONE',  ( -2.100000000000000089, -6.661338147749999512E-16, 226.6412452697800006 ) ) ;
#14719 = CARTESIAN_POINT ( 'NONE',  ( -1.143212971672622036, -4.711439499498762729, -61.94311227092499195 ) ) ;
#14720 = CARTESIAN_POINT ( 'NONE',  ( 8.700000000241654874, -24.19757157926353486, -27.32949869323976699 ) ) ;
#14721 = AXIS2_PLACEMENT_3D ( 'NONE', #18751, #9622, #11523 ) ;
#14722 = B_SPLINE_SURFACE_WITH_KNOTS ( 'NONE', 5, 5, ( 
 ( #22745, #13769, #22910, #6059, #20698, #18168 ),
 ( #3696, #15654, #18334, #25108, #10787, #3862 ),
 ( #10943, #1350, #20539, #13452, #30136, #13299 ),
 ( #23221, #30297, #29975, #27613, #20385, #3540 ),
 ( #27771, #23070, #8727, #25265, #25433, #23390 ),
 ( #9044, #13136, #8884, #28239, #11104, #13616 ) ),
 .UNSPECIFIED., .F., .F., .F.,
 ( 6, 6 ),
 ( 6, 6 ),
 ( 0.000000000000000000, 21.89975014569999701 ),
 ( -3.500000000000000000, 3.500000000000000000 ),
 .UNSPECIFIED. ) ;
#14723 = CARTESIAN_POINT ( 'NONE',  ( -4.616187199071799085, -18.92276888191837969, -28.24991812151081660 ) ) ;
#14724 = UNCERTAINTY_MEASURE_WITH_UNIT (LENGTH_MEASURE( 1.000000000000000082E-05 ), #13777, 'distance_accuracy_value', 'NONE');
#14725 = CARTESIAN_POINT ( 'NONE',  ( 8.700000000283790058, -13.49664205606710787, -34.94696692446570552 ) ) ;
#14726 = DIRECTION ( 'NONE',  ( 0.000000000000000000, -1.000000000000000000, 0.000000000000000000 ) ) ;
#14727 = ORIENTED_EDGE ( 'NONE', *, *, #30110, .F. ) ;
#14728 = DIRECTION ( 'NONE',  ( 0.000000000000000000, 0.000000000000000000, 1.000000000000000000 ) ) ;
#14729 = CARTESIAN_POINT ( 'NONE',  ( 23.73992238019999945, -12.43607998449999918, 225.0000000000000000 ) ) ;
#14730 = CARTESIAN_POINT ( 'NONE',  ( -6.635641388829999876, 10.13289756740000058, 231.9999989789999972 ) ) ;
#14731 = CARTESIAN_POINT ( 'NONE',  ( 9.999999999959999997, -29.06670649020000141, -26.22546295170000263 ) ) ;
#14732 = CARTESIAN_POINT ( 'NONE',  ( -11.95683682116932545, 1.871217339555339976, 232.0000000000048601 ) ) ;
#14733 = DIRECTION ( 'NONE',  ( 0.000000000000000000, 0.3420201433259318358, -0.9396926207858125046 ) ) ;
#14734 = CARTESIAN_POINT ( 'NONE',  ( 3.486867635905563034, -2.515642288303716168, -0.6999999999999992895 ) ) ;
#14735 = CARTESIAN_POINT ( 'NONE',  ( -27.90496282365170799, -7.855453155277750454, -0.2432540810000105580 ) ) ;
#14737 = EDGE_CURVE ( 'NONE', #9526, #20878, #12781, .T. ) ;
#14736 = CARTESIAN_POINT ( 'NONE',  ( -26.80000000000000071, -7.283063041539999493E-14, 230.0000000000000000 ) ) ;
#14738 = CARTESIAN_POINT ( 'NONE',  ( -25.77914833267782413, -15.40383343775964065, 8.000000000000007105 ) ) ;
#14739 = CARTESIAN_POINT ( 'NONE',  ( 23.50667118421176127, -14.84174322970506488, 225.1469793251989984 ) ) ;
#14740 = AXIS2_PLACEMENT_3D ( 'NONE', #30616, #28553, #28234 ) ;
#14741 =( GEOMETRIC_REPRESENTATION_CONTEXT ( 3 ) GLOBAL_UNCERTAINTY_ASSIGNED_CONTEXT ( ( #5278 ) ) GLOBAL_UNIT_ASSIGNED_CONTEXT ( ( #18011, #24957, #12680 ) ) REPRESENTATION_CONTEXT ( 'NONE', 'WORKASPACE' ) );
#14742 = CARTESIAN_POINT ( 'NONE',  ( 7.131609509308356465, -9.777910293739868308, 232.0000002394078535 ) ) ;
#14743 = CARTESIAN_POINT ( 'NONE',  ( -1.630907769230000026, -5.558498091359999727, 227.6412452697800006 ) ) ;
#14744 = DIRECTION ( 'NONE',  ( -0.7071067811865467956, -0.6644630243886068266, -0.2418447626481644297 ) ) ;
#14745 = ORIENTED_EDGE ( 'NONE', *, *, #15024, .T. ) ;
#14746 = DIRECTION ( 'NONE',  ( 0.8660254037843290176, -0.5000000000001900702, 0.000000000000000000 ) ) ;
#14747 = CARTESIAN_POINT ( 'NONE',  ( -24.80426825139999991, -14.03688870149999879, 223.9201349309999785 ) ) ;
#14748 = DIRECTION ( 'NONE',  ( -1.000000000000000000, 0.000000000000000000, 0.000000000000000000 ) ) ;
#14749 = CARTESIAN_POINT ( 'NONE',  ( 3.312932182603870679, 3.356011527877057254, -58.10805965152499653 ) ) ;
#14750 = EDGE_LOOP ( 'NONE', ( #18363, #25819, #22712, #21441, #8098, #22070 ) ) ;
#14751 = VERTEX_POINT ( 'NONE', #18328 ) ;
#14752 = CARTESIAN_POINT ( 'NONE',  ( 13.00000000000000000, 21.72305290929948640, -60.97178489257708378 ) ) ;
#14753 = ORIENTED_EDGE ( 'NONE', *, *, #30558, .F. ) ;
#14754 = AXIS2_PLACEMENT_3D ( 'NONE', #28473, #6603, #13692 ) ;
#14755 = CARTESIAN_POINT ( 'NONE',  ( -15.86808677770000209, 10.47263190749999495, -0.7999999992999995424 ) ) ;
#14756 = EDGE_CURVE ( 'NONE', #26453, #27866, #25147, .T. ) ;
#14757 = CARTESIAN_POINT ( 'NONE',  ( -23.77307140041805411, 14.41181874028064591, 4.895781291000017355 ) ) ;
#14758 = CARTESIAN_POINT ( 'NONE',  ( -27.07233446881474137, 8.380004974202883261, 2.400000000000013234 ) ) ;
#14759 = AXIS2_PLACEMENT_3D ( 'NONE', #16445, #7465, #26054 ) ;
#14760 = CARTESIAN_POINT ( 'NONE',  ( 16.27026390832094549, 11.65373091049968579, -1.400000000000002132 ) ) ;
#14761 = CARTESIAN_POINT ( 'NONE',  ( 27.50000000000000000, -3.367667472999999580E-15, 86.71909809219998522 ) ) ;
#14762 = CARTESIAN_POINT ( 'NONE',  ( 6.034652528523337445, 2.501332855249893683, -10.89261350020000130 ) ) ;
#14763 = CARTESIAN_POINT ( 'NONE',  ( 23.47715715144835613, -20.00370206646645599, 8.000000000000007105 ) ) ;
#14764 = ORIENTED_EDGE ( 'NONE', *, *, #14463, .F. ) ;
#14765 = CARTESIAN_POINT ( 'NONE',  ( 1.983129573338659579, -3.679247247662226883, -44.10000000002498410 ) ) ;
#14766 = DIRECTION ( 'NONE',  ( 0.07710832187649481473, -0.008981096902548890704, 0.9969822699505833663 ) ) ;
#14767 = CARTESIAN_POINT ( 'NONE',  ( 4.129834804009608007, 5.047645050193429128, -20.25622222230000347 ) ) ;
#14768 = CARTESIAN_POINT ( 'NONE',  ( 12.70701705218868760, 21.70000000000012363, -56.04761461377552223 ) ) ;
#14769 = CARTESIAN_POINT ( 'NONE',  ( -8.699999999702578535, -24.42241997903665407, -29.98484581762153667 ) ) ;
#14770 = DIRECTION ( 'NONE',  ( 0.7071067811865467956, -0.6644630243886068266, -0.2418447626481644297 ) ) ;
#14771 = FACE_OUTER_BOUND ( 'NONE', #2268, .T. ) ;
#14772 = CARTESIAN_POINT ( 'NONE',  ( -0.6222386373588042474, 5.469632259241050676, -47.46410749632500625 ) ) ;
#14773 = FACE_OUTER_BOUND ( 'NONE', #14794, .T. ) ;
#14774 = CARTESIAN_POINT ( 'NONE',  ( 0.4946807726542973849, -26.79522487520557661, 224.0068048305045068 ) ) ;
#14775 = CARTESIAN_POINT ( 'NONE',  ( -10.06596365874885812, -25.80632433378972124, 40.00000000000000000 ) ) ;
#14776 = CARTESIAN_POINT ( 'NONE',  ( -18.44984667599999639, 20.68448142150000280, 229.4485728150000057 ) ) ;
#14777 = TOROIDAL_SURFACE ( 'NONE', #18293, 3.176829268290000563, 0.2500000000000000000 ) ;
#14778 = EDGE_CURVE ( 'NONE', #26791, #12935, #12419, .T. ) ;
#14779 = AXIS2_PLACEMENT_3D ( 'NONE', #4669, #19303, #16931 ) ;
#14780 = AXIS2_PLACEMENT_3D ( 'NONE', #8028, #26467, #17020 ) ;
#14781 = CARTESIAN_POINT ( 'NONE',  ( -11.50000000044500048, -33.00000000000000000, -28.40000000000542002 ) ) ;
#14782 = VERTEX_POINT ( 'NONE', #23383 ) ;
#14783 = VECTOR ( 'NONE', #13287, 1000.000000000000000 ) ;
#14784 = CARTESIAN_POINT ( 'NONE',  ( 2.499950477468926291, 3.566222500441432075, -29.21106724380000230 ) ) ;
#14785 = VERTEX_POINT ( 'NONE', #4012 ) ;
#14786 = CARTESIAN_POINT ( 'NONE',  ( -10.00000000063852035, -42.68965130439637790, -27.18132884625137535 ) ) ;
#14787 = CARTESIAN_POINT ( 'NONE',  ( -2.571638601809289160, 3.775240214263653193, -48.45391720702500749 ) ) ;
#14788 = VERTEX_POINT ( 'NONE', #18481 ) ;
#14789 = VERTEX_POINT ( 'NONE', #23215 ) ;
#14790 = EDGE_CURVE ( 'NONE', #28212, #20745, #5258, .T. ) ;
#14791 = SHAPE_DEFINITION_REPRESENTATION ( #30767, #6935 ) ;
#14792 = VERTEX_POINT ( 'NONE', #16583 ) ;
#14793 = CARTESIAN_POINT ( 'NONE',  ( 20.29863583259346527, 20.00004025424676612, 229.1322715859966195 ) ) ;
#14794 = EDGE_LOOP ( 'NONE', ( #4341, #5581, #2795, #2637 ) ) ;
#14795 =( GEOMETRIC_REPRESENTATION_CONTEXT ( 3 ) GLOBAL_UNCERTAINTY_ASSIGNED_CONTEXT ( ( #26380 ) ) GLOBAL_UNIT_ASSIGNED_CONTEXT ( ( #93, #19119, #28864 ) ) REPRESENTATION_CONTEXT ( 'NONE', 'WORKASPACE' ) );
#14796 = CARTESIAN_POINT ( 'NONE',  ( -10.00000000001762146, -17.77478083485818061, -34.71627511726088500 ) ) ;
#14797 = CARTESIAN_POINT ( 'NONE',  ( 2.219613442066579623, 3.155516745171627058, 227.8440641264181750 ) ) ;
#14798 = EDGE_CURVE ( 'NONE', #29336, #7923, #25599, .T. ) ;
#14799 = CARTESIAN_POINT ( 'NONE',  ( 9.999999999959999997, -29.30501631460000311, -26.47986984960000001 ) ) ;
#14800 = CARTESIAN_POINT ( 'NONE',  ( 1.155622926759880986, 3.934465103449412915, -35.69999999999999574 ) ) ;
#14801 = CARTESIAN_POINT ( 'NONE',  ( -12.40641005330639501, -30.64563522679841867, -24.73155443112704432 ) ) ;
#14802 = CARTESIAN_POINT ( 'NONE',  ( -23.77307140041805411, 14.41181874028064591, 4.999998581000003384 ) ) ;
#14803 = CARTESIAN_POINT ( 'NONE',  ( -10.00000000070000183, -27.00000000000000000, -25.39999999999999858 ) ) ;
#14804 = CIRCLE ( 'NONE', #25866, 27.50000000000000000 ) ;
#14805 = CARTESIAN_POINT ( 'NONE',  ( -10.69999999999999929, -27.00000000000000000, -28.40000000000000213 ) ) ;
#14806 = AXIS2_PLACEMENT_3D ( 'NONE', #15774, #30575, #11063 ) ;
#14807 = ORIENTED_EDGE ( 'NONE', *, *, #8533, .T. ) ;
#14808 = VECTOR ( 'NONE', #12331, 1000.000000000000114 ) ;
#14809 = CARTESIAN_POINT ( 'NONE',  ( -4.932711197237716227, 1.396981812416056457, -8.248327254899997740 ) ) ;
#14810 = CARTESIAN_POINT ( 'NONE',  ( 2.749945525234485988, 3.922844750473964748, -28.27356724379999875 ) ) ;
#14811 = CIRCLE ( 'NONE', #23798, 1.700000000000000178 ) ;
#14812 = DIRECTION ( 'NONE',  ( 6.326189572192215265E-12, 0.3568421334038983650, -0.9341647027306021478 ) ) ;
#14813 = DIRECTION ( 'NONE',  ( 0.8660254037843290176, 0.5000000000001899592, 1.018673689593249976E-32 ) ) ;
#14814 = CARTESIAN_POINT ( 'NONE',  ( 24.43659368183839931, 14.66646236428692340, 6.099998581000020792 ) ) ;
#14815 = CARTESIAN_POINT ( 'NONE',  ( -2.299991308520000465E-10, 21.70000000000000284, -60.10000000000000142 ) ) ;
#14816 = CARTESIAN_POINT ( 'NONE',  ( -4.363437395929419260, 0.1294788321584625090, -13.18304957890000573 ) ) ;
#14817 = ADVANCED_FACE ( 'NONE', ( #14234 ), #4627, .F. ) ;
#14818 = CARTESIAN_POINT ( 'NONE',  ( 9.999999999964986230, -24.37875421243714058, -26.88867997429543166 ) ) ;
#14819 =( REPRESENTATION_RELATIONSHIP ('NONE','NONE', #2712, #19806 ) REPRESENTATION_RELATIONSHIP_WITH_TRANSFORMATION ( #7201 )SHAPE_REPRESENTATION_RELATIONSHIP( ) );
#14820 = CARTESIAN_POINT ( 'NONE',  ( -24.14840830027331364, -13.77363891130890039, 4.098702617000016701 ) ) ;
#14821 = CARTESIAN_POINT ( 'NONE',  ( 10.69999999930000101, -25.00000000000000000, -26.16393202249999916 ) ) ;
#14822 = AXIS2_PLACEMENT_3D ( 'NONE', #30280, #11240, #23372 ) ;
#14823 = ORIENTED_EDGE ( 'NONE', *, *, #10210, .F. ) ;
#14824 =( GEOMETRIC_REPRESENTATION_CONTEXT ( 3 ) GLOBAL_UNCERTAINTY_ASSIGNED_CONTEXT ( ( #4965 ) ) GLOBAL_UNIT_ASSIGNED_CONTEXT ( ( #4773, #11847, #19238 ) ) REPRESENTATION_CONTEXT ( 'NONE', 'WORKASPACE' ) );
#14825 = EDGE_CURVE ( 'NONE', #17991, #1011, #7157, .T. ) ;
#14826 = DIRECTION ( 'NONE',  ( 0.000000000000000000, 0.000000000000000000, -1.000000000000000000 ) ) ;
#14827 = CARTESIAN_POINT ( 'NONE',  ( 13.99999999977382359, 20.99999999989910293, -67.49269908208931668 ) ) ;
#14828 = ORIENTED_EDGE ( 'NONE', *, *, #26734, .T. ) ;
#14829 = B_SPLINE_SURFACE_WITH_KNOTS ( 'NONE', 5, 5, ( 
 ( #27838, #30680, #8634, #1731, #28307, #23608, #23137, #11167, #8798 ),
 ( #28157, #18708, #2044, #18230, #11634, #27997, #21233, #30832, #28465 ),
 ( #18868, #6902, #16505, #4978, #5588, #26842, #22439, #2617, #24793 ),
 ( #7945, #20076, #19767, #21978, #12209, #29352, #884, #17688, #29508 ),
 ( #22278, #24333, #275, #24487, #5745, #17544, #26998, #21821, #586 ),
 ( #15348, #26686, #9856, #12671, #7640, #19454, #15189, #29046, #5125 ),
 ( #3229, #24640, #2926, #19611, #29192, #27155, #17395, #7492, #17086 ),
 ( #10480, #5292, #12368, #3073, #14735, #15048, #2777, #434, #12836 ),
 ( #7795, #5438, #736, #10014, #14895, #29666, #10327, #17237, #8096 ) ),
 .UNSPECIFIED., .F., .F., .F.,
 ( 6, 3, 6 ),
 ( 6, 3, 6 ),
 ( 0.000000000000000000, 54.03331039209999886, 92.56095350929999199 ),
 ( 8.011061266649999624, 9.405960541640000727, 10.80085981660000094 ),
 .UNSPECIFIED. ) ;
#14830 = CARTESIAN_POINT ( 'NONE',  ( -20.30396346370000060, 20.00000000000000000, 229.0000000000000000 ) ) ;
#14831 = CARTESIAN_POINT ( 'NONE',  ( 7.867249199797543113, -115.3182685132986904, 21.51331176843062210 ) ) ;
#14832 = VECTOR ( 'NONE', #13811, 999.9999999999998863 ) ;
#14833 = EDGE_LOOP ( 'NONE', ( #26064, #24461, #30343, #3354 ) ) ;
#14834 = CARTESIAN_POINT ( 'NONE',  ( -11.69999999989999928, -2.500000000000002220, -0.6999999999999992895 ) ) ;
#14835 = CIRCLE ( 'NONE', #23319, 26.79999999889999884 ) ;
#14836 = EDGE_LOOP ( 'NONE', ( #26404, #525, #3016, #13145, #9086, #29208, #26016 ) ) ;
#14837 = ORIENTED_EDGE ( 'NONE', *, *, #23107, .T. ) ;
#14838 =( LENGTH_UNIT ( ) NAMED_UNIT ( * ) SI_UNIT ( .MILLI., .METRE. ) );
#14839 = ORIENTED_EDGE ( 'NONE', *, *, #7528, .T. ) ;
#14840 = CARTESIAN_POINT ( 'NONE',  ( 13.99999999979999821, 20.99999999999999645, -51.10000000000000142 ) ) ;
#14841 = EDGE_CURVE ( 'NONE', #1598, #17245, #21509, .T. ) ;
#14842 = CARTESIAN_POINT ( 'NONE',  ( 0.000000000000000000, -17.25771824150000100, 225.0000000000000000 ) ) ;
#14843 = CARTESIAN_POINT ( 'NONE',  ( 8.000000000111514353, -60.34578018690848467, -2.533826264238200121 ) ) ;
#14844 = ORIENTED_EDGE ( 'NONE', *, *, #18852, .T. ) ;
#14845 = CARTESIAN_POINT ( 'NONE',  ( -25.32653162617393861, 13.07087917251410403, 5.760266710000017554 ) ) ;
#14846 = DIRECTION ( 'NONE',  ( -1.000000000000000000, 0.000000000000000000, 0.000000000000000000 ) ) ;
#14847 = CARTESIAN_POINT ( 'NONE',  ( -7.999999999674140660, -13.61361098168129224, -34.64062768038885309 ) ) ;
#14848 = AXIS2_PLACEMENT_3D ( 'NONE', #12016, #7140, #16722 ) ;
#14849 = CYLINDRICAL_SURFACE ( 'NONE', #1912, 3.749999999999999556 ) ;
#14850 = ORIENTED_EDGE ( 'NONE', *, *, #11985, .F. ) ;
#14851 = EDGE_CURVE ( 'NONE', #30214, #23190, #17474, .T. ) ;
#14852 = CARTESIAN_POINT ( 'NONE',  ( -10.69999999994010587, -26.89373798101190616, -15.86471592097247019 ) ) ;
#14853 = CARTESIAN_POINT ( 'NONE',  ( 0.5830502407437251344, -4.723335260236232180, -17.43304674910000429 ) ) ;
#14854 = CARTESIAN_POINT ( 'NONE',  ( -7.999999999650055926, -15.51869328868451170, -38.00326546224398783 ) ) ;
#14855 = CARTESIAN_POINT ( 'NONE',  ( -27.63177371730000331, 3.383804566159999695E-15, 142.6394760449999808 ) ) ;
#14856 = CARTESIAN_POINT ( 'NONE',  ( 4.590690989210701289, -18.41552811670975487, -28.49731597295215479 ) ) ;
#14857 = LINE ( 'NONE', #5087, #26306 ) ;
#14858 = CARTESIAN_POINT ( 'NONE',  ( -24.64320960688972306, 12.86800382723239622, 4.117082646578299254 ) ) ;
#14859 = CARTESIAN_POINT ( 'NONE',  ( 1.998401444330000344E-15, 2.100000000000000089, 227.6412452697800006 ) ) ;
#14860 = LINE ( 'NONE', #19888, #11708 ) ;
#14861 = ADVANCED_FACE ( 'NONE', ( #11564, #2121, #21161 ), #9187, .F. ) ;
#14862 = FACE_OUTER_BOUND ( 'NONE', #4344, .T. ) ;
#14863 = CARTESIAN_POINT ( 'NONE',  ( -14.43445815169999946, 11.21795253560000027, 230.6999999999999886 ) ) ;
#14864 = ORIENTED_EDGE ( 'NONE', *, *, #1535, .T. ) ;
#14865 = CARTESIAN_POINT ( 'NONE',  ( -4.213298386699523945, 4.800796338101376293, -53.98587006832499924 ) ) ;
#14866 = CARTESIAN_POINT ( 'NONE',  ( -10.69999999999999929, -130.0000000000000000, -41.82335799894999440 ) ) ;
#14867 = CARTESIAN_POINT ( 'NONE',  ( -24.71034964618677776, 13.49086583186187660, 0.2686791940000321510 ) ) ;
#14868 = CARTESIAN_POINT ( 'NONE',  ( -4.579986235535789874, 0.9295504054295574692, -68.10000000002499121 ) ) ;
#14869 = PRODUCT_DEFINITION_FORMATION_WITH_SPECIFIED_SOURCE ( 'ANY', '', #9142, .NOT_KNOWN. ) ;
#14870 = ORIENTED_EDGE ( 'NONE', *, *, #1903, .T. ) ;
#14871 = CARTESIAN_POINT ( 'NONE',  ( -3.045581262757260266, 1.082242280537820678, -94.56600524946087205 ) ) ;
#14872 =( NAMED_UNIT ( * ) SI_UNIT ( $, .STERADIAN. ) SOLID_ANGLE_UNIT ( ) );
#14873 = VERTEX_POINT ( 'NONE', #18946 ) ;
#14874 = CARTESIAN_POINT ( 'NONE',  ( 0.000000000000000000, 0.000000000000000000, 229.6412452697800006 ) ) ;
#14875 = ADVANCED_FACE ( 'NONE', ( #31068 ), #24141, .F. ) ;
#14876 = DIRECTION ( 'NONE',  ( 1.000000000000000000, 0.000000000000000000, -2.257150022439999944E-12 ) ) ;
#14877 = VERTEX_POINT ( 'NONE', #390 ) ;
#14878 = CARTESIAN_POINT ( 'NONE',  ( 4.807767551039155762, 1.738376938488521040, -27.44999766020000465 ) ) ;
#14879 = CARTESIAN_POINT ( 'NONE',  ( -3.552713678799999608E-15, -3.552713678799999608E-15, 193.6055512750000105 ) ) ;
#14880 = ADVANCED_FACE ( 'NONE', ( #23994 ), #27531, .T. ) ;
#14881 = B_SPLINE_CURVE_WITH_KNOTS ( 'NONE', 3,
 ( #9678, #17981, #865, #15631, #3514, #27592, #13112, #20053, #20516, #24931, #5725, #10922 ),
 .UNSPECIFIED., .F., .F.,
 ( 4, 2, 2, 2, 2, 4 ),
 ( 0.000000000000000000, 0.2499999999999997224, 0.4999999999999996669, 0.6249999999999997780, 0.7499999999999997780, 1.000000000000000000 ),
 .UNSPECIFIED. ) ;
#14882 = CARTESIAN_POINT ( 'NONE',  ( -3.108138112192390778, -3.359256988581870385, -50.19612412472499585 ) ) ;
#14883 = FACE_OUTER_BOUND ( 'NONE', #10997, .T. ) ;
#14884 = CARTESIAN_POINT ( 'NONE',  ( -4.861208984456414584, -17.82998039991930028, -28.78290667659118540 ) ) ;
#14885 = CARTESIAN_POINT ( 'NONE',  ( 3.257018533420329653, 1.358678418917213637, 230.8224594091670383 ) ) ;
#14886 = CARTESIAN_POINT ( 'NONE',  ( -17.30352168678310676, -22.00035733197351107, -26.55503778092711187 ) ) ;
#14887 = ORIENTED_EDGE ( 'NONE', *, *, #677, .T. ) ;
#14888 = LINE ( 'NONE', #8089, #16194 ) ;
#14889 = DIRECTION ( 'NONE',  ( -7.759996349202911684E-13, -0.9341647027306021478, -0.3568421334038983650 ) ) ;
#14890 = CARTESIAN_POINT ( 'NONE',  ( -2.860892586589999897, -11.94945454729999845, 232.6627643349999914 ) ) ;
#14891 = DIRECTION ( 'NONE',  ( 0.000000000000000000, 0.000000000000000000, -1.000000000000000000 ) ) ;
#14892 = CARTESIAN_POINT ( 'NONE',  ( -11.28407061768355568, -4.374602998566188283, 232.0000000000047464 ) ) ;
#14893 = CARTESIAN_POINT ( 'NONE',  ( 2.131628207279999844E-14, -5.329070518200000398E-15, 86.78285841159998881 ) ) ;
#14894 = CARTESIAN_POINT ( 'NONE',  ( 3.075842487415840765, -2.801017835266844891, -0.6999999999999992895 ) ) ;
#14895 = CARTESIAN_POINT ( 'NONE',  ( -28.03861306157277866, -0.5101735396242147447, -0.2432540810000105580 ) ) ;
#14896 = DIRECTION ( 'NONE',  ( 1.000000000000000000, 0.000000000000000000, 0.000000000000000000 ) ) ;
#14897 = DIRECTION ( 'NONE',  ( -0.2815395311429196301, -0.9595496299847262600, 0.000000000000000000 ) ) ;
#14898 = CARTESIAN_POINT ( 'NONE',  ( 2.020725942159999899, -3.500000000000000000, 230.5235986622430175 ) ) ;
#14899 = DIRECTION ( 'NONE',  ( -1.553705081258627072E-12, -0.7253743710120287291, 0.6883545756940268046 ) ) ;
#14900 = CARTESIAN_POINT ( 'NONE',  ( 0.3030197492349069321, -3.973671256962546749, -68.10000000002499121 ) ) ;
#14901 = ORIENTED_EDGE ( 'NONE', *, *, #14463, .T. ) ;
#14902 = CARTESIAN_POINT ( 'NONE',  ( 10.40384844070000092, -24.69832375569999883, -1.291913789700005477 ) ) ;
#14903 = CARTESIAN_POINT ( 'NONE',  ( -24.73474822280000041, -14.15859640590000090, 223.9040321390000088 ) ) ;
#14904 = CARTESIAN_POINT ( 'NONE',  ( 24.46818569879999927, -13.19686604630000026, 225.7601281139999969 ) ) ;
#14905 = EDGE_CURVE ( 'NONE', #26188, #5639, #26497, .T. ) ;
#14906 = CARTESIAN_POINT ( 'NONE',  ( 1.169850847344618083, -6.301966510834352775, -59.22125695792499300 ) ) ;
#14907 = EDGE_LOOP ( 'NONE', ( #5379, #5139 ) ) ;
#14908 = ORIENTED_EDGE ( 'NONE', *, *, #9712, .T. ) ;
#14909 = EDGE_CURVE ( 'NONE', #6775, #17179, #233, .T. ) ;
#14910 = DIRECTION ( 'NONE',  ( 0.000000000000000000, -2.259525899719999991E-12, -1.000000000000000000 ) ) ;
#14911 = ADVANCED_FACE ( 'NONE', ( #29157 ), #19107, .T. ) ;
#14912 = ORIENTED_EDGE ( 'NONE', *, *, #19856, .T. ) ;
#14913 = CARTESIAN_POINT ( 'NONE',  ( 1.776356839399999922E-14, 0.000000000000000000, 232.0000000000000000 ) ) ;
#14914 = CARTESIAN_POINT ( 'NONE',  ( -24.81746041937532965, 14.01353061208509310, 3.920132063000014710 ) ) ;
#14915 = CARTESIAN_POINT ( 'NONE',  ( -19.80535357367646654, 19.50875577052770993, 2.400000000000013234 ) ) ;
#14916 = B_SPLINE_SURFACE_WITH_KNOTS ( 'NONE', 5, 1, ( 
 ( #30249, #22862 ),
 ( #6014, #15929 ),
 ( #8519, #1467 ),
 ( #29774, #8205 ),
 ( #30093, #27416 ),
 ( #30417, #27724 ),
 ( #10900, #11058 ),
 ( #13570, #5854 ),
 ( #15458, #25063 ) ),
 .UNSPECIFIED., .F., .F., .F.,
 ( 6, 3, 6 ),
 ( 2, 2 ),
 ( 0.000000000000000000, 53.95537973340000093, 92.42745556099998794 ),
 ( -3.500000000000000000, 3.500000000000000000 ),
 .UNSPECIFIED. ) ;
#14917 = CARTESIAN_POINT ( 'NONE',  ( 17.82030331447854010, 11.89630849604035845, -1.400000000000001910 ) ) ;
#14918 = FACE_OUTER_BOUND ( 'NONE', #20351, .T. ) ;
#14919 = CARTESIAN_POINT ( 'NONE',  ( 4.880902371519058036, -3.592936783560450653, -8.372776792900001652 ) ) ;
#14920 = DIRECTION ( 'NONE',  ( 0.000000000000000000, 0.000000000000000000, -1.000000000000000000 ) ) ;
#14921 = ORIENTED_EDGE ( 'NONE', *, *, #4802, .F. ) ;
#14922 = CARTESIAN_POINT ( 'NONE',  ( 2.613626818191559398, -3.470008059885128837, -44.10000000002499121 ) ) ;
#14923 = CARTESIAN_POINT ( 'NONE',  ( 24.61381495443087175, 14.36755986787189521, 3.957524335000017768 ) ) ;
#14924 = CARTESIAN_POINT ( 'NONE',  ( -5.635022120040177995, 0.7837540840564873879, -20.25159460730000305 ) ) ;
#14925 = CARTESIAN_POINT ( 'NONE',  ( -12.34115088265052940, -23.82565491187611428, -32.34044972036594601 ) ) ;
#14926 = CARTESIAN_POINT ( 'NONE',  ( -8.699999999707589637, -24.26136093481122558, -29.62468611113576955 ) ) ;
#14927 = DIRECTION ( 'NONE',  ( -0.3633921898465274913, 0.9316362575375355393, 0.000000000000000000 ) ) ;
#14928 = CARTESIAN_POINT ( 'NONE',  ( 0.8694071509298356704, -27.78660432966791660, 224.3226506338012882 ) ) ;
#14929 = CARTESIAN_POINT ( 'NONE',  ( -2.393684743089945055, 3.904820337558672083, -44.65531229042500172 ) ) ;
#14930 = LINE ( 'NONE', #2656, #19256 ) ;
#14931 = FACE_OUTER_BOUND ( 'NONE', #21288, .T. ) ;
#14932 = FACE_OUTER_BOUND ( 'NONE', #24191, .T. ) ;
#14933 = CARTESIAN_POINT ( 'NONE',  ( -26.94142135619999934, 4.542738371190000457, 230.0000000000000000 ) ) ;
#14934 = EDGE_CURVE ( 'NONE', #19754, #9128, #14549, .T. ) ;
#14935 = LINE ( 'NONE', #24533, #30346 ) ;
#14936 = ORIENTED_EDGE ( 'NONE', *, *, #12718, .F. ) ;
#14937 = CARTESIAN_POINT ( 'NONE',  ( -5.864216825196034932, 1.669623860970033347, -31.30158078969999380 ) ) ;
#14938 = ORIENTED_EDGE ( 'NONE', *, *, #25123, .T. ) ;
#14939 = CARTESIAN_POINT ( 'NONE',  ( 25.45799949673341800, -12.81261086040661645, 4.791562841999996714 ) ) ;
#14940 = CARTESIAN_POINT ( 'NONE',  ( -3.501023913647623331, -3.402888588040827500, -47.95083066912501124 ) ) ;
#14941 = ORIENTED_EDGE ( 'NONE', *, *, #26372, .F. ) ;
#14942 = ORIENTED_EDGE ( 'NONE', *, *, #21502, .F. ) ;
#14943 = AXIS2_PLACEMENT_3D ( 'NONE', #17184, #28830, #26949 ) ;
#14944 = DIRECTION ( 'NONE',  ( -0.1684282417370463469, -0.2917262721179094687, -0.9415560044636510639 ) ) ;
#14945 = ORIENTED_EDGE ( 'NONE', *, *, #27192, .F. ) ;
#14946 = VECTOR ( 'NONE', #7095, 1000.000000000000000 ) ;
#14947 = CARTESIAN_POINT ( 'NONE',  ( -8.699999999730728462, -26.13380090399637368, -25.50104989788441756 ) ) ;
#14948 = B_SPLINE_CURVE_WITH_KNOTS ( 'NONE', 3,
 ( #236, #24607, #17054, #10288, #19890, #29471 ),
 .UNSPECIFIED., .F., .F.,
 ( 4, 2, 4 ),
 ( 0.000000000000000000, 0.5000000000000000000, 1.000000000000000000 ),
 .UNSPECIFIED. ) ;
#14949 = ORIENTED_EDGE ( 'NONE', *, *, #27942, .F. ) ;
#14950 = CARTESIAN_POINT ( 'NONE',  ( -11.78524365341753466, 20.99999999990017585, -70.02191802985640834 ) ) ;
#14951 = CARTESIAN_POINT ( 'NONE',  ( 12.80098767942999771, -27.00000000059169736, -22.62649730765999578 ) ) ;
#14952 = CARTESIAN_POINT ( 'NONE',  ( 27.51770821245201759, 4.728187301810311105, 8.000000000000007105 ) ) ;
#14953 = CARTESIAN_POINT ( 'NONE',  ( -27.50000000000000000, 3.367667473009999970E-15, 86.71909809219998522 ) ) ;
#14954 = CARTESIAN_POINT ( 'NONE',  ( -12.37073348361184699, -30.41559816918431025, -24.59878346509346159 ) ) ;
#14955 = CARTESIAN_POINT ( 'NONE',  ( 9.499999999888803615, -15.21984422747265420, -37.76664074417031713 ) ) ;
#14956 = CARTESIAN_POINT ( 'NONE',  ( 0.5877407897813119453, -4.297347728519514298, 0.1268759519999947127 ) ) ;
#14957 = CARTESIAN_POINT ( 'NONE',  ( -10.69999999995573958, -32.31934595230423923, -22.79266741176987310 ) ) ;
#14958 = ORIENTED_EDGE ( 'NONE', *, *, #12558, .T. ) ;
#14959 = CARTESIAN_POINT ( 'NONE',  ( -2.014747437493234816, 4.354226950121528716, -8.669225184300003662 ) ) ;
#14960 = CARTESIAN_POINT ( 'NONE',  ( 1.844957972340690588, -5.198917526286033208, -29.25632401680000427 ) ) ;
#14961 = CARTESIAN_POINT ( 'NONE',  ( -7.482225056410205077, -15.92425073469576979, -74.67428281938484247 ) ) ;
#14962 = CARTESIAN_POINT ( 'NONE',  ( 24.27467683999808301, -13.55001166052597128, 6.095967889000020179 ) ) ;
#14963 = EDGE_CURVE ( 'NONE', #2713, #28317, #30565, .T. ) ;
#14964 = CARTESIAN_POINT ( 'NONE',  ( 24.31416967338466861, 13.47842985269137728, 5.506973475999988210 ) ) ;
#14965 = DIRECTION ( 'NONE',  ( 0.000000000000000000, -1.000000000000000000, 2.257145581549999994E-12 ) ) ;
#14966 = CARTESIAN_POINT ( 'NONE',  ( -27.29823224880000154, -3.596834937749999341E-14, 230.6577119970000069 ) ) ;
#14967 = CARTESIAN_POINT ( 'NONE',  ( -8.699999999730072986, -28.07050130677435362, -25.59757157925566773 ) ) ;
#14968 = EDGE_CURVE ( 'NONE', #17625, #15429, #7859, .T. ) ;
#14969 = AXIS2_PLACEMENT_3D ( 'NONE', #3762, #11471, #20916 ) ;
#14970 = CIRCLE ( 'NONE', #1402, 3.200000000000000178 ) ;
#14971 = CARTESIAN_POINT ( 'NONE',  ( 16.40025437452154478, 10.19782190223724072, -1.400000000000001910 ) ) ;
#14972 = CARTESIAN_POINT ( 'NONE',  ( 6.339027081030000540E-10, -4.118494162357343669, -70.37733883405731206 ) ) ;
#14973 = CARTESIAN_POINT ( 'NONE',  ( 0.9263908148115145291, -3.499834818479312659, 230.7667222917537515 ) ) ;
#14974 = AXIS2_PLACEMENT_3D ( 'NONE', #2068, #4272, #6466 ) ;
#14975 = ORIENTED_EDGE ( 'NONE', *, *, #2577, .F. ) ;
#14976 = EDGE_CURVE ( 'NONE', #17664, #8508, #3405, .T. ) ;
#14977 = DIRECTION ( 'NONE',  ( -1.000000000000000000, 0.000000000000000000, 0.000000000000000000 ) ) ;
#14978 = CARTESIAN_POINT ( 'NONE',  ( -3.304042416708073304, -20.19592245937915109, -27.62895963153397716 ) ) ;
#14979 = ORIENTED_EDGE ( 'NONE', *, *, #18525, .F. ) ;
#14980 = CARTESIAN_POINT ( 'NONE',  ( 25.41371745730516807, 13.31556240574341210, 8.000000000000007105 ) ) ;
#14981 = EDGE_LOOP ( 'NONE', ( #15241, #10885, #2628, #640 ) ) ;
#14982 = CARTESIAN_POINT ( 'NONE',  ( 10.00000000005000267, -14.23127763357968156, -74.05809100316466242 ) ) ;
#14983 = ORIENTED_EDGE ( 'NONE', *, *, #23382, .T. ) ;
#14984 = EDGE_LOOP ( 'NONE', ( #8337, #19527, #3245, #12074, #29601, #16335, #19960 ) ) ;
#14985 = CIRCLE ( 'NONE', #20007, 4.175165894169885483 ) ;
#14986 = ORIENTED_EDGE ( 'NONE', *, *, #10579, .T. ) ;
#14987 = CARTESIAN_POINT ( 'NONE',  ( 24.15098795939999832, 13.41224477779999980, 230.6999999999999886 ) ) ;
#14988 = CARTESIAN_POINT ( 'NONE',  ( -28.49999999970000175, 7.466149641070000342, 229.0000000000000000 ) ) ;
#14989 = ADVANCED_FACE ( 'NONE', ( #9658 ), #17197, .F. ) ;
#14990 = CARTESIAN_POINT ( 'NONE',  ( -10.69999999999999929, -24.92624642180000194, -26.23177034519999751 ) ) ;
#14991 = ORIENTED_EDGE ( 'NONE', *, *, #4833, .T. ) ;
#14992 = CARTESIAN_POINT ( 'NONE',  ( -24.73569401515663202, 12.68911708161206953, 5.680831397999991594 ) ) ;
#14993 = CARTESIAN_POINT ( 'NONE',  ( 20.77600629922060449, 21.68409807857484140, 1.000000000000000888 ) ) ;
#14994 = AXIS2_PLACEMENT_3D ( 'NONE', #7296, #800, #19980 ) ;
#14995 = CARTESIAN_POINT ( 'NONE',  ( -17.45884911675408091, -31.99970210406505444, -27.62116137362975721 ) ) ;
#14996 = ORIENTED_EDGE ( 'NONE', *, *, #1892, .F. ) ;
#14997 = DIRECTION ( 'NONE',  ( 0.9316362575375356503, 0.3633921898465274913, 0.000000000000000000 ) ) ;
#14998 = CARTESIAN_POINT ( 'NONE',  ( 4.324151835433248436, -2.064520475586355985, -19.94430150030000348 ) ) ;
#14999 = CARTESIAN_POINT ( 'NONE',  ( 20.64716981389999972, -20.77933506589999979, 229.0000000020000073 ) ) ;
#15000 = CARTESIAN_POINT ( 'NONE',  ( -4.276011752185619130, -51.11187400311629858, -27.80500476125005704 ) ) ;
#15001 = LINE ( 'NONE', #24447, #28256 ) ;
#15002 = DIRECTION ( 'NONE',  ( 0.5193310806158223381, 1.929012505286207873E-12, 0.8545731265997089654 ) ) ;
#15003 = CYLINDRICAL_SURFACE ( 'NONE', #3177, 5.000000000000003553 ) ;
#15004 = VECTOR ( 'NONE', #3598, 1000.000000000000000 ) ;
#15005 = B_SPLINE_CURVE_WITH_KNOTS ( 'NONE', 3,
 ( #21697, #16650, #5008, #6896, #26567, #24061, #12088, #146, #9727, #14616, #21857, #308, #9886, #19488, #23755, #3258, #29845, #20245, #917, #15072, #24364, #12863, #26716, #17422, #2955, #12549, #3409, #5318, #5774, #17574, #463, #10654, #24518, #3102, #1063, #5619, #2805, #612, #27029, #10507, #22007, #19945, #17115, #12397, #5465, #24668, #22155, #10198, #19798, #12698, #29383, #14922, #22310, #24824, #762, #10045, #10353, #5152, #22465, #29539, #7973, #7823, #27180, #20107, #13011, #15219, #29695, #14765, #8122, #15376, #19639, #17717, #29225, #27335, #24973, #22623, #7665, #17268, #26877, #1537, #18029, #18364, #30159, #25767, #27797, #8431, #11441, #23095, #17873 ),
 .UNSPECIFIED., .F., .F.,
 ( 4, 2, 2, 2, 2, 2, 2, 1, 1, 2, 2, 1, 1, 1, 1, 2, 2, 1, 1, 1, 2, 2, 2, 2, 2, 2, 1, 1, 2, 2, 1, 1, 1, 2, 2, 1, 2, 2, 1, 1, 1, 1, 2, 2, 1, 1, 2, 2, 1, 1, 2, 2, 1, 1, 2, 2, 4 ),
 ( 0.000000000000000000, 0.03125000000000302536, 0.06250000000000605072, 0.1250000000000121569, 0.1875000000000182632, 0.2500000000000243694, 0.3125000000000304756, 0.3437500000000335287, 0.3593750000000350830, 0.3671875000000358602, 0.3750000000000366929, 0.4062500000000395795, 0.4218750000000410227, 0.4296875000000416889, 0.4335937500000420775, 0.4355468750000421885, 0.4375000000000422440, 0.4531250000000427991, 0.4609375000000430767, 0.4648437500000431877, 0.4667968750000431877, 0.4687500000000431877, 0.4765625000000434097, 0.4843750000000436318, 0.4921875000000437983, 0.5000000000000439648, 0.5078125000000442979, 0.5117187500000442979, 0.5136718750000442979, 0.5156250000000442979, 0.5234375000000442979, 0.5273437500000444089, 0.5292968750000445199, 0.5302734375000445199, 0.5312500000000446310, 0.5468750000000431877, 0.5546875000000425215, 0.5625000000000417444, 0.5781250000000404121, 0.5859375000000397460, 0.5898437500000394129, 0.5917968750000394129, 0.5927734375000394129, 0.5937500000000394129, 0.6093750000000378586, 0.6171875000000370814, 0.6210937500000367484, 0.6250000000000363043, 0.6875000000000303091, 0.7187500000000274225, 0.7343750000000258682, 0.7500000000000244249, 0.8125000000000183187, 0.8437500000000153211, 0.8593750000000137668, 0.8750000000000123235, 1.000000000000000000 ),
 .UNSPECIFIED. ) ;
#15007 = CARTESIAN_POINT ( 'NONE',  ( 11.69999999989999928, -25.00000000000000000, -2.399999999999999467 ) ) ;
#15006 = B_SPLINE_CURVE_WITH_KNOTS ( 'NONE', 3,
 ( #18245, #15431, #8490, #3943, #5984, #17926, #11177, #25186, #6453, #30383, #1745, #3619, #13536, #6138, #20776, #22827, #23147, #1590, #22987, #6304 ),
 .UNSPECIFIED., .F., .F.,
 ( 4, 1, 1, 1, 2, 2, 2, 1, 1, 1, 2, 2, 4 ),
 ( 0.000000000000000000, 0.1250000000000261458, 0.1875000000000392186, 0.2187500000000439648, 0.2343750000000447697, 0.2500000000000455747, 0.5000000000000199840, 0.6250000000000072164, 0.6875000000000016653, 0.7187500000000001110, 0.7343749999999980016, 0.7499999999999957812, 1.000000000000000000 ),
 .UNSPECIFIED. ) ;
#15008 = CARTESIAN_POINT ( 'NONE',  ( 27.79999999980000069, 4.694479351150000035, 229.1414213560000235 ) ) ;
#15009 = DIRECTION ( 'NONE',  ( 0.1090476345695675503, 0.6986477033489619792, 0.7071067811865496822 ) ) ;
#15010 = ORIENTED_EDGE ( 'NONE', *, *, #13033, .T. ) ;
#15011 = CARTESIAN_POINT ( 'NONE',  ( -0.9891938378274525157, -4.753657830815115837, -52.92706695232499925 ) ) ;
#15012 = VECTOR ( 'NONE', #13383, 1000.000000000000000 ) ;
#15013 = CARTESIAN_POINT ( 'NONE',  ( 9.897162125334208582, -25.37356426560172196, 191.6604601750000256 ) ) ;
#15014 = EDGE_CURVE ( 'NONE', #22416, #27419, #7306, .T. ) ;
#15015 = CARTESIAN_POINT ( 'NONE',  ( -24.95150188576461403, 13.62250486174595920, 0.8585803919999857037 ) ) ;
#15016 = CIRCLE ( 'NONE', #19053, 1.472846691535505848 ) ;
#15017 = CARTESIAN_POINT ( 'NONE',  ( -4.718533212916164565, 0.6243469615916787951, -68.10000000002501963 ) ) ;
#15018 = ORIENTED_EDGE ( 'NONE', *, *, #21062, .T. ) ;
#15019 = CARTESIAN_POINT ( 'NONE',  ( 23.92402432539614310, -13.56054118960007493, 6.087706803184607551 ) ) ;
#15020 = SURFACE_STYLE_USAGE ( .BOTH. , #8377 ) ;
#15021 = VERTEX_POINT ( 'NONE', #2736 ) ;
#15022 = DIRECTION ( 'NONE',  ( 0.000000000000000000, 0.000000000000000000, -1.000000000000000000 ) ) ;
#15023 = CARTESIAN_POINT ( 'NONE',  ( -7.999999999994412470, -117.3221216070908355, 13.04594386772275527 ) ) ;
#15024 = EDGE_CURVE ( 'NONE', #5868, #27894, #11952, .T. ) ;
#15025 = VERTEX_POINT ( 'NONE', #14859 ) ;
#15026 = CARTESIAN_POINT ( 'NONE',  ( -0.6320852424383932577, 6.069672320066970883, -25.88903409330001182 ) ) ;
#15027 = CYLINDRICAL_SURFACE ( 'NONE', #866, 3.000000000000000444 ) ;
#15028 = ADVANCED_FACE ( 'NONE', ( #12333 ), #549, .F. ) ;
#15029 = EDGE_CURVE ( 'NONE', #28198, #19001, #4797, .T. ) ;
#15030 = CARTESIAN_POINT ( 'NONE',  ( -0.9769741165347872736, -4.003510540716011867, -67.93704710652500012 ) ) ;
#15031 = LINE ( 'NONE', #24624, #18554 ) ;
#15032 = CARTESIAN_POINT ( 'NONE',  ( -15.86808677770000209, -9.527368092500001495, -1.399999999599998990 ) ) ;
#15033 = ORIENTED_EDGE ( 'NONE', *, *, #8063, .T. ) ;
#15034 = UNCERTAINTY_MEASURE_WITH_UNIT (LENGTH_MEASURE( 1.000000000000000082E-05 ), #5971, 'distance_accuracy_value', 'NONE');
#15035 = ADVANCED_FACE ( 'NONE', ( #11815 ), #8427, .T. ) ;
#15036 = CARTESIAN_POINT ( 'NONE',  ( 4.440892098500000496E-16, -0.1455297029551360921, -71.05965357398815740 ) ) ;
#15037 = CIRCLE ( 'NONE', #1477, 10.00000000000000355 ) ;
#15038 = CARTESIAN_POINT ( 'NONE',  ( -17.37426278432861082, -22.00023419291344240, -26.95111891605012744 ) ) ;
#15039 = ORIENTED_EDGE ( 'NONE', *, *, #27687, .T. ) ;
#15040 = DIRECTION ( 'NONE',  ( 0.000000000000000000, -0.3420201433259318913, 0.9396926207858126157 ) ) ;
#15041 = LINE ( 'NONE', #5430, #1737 ) ;
#15042 = CARTESIAN_POINT ( 'NONE',  ( -23.94466870085087606, -15.45669659436210175, 5.680691770000024121 ) ) ;
#15043 = CARTESIAN_POINT ( 'NONE',  ( -5.304254813150000639E-10, 4.380584783799999468E-10, 230.0000000000000000 ) ) ;
#15044 = CARTESIAN_POINT ( 'NONE',  ( -8.751033796364147577, -8.359833048263213939, 232.0000000000046043 ) ) ;
#15045 = DIRECTION ( 'NONE',  ( 0.000000000000000000, 0.000000000000000000, -1.000000000000000000 ) ) ;
#15046 = CARTESIAN_POINT ( 'NONE',  ( 0.7846218181574846628, -3.768377790190448717, -0.6999999999999992895 ) ) ;
#15047 = EDGE_CURVE ( 'NONE', #10599, #5374, #21108, .T. ) ;
#15048 = CARTESIAN_POINT ( 'NONE',  ( -28.21939423762516341, -7.943967920865026677, 0.2374258030000131470 ) ) ;
#15049 = CARTESIAN_POINT ( 'NONE',  ( 10.69999999999999929, -30.00000000000000000, -28.40000000000000213 ) ) ;
#15050 = DIRECTION ( 'NONE',  ( 0.000000000000000000, 1.000000000000000000, 0.000000000000000000 ) ) ;
#15051 = LINE ( 'NONE', #12675, #14122 ) ;
#15052 = CARTESIAN_POINT ( 'NONE',  ( -3.931979172340965611, -26.51120696000498356, 20.25730302972669605 ) ) ;
#15053 = CARTESIAN_POINT ( 'NONE',  ( 0.4368970292312223669, -27.79681690464256150, 6.098651241000007772 ) ) ;
#15054 = ORIENTED_EDGE ( 'NONE', *, *, #353, .F. ) ;
#15055 = ADVANCED_FACE ( 'NONE', ( #21259 ), #12464, .T. ) ;
#15056 = CARTESIAN_POINT ( 'NONE',  ( 10.79767714369999965, -24.52928866599999935, -0.9448357716000042039 ) ) ;
#15057 = CARTESIAN_POINT ( 'NONE',  ( 25.08428924680000094, -13.52916357279999993, 225.7601281139999969 ) ) ;
#15058 = CARTESIAN_POINT ( 'NONE',  ( -3.112296099710462727, 3.758517760630103233, -62.99933298492499034 ) ) ;
#15059 = ORIENTED_EDGE ( 'NONE', *, *, #13051, .F. ) ;
#15060 = ORIENTED_EDGE ( 'NONE', *, *, #29764, .T. ) ;
#15061 = CARTESIAN_POINT ( 'NONE',  ( 27.42619050773425826, -9.513793714290953218, 0.08279779300002232389 ) ) ;
#15062 = ORIENTED_EDGE ( 'NONE', *, *, #18153, .T. ) ;
#15063 = EDGE_LOOP ( 'NONE', ( #11375, #9214, #15702, #1283 ) ) ;
#15064 = CARTESIAN_POINT ( 'NONE',  ( -3.971746973078826848, 0.6114051921346451701, -41.11517722957051291 ) ) ;
#15065 = FACE_OUTER_BOUND ( 'NONE', #21897, .T. ) ;
#15066 = CARTESIAN_POINT ( 'NONE',  ( 18.13191322229999969, -9.527368092500001495, -1.399999999599998990 ) ) ;
#15067 = UNCERTAINTY_MEASURE_WITH_UNIT (LENGTH_MEASURE( 1.000000000000000082E-05 ), #19091, 'distance_accuracy_value', 'NONE');
#15068 = CARTESIAN_POINT ( 'NONE',  ( 12.06519527120000035, 0.2459946332740000075, 231.9999991140000191 ) ) ;
#15069 = CARTESIAN_POINT ( 'NONE',  ( 10.69999999996760742, -29.99999999999999645, -28.04933239862057803 ) ) ;
#15070 = CARTESIAN_POINT ( 'NONE',  ( 28.45771199730000234, -1.776356839399999922E-14, 229.4982322489999831 ) ) ;
#15071 = ORIENTED_EDGE ( 'NONE', *, *, #8085, .T. ) ;
#15072 = CARTESIAN_POINT ( 'NONE',  ( 2.128921717830389859, -4.360192604088349633, -44.10000000002499831 ) ) ;
#15073 = CARTESIAN_POINT ( 'NONE',  ( -24.66346748855670867, -14.28208995890320665, 3.997248602000014195 ) ) ;
#15074 = CARTESIAN_POINT ( 'NONE',  ( -5.151963982244392781, -3.152247574024123811, -22.50799200640000919 ) ) ;
#15075 = DIRECTION ( 'NONE',  ( -3.582203977874193828E-13, -0.9128796883888956604, 0.4082287037029523336 ) ) ;
#15076 = CARTESIAN_POINT ( 'NONE',  ( -16.26205251953807007, 10.04907227120676261, -4.336808689942017243E-16 ) ) ;
#15077 = ADVANCED_FACE ( 'NONE', ( #16070 ), #2225, .F. ) ;
#15078 = CYLINDRICAL_SURFACE ( 'NONE', #6604, 2.000000000000000000 ) ;
#15079 = CARTESIAN_POINT ( 'NONE',  ( 1.638687372170418932, -21.15936910096317902, -28.82795821780189272 ) ) ;
#15080 = CARTESIAN_POINT ( 'NONE',  ( -4.251243323665415907, -4.132078999800212316, -46.72083066912499305 ) ) ;
#15081 = EDGE_CURVE ( 'NONE', #13864, #25831, #13457, .T. ) ;
#15082 = FACE_OUTER_BOUND ( 'NONE', #30774, .T. ) ;
#15083 = EDGE_CURVE ( 'NONE', #18133, #2248, #23477, .T. ) ;
#15084 = CARTESIAN_POINT ( 'NONE',  ( -1.057731049208300078, 1.834980888704576207, 226.6412452697800575 ) ) ;
#15085 = PLANE ( 'NONE',  #6751 ) ;
#15086 = CARTESIAN_POINT ( 'NONE',  ( -26.94142135619999934, -1.741760412339999700E-13, 230.0000000000000000 ) ) ;
#15087 = EDGE_CURVE ( 'NONE', #15510, #1011, #26691, .T. ) ;
#15088 = CARTESIAN_POINT ( 'NONE',  ( -16.81341597763548990, -10.09981795544978311, -0.6999999999999784173 ) ) ;
#15089 = ORIENTED_EDGE ( 'NONE', *, *, #11278, .F. ) ;
#15090 = AXIS2_PLACEMENT_3D ( 'NONE', #1093, #8311, #17906 ) ;
#15091 = CARTESIAN_POINT ( 'NONE',  ( -2.705882613314523955, 5.963358562559473164, -31.72635571290000200 ) ) ;
#15092 = VERTEX_POINT ( 'NONE', #25985 ) ;
#15093 = CARTESIAN_POINT ( 'NONE',  ( -10.00000000007662138, -32.32189936806710762, -22.79484972449596469 ) ) ;
#15094 = CARTESIAN_POINT ( 'NONE',  ( 5.782578939028539367, 2.564649547393091478, -51.87998794302499306 ) ) ;
#15095 = ORIENTED_EDGE ( 'NONE', *, *, #21187, .T. ) ;
#15096 = ORIENTED_EDGE ( 'NONE', *, *, #1620, .T. ) ;
#15097 = SHAPE_DEFINITION_REPRESENTATION ( #8888, #527 ) ;
#15098 = B_SPLINE_CURVE_WITH_KNOTS ( 'NONE', 3,
 ( #1070, #13487, #8762, #23103, #21049, #4052, #1544, #1850, #25928, #15685 ),
 .UNSPECIFIED., .F., .F.,
 ( 4, 2, 2, 2, 4 ),
 ( 0.000000000000000000, 0.2500000000000000000, 0.5000000000000001110, 0.7500000000000001110, 1.000000000000000000 ),
 .UNSPECIFIED. ) ;
#15099 = ORIENTED_EDGE ( 'NONE', *, *, #17484, .F. ) ;
#15100 = ORIENTED_EDGE ( 'NONE', *, *, #30446, .F. ) ;
#15101 = VECTOR ( 'NONE', #24505, 1000.000000000000000 ) ;
#15102 = CARTESIAN_POINT ( 'NONE',  ( 18.95046173579999760, -18.95046173579999760, 230.0000000000000000 ) ) ;
#15103 = CARTESIAN_POINT ( 'NONE',  ( -26.80000000069999899, 3.281945028329999726E-15, 115.0000000010000036 ) ) ;
#15104 = CARTESIAN_POINT ( 'NONE',  ( 9.999999999966957986, -29.70271642751552221, -27.05243720740120139 ) ) ;
#15105 = CARTESIAN_POINT ( 'NONE',  ( 2.716715618103660024, 4.270696308027718047, -35.69999999999998863 ) ) ;
#15106 = CARTESIAN_POINT ( 'NONE',  ( -12.40457278470585756, -30.63479341678588952, -24.72529260430050257 ) ) ;
#15107 = CARTESIAN_POINT ( 'NONE',  ( -4.345470169637781765, 2.035989658359887766, -0.6999999999999991784 ) ) ;
#15108 = CARTESIAN_POINT ( 'NONE',  ( 7.638687372236854678, -7.019901686315971112, -34.05533435017771637 ) ) ;
#15109 = LINE ( 'NONE', #17003, #25040 ) ;
#15110 = CARTESIAN_POINT ( 'NONE',  ( -16.06988921239048551, -8.208160914692745891, -0.6999999999999784173 ) ) ;
#15111 = CARTESIAN_POINT ( 'NONE',  ( 2.536150288113629081, -3.576595042060319862, -12.62388893670000023 ) ) ;
#15112 = CARTESIAN_POINT ( 'NONE',  ( -4.274658871253808279, -0.8336587121505223408, -30.59652066319999975 ) ) ;
#15113 = CARTESIAN_POINT ( 'NONE',  ( 24.74993095452947856, -14.13250376044891965, 6.042507811999997536 ) ) ;
#15114 = CARTESIAN_POINT ( 'NONE',  ( 18.80717682333433061, 19.99999822827082241, -0.5856167109999921294 ) ) ;
#15115 = CARTESIAN_POINT ( 'NONE',  ( 28.68577476838161644, -9.950727360109466346, 8.000000000000007105 ) ) ;
#15116 = CARTESIAN_POINT ( 'NONE',  ( 28.53960566377543984, -1.916108254339756067, 8.000000000000007105 ) ) ;
#15117 = CARTESIAN_POINT ( 'NONE',  ( 2.022420680230021972, -3.847796821814266632, -33.20721934060000535 ) ) ;
#15118 = DIRECTION ( 'NONE',  ( -3.582203977874193828E-13, -0.9128796883888956604, 0.4082287037029523336 ) ) ;
#15119 = CARTESIAN_POINT ( 'NONE',  ( 14.76986634514344310, -25.51951968493025902, -23.48139095529251463 ) ) ;
#15120 = CARTESIAN_POINT ( 'NONE',  ( 1.015231355539999880, -28.48218680760000154, 224.4935313260000100 ) ) ;
#15121 = EDGE_CURVE ( 'NONE', #7509, #27320, #21422, .T. ) ;
#15122 = ORIENTED_EDGE ( 'NONE', *, *, #23460, .F. ) ;
#15123 = DIRECTION ( 'NONE',  ( 0.000000000000000000, -1.000000000000000000, 2.257145581549999994E-12 ) ) ;
#15124 = DIRECTION ( 'NONE',  ( 0.000000000000000000, 0.000000000000000000, 1.000000000000000000 ) ) ;
#15125 = ORIENTED_EDGE ( 'NONE', *, *, #26362, .T. ) ;
#15126 = DIRECTION ( 'NONE',  ( 0.000000000000000000, 1.000000000000000000, 0.000000000000000000 ) ) ;
#15127 = CARTESIAN_POINT ( 'NONE',  ( -3.552713678799999608E-15, -3.552713678799999608E-15, 143.2171415880000040 ) ) ;
#15128 = ORIENTED_EDGE ( 'NONE', *, *, #6995, .F. ) ;
#15129 = CARTESIAN_POINT ( 'NONE',  ( -4.766028791791773855, -1.519250813530571564, -44.10000000002499121 ) ) ;
#15130 = ORIENTED_EDGE ( 'NONE', *, *, #5558, .F. ) ;
#15131 = EDGE_LOOP ( 'NONE', ( #25939, #11460, #27179 ) ) ;
#15132 = ORIENTED_EDGE ( 'NONE', *, *, #12377, .F. ) ;
#15133 = PLANE ( 'NONE',  #10449 ) ;
#15134 = CARTESIAN_POINT ( 'NONE',  ( -16.70716219638308075, 12.10247952391986281, -0.6999999999999784173 ) ) ;
#15135 = EDGE_CURVE ( 'NONE', #18136, #11286, #20948, .T. ) ;
#15136 = CARTESIAN_POINT ( 'NONE',  ( 16.19686700681432256, -8.461754693832318708, -0.6999999999999785283 ) ) ;
#15137 = EDGE_LOOP ( 'NONE', ( #10379, #1314, #6303, #26214 ) ) ;
#15138 = CARTESIAN_POINT ( 'NONE',  ( -19.80526803560000104, 19.50877411510000314, 228.5999999999999943 ) ) ;
#15139 = CARTESIAN_POINT ( 'NONE',  ( 0.4831567132655384955, -28.49614615030703391, 6.099998581000020792 ) ) ;
#15140 = CARTESIAN_POINT ( 'NONE',  ( -11.83960380747999963, -20.99999999999999645, -28.40000000000771863 ) ) ;
#15141 = LINE ( 'NONE', #22392, #13490 ) ;
#15142 = ORIENTED_EDGE ( 'NONE', *, *, #10080, .T. ) ;
#15143 = EDGE_CURVE ( 'NONE', #27949, #12805, #9963, .T. ) ;
#15144 = CIRCLE ( 'NONE', #15632, 4.000000000000001776 ) ;
#15145 = DIRECTION ( 'NONE',  ( 1.000000000000000000, 0.000000000000000000, 0.000000000000000000 ) ) ;
#15146 = CARTESIAN_POINT ( 'NONE',  ( 2.949882002856674124, 3.605460750137338799, -20.25622222230000347 ) ) ;
#15147 = CARTESIAN_POINT ( 'NONE',  ( -20.19076655603532799, -17.71015691556360494, 193.2171415880000040 ) ) ;
#15148 = CARTESIAN_POINT ( 'NONE',  ( -0.6812178144568332705, -27.49175526154860805, 5.876143015413799908 ) ) ;
#15149 = CARTESIAN_POINT ( 'NONE',  ( 23.36339467975494344, -14.50559736754933837, 225.6749683488453400 ) ) ;
#15150 = CARTESIAN_POINT ( 'NONE',  ( -27.04041630560000087, -5.416379761039999262E-14, 230.6999999999999886 ) ) ;
#15151 = LINE ( 'NONE', #20334, #8748 ) ;
#15152 = CARTESIAN_POINT ( 'NONE',  ( -3.254826447623020425, 1.366018022090351280, -0.6999999999999783062 ) ) ;
#15153 = CARTESIAN_POINT ( 'NONE',  ( 23.93626153989999850, 13.29299652659999964, 230.0000000000000000 ) ) ;
#15154 = CARTESIAN_POINT ( 'NONE',  ( 5.571346931303373218, -7.726481253986936082, -33.71071246860980608 ) ) ;
#15155 = ORIENTED_EDGE ( 'NONE', *, *, #28364, .T. ) ;
#15156 = CARTESIAN_POINT ( 'NONE',  ( -0.05052225346893526176, 4.317558364482406930, -56.91818518972499419 ) ) ;
#15157 = CARTESIAN_POINT ( 'NONE',  ( -12.41036288878599336, -25.66802163662577385, -23.39552330665722479 ) ) ;
#15158 = CARTESIAN_POINT ( 'NONE',  ( -22.06913545123989806, 17.56725181269473524, 0.8585790010000038386 ) ) ;
#15159 = CARTESIAN_POINT ( 'NONE',  ( -4.680684891358993127, 0.7214394727549908737, -68.10000000002501963 ) ) ;
#15160 = EDGE_CURVE ( 'NONE', #22213, #29409, #4574, .T. ) ;
#15161 = VERTEX_POINT ( 'NONE', #31011 ) ;
#15162 = ORIENTED_EDGE ( 'NONE', *, *, #24774, .T. ) ;
#15163 = CARTESIAN_POINT ( 'NONE',  ( 0.5564057544863512117, 3.564787113782302619, -88.52261276243972077 ) ) ;
#15164 = AXIS2_PLACEMENT_3D ( 'NONE', #17916, #22814, #15266 ) ;
#15165 = ORIENTED_EDGE ( 'NONE', *, *, #7689, .T. ) ;
#15166 = CARTESIAN_POINT ( 'NONE',  ( -10.69999999999999929, -25.00000000000000000, -26.16393202249999916 ) ) ;
#15167 = LINE ( 'NONE', #15481, #19023 ) ;
#15168 = ORIENTED_EDGE ( 'NONE', *, *, #713, .T. ) ;
#15169 = CARTESIAN_POINT ( 'NONE',  ( -5.427432314178970429, 2.515719109140460041, -65.29526299442500203 ) ) ;
#15170 = CARTESIAN_POINT ( 'NONE',  ( -22.39560851969999788, -19.79663304750000208, 230.0000000000000000 ) ) ;
#15171 = CARTESIAN_POINT ( 'NONE',  ( -28.35455043824866550, -0.5159221438580332553, 0.2374258030000131470 ) ) ;
#15172 = CARTESIAN_POINT ( 'NONE',  ( 0.000000000000000000, 0.000000000000000000, 40.00000000000000000 ) ) ;
#15173 = DIRECTION ( 'NONE',  ( 0.000000000000000000, 1.000000000000000000, 0.000000000000000000 ) ) ;
#15174 = EDGE_CURVE ( 'NONE', #4659, #11492, #19995, .T. ) ;
#15175 = LINE ( 'NONE', #24780, #10227 ) ;
#15176 = VERTEX_POINT ( 'NONE', #30552 ) ;
#15177 = CARTESIAN_POINT ( 'NONE',  ( -26.84464183080000055, 3.287411895199999866E-15, 42.56249624490000372 ) ) ;
#15178 =( GEOMETRIC_REPRESENTATION_CONTEXT ( 3 ) GLOBAL_UNCERTAINTY_ASSIGNED_CONTEXT ( ( #21037 ) ) GLOBAL_UNIT_ASSIGNED_CONTEXT ( ( #11774, #23906, #16797 ) ) REPRESENTATION_CONTEXT ( 'NONE', 'WORKASPACE' ) );
#15179 = CARTESIAN_POINT ( 'NONE',  ( 14.68395928812360651, -31.04325972095271169, -31.83912560350277943 ) ) ;
#15180 = AXIS2_PLACEMENT_3D ( 'NONE', #27147, #15040, #267 ) ;
#15181 = VERTEX_POINT ( 'NONE', #7092 ) ;
#15182 = CARTESIAN_POINT ( 'NONE',  ( -15.73099012567143618, 10.87604578374266673, -1.384526174263989162E-13 ) ) ;
#15183 = CARTESIAN_POINT ( 'NONE',  ( -24.92639508767336309, -13.81781708088548122, 5.506973469000003618 ) ) ;
#15184 = CARTESIAN_POINT ( 'NONE',  ( -24.41841039498785193, -14.69667350221323865, 6.099998581000020792 ) ) ;
#15185 = CARTESIAN_POINT ( 'NONE',  ( 24.05832192679999793, -13.92979812329999945, 223.9000014189999774 ) ) ;
#15186 = DIRECTION ( 'NONE',  ( 0.000000000000000000, -0.9128796883888953273, 0.4082287037029528332 ) ) ;
#15187 = PRODUCT_DEFINITION_SHAPE ( 'NONE', 'NONE',  #31124 ) ;
#15188 = CARTESIAN_POINT ( 'NONE',  ( -1.804682441769323464, -3.297106965646906751, -0.6999999999999991784 ) ) ;
#15189 = CARTESIAN_POINT ( 'NONE',  ( -20.74517834863038601, -21.65192390581155379, 0.5017677510000262409 ) ) ;
#15190 = CARTESIAN_POINT ( 'NONE',  ( -9.414213562409999625, -15.31419272936388687, -74.45223986426802298 ) ) ;
#15191 = EDGE_CURVE ( 'NONE', #24060, #11184, #14344, .T. ) ;
#15192 =( NAMED_UNIT ( * ) PLANE_ANGLE_UNIT ( ) SI_UNIT ( $, .RADIAN. ) );
#15193 = DIRECTION ( 'NONE',  ( -1.000000000000000000, 1.224606353819999829E-16, 0.000000000000000000 ) ) ;
#15194 = ADVANCED_FACE ( 'NONE', ( #24 ), #19205, .F. ) ;
#15195 = CARTESIAN_POINT ( 'NONE',  ( -4.679341198149895575, -26.38945575071663896, 20.49029498623629664 ) ) ;
#15196 = CARTESIAN_POINT ( 'NONE',  ( 0.4713258872163371693, -27.79624559782060800, 6.099998581000020792 ) ) ;
#15197 = AXIS2_PLACEMENT_3D ( 'NONE', #19193, #21561, #5599 ) ;
#15198 = EDGE_LOOP ( 'NONE', ( #19102, #9412, #6101, #19016 ) ) ;
#15199 = LINE ( 'NONE', #8410, #9743 ) ;
#15200 = ADVANCED_FACE ( 'NONE', ( #2529 ), #19366, .F. ) ;
#15201 = CARTESIAN_POINT ( 'NONE',  ( 9.999999999979998222, -127.2537437101000108, -34.36317024011000143 ) ) ;
#15202 = CARTESIAN_POINT ( 'NONE',  ( 16.20123158649999695, 11.52736809289999620, -0.6999999999999992895 ) ) ;
#15203 = CIRCLE ( 'NONE', #13707, 26.80000000000000071 ) ;
#15204 = CARTESIAN_POINT ( 'NONE',  ( 0.8372177269581546621, 4.490875019823945991, -63.42744533512499316 ) ) ;
#15205 = ORIENTED_EDGE ( 'NONE', *, *, #17928, .F. ) ;
#15206 = ORIENTED_EDGE ( 'NONE', *, *, #16603, .F. ) ;
#15208 = EDGE_CURVE ( 'NONE', #30391, #5518, #8248, .T. ) ;
#15207 = CARTESIAN_POINT ( 'NONE',  ( 22.75205003212621335, -19.38592737840143343, 0.000000000000000000 ) ) ;
#15209 = VERTEX_POINT ( 'NONE', #24698 ) ;
#15210 = EDGE_LOOP ( 'NONE', ( #7165, #25752, #14285, #13703 ) ) ;
#15211 = CARTESIAN_POINT ( 'NONE',  ( 9.999999999979998222, -27.00000000000000000, -31.39999999999999858 ) ) ;
#15212 = CARTESIAN_POINT ( 'NONE',  ( 25.05552768372066907, -13.58331698798256504, 3.920132093000017193 ) ) ;
#15213 = CARTESIAN_POINT ( 'NONE',  ( -25.11462376325593837, -13.47330140865266834, 224.3201053094227859 ) ) ;
#15214 = CARTESIAN_POINT ( 'NONE',  ( 8.700000000284079604, -17.26910668097993096, -37.68099296457697278 ) ) ;
#15215 =( REPRESENTATION_RELATIONSHIP ('NONE','NONE', #2712, #30659 ) REPRESENTATION_RELATIONSHIP_WITH_TRANSFORMATION ( #9562 )SHAPE_REPRESENTATION_RELATIONSHIP( ) );
#15216 = CARTESIAN_POINT ( 'NONE',  ( 24.97129468909112404, -13.73710443560444183, 6.098655031999994591 ) ) ;
#15217 = DIRECTION ( 'NONE',  ( -0.6941258031311203780, -0.7198537139083029945, 0.000000000000000000 ) ) ;
#15218 = ORIENTED_EDGE ( 'NONE', *, *, #14963, .T. ) ;
#15219 = CARTESIAN_POINT ( 'NONE',  ( 1.988743700875508891, -3.677409591406694211, -44.10000000002499121 ) ) ;
#15220 = CARTESIAN_POINT ( 'NONE',  ( 16.06675444873834380, 10.97998838177521286, -0.6999999999999784173 ) ) ;
#15221 = EDGE_CURVE ( 'NONE', #23236, #28202, #26538, .T. ) ;
#15222 = CARTESIAN_POINT ( 'NONE',  ( -5.151963982244392781, -3.152247574024123811, -21.90799200640000777 ) ) ;
#15223 = CARTESIAN_POINT ( 'NONE',  ( -12.46077600683748265, -25.93302859383775427, -33.55712785976603385 ) ) ;
#15224 = CARTESIAN_POINT ( 'NONE',  ( -6.661312627754256255, -8.560122214784900763, -36.64192442629084212 ) ) ;
#15225 = CIRCLE ( 'NONE', #28300, 2.000000000010000889 ) ;
#15226 = CARTESIAN_POINT ( 'NONE',  ( 26.80000000000001492, -1.754055898254314183, 86.78285841095834030 ) ) ;
#15227 = CARTESIAN_POINT ( 'NONE',  ( 6.000000000000000000, -15.18061163548115466, -76.53197586718597734 ) ) ;
#15228 = CARTESIAN_POINT ( 'NONE',  ( -4.251243323665415907, -4.132078999800212316, -47.20083066912499703 ) ) ;
#15229 = CARTESIAN_POINT ( 'NONE',  ( -16.43242232095159139, 12.03437313996399105, -1.400000000000002132 ) ) ;
#15230 = CARTESIAN_POINT ( 'NONE',  ( 7.121574564636415694, -25.83919502053028339, 208.0635107809515318 ) ) ;
#15231 = CARTESIAN_POINT ( 'NONE',  ( -8.699999998953916958, -16.84112679184576677, -33.19732076807623145 ) ) ;
#15232 = CARTESIAN_POINT ( 'NONE',  ( -27.53132593009999951, -1.221715529480000030E-11, 229.7313259299999686 ) ) ;
#15233 = CARTESIAN_POINT ( 'NONE',  ( -17.59696597926837214, -9.791839085300418688, -0.6999999999999784173 ) ) ;
#15234 = ORIENTED_EDGE ( 'NONE', *, *, #22900, .F. ) ;
#15235 = CARTESIAN_POINT ( 'NONE',  ( -3.850850186879767545, -3.402327863231305205, -34.77197003409999354 ) ) ;
#15236 = ORIENTED_EDGE ( 'NONE', *, *, #26394, .T. ) ;
#15237 = DIRECTION ( 'NONE',  ( 1.553791817432423893E-12, -0.7253743710120292842, 0.6883545756940262494 ) ) ;
#15238 = CARTESIAN_POINT ( 'NONE',  ( 4.416651415012724513, -2.079980245798425109, -53.04872167392500870 ) ) ;
#15239 = ORIENTED_EDGE ( 'NONE', *, *, #7753, .T. ) ;
#15240 = CONICAL_SURFACE ( 'NONE', #19789, 4.997501249379996402, 1.047197551199999799 ) ;
#15241 = ORIENTED_EDGE ( 'NONE', *, *, #30426, .F. ) ;
#15242 = DIRECTION ( 'NONE',  ( 0.1508756461098751389, -5.572891941358692673E-17, -0.9885527499384785255 ) ) ;
#15243 = VECTOR ( 'NONE', #13066, 1000.000000000000000 ) ;
#15244 = VERTEX_POINT ( 'NONE', #9920 ) ;
#15245 = ADVANCED_FACE ( 'NONE', ( #7553 ), #19673, .F. ) ;
#15246 = ORIENTED_EDGE ( 'NONE', *, *, #20014, .T. ) ;
#15247 = DIRECTION ( 'NONE',  ( -1.000000000000000000, 5.063197467948052462E-16, -2.257212216284997029E-12 ) ) ;
#15248 = DIRECTION ( 'NONE',  ( 0.7071067811865466846, 1.595945597898659700E-12, 0.7071067811865484609 ) ) ;
#15249 = CARTESIAN_POINT ( 'NONE',  ( 3.835128050359830176, 3.444395927274146452, -35.69999999999999574 ) ) ;
#15250 = ADVANCED_FACE ( 'NONE', ( #27058, #29256 ), #2832, .F. ) ;
#15251 = FACE_OUTER_BOUND ( 'NONE', #10340, .T. ) ;
#15252 = EDGE_CURVE ( 'NONE', #22030, #27419, #19520, .T. ) ;
#15253 = CARTESIAN_POINT ( 'NONE',  ( -12.44385388531385495, -28.14926872442419281, -23.29034717779581598 ) ) ;
#15254 = CARTESIAN_POINT ( 'NONE',  ( -3.893462112830481825, 1.255681637813407248, -0.6999999999999992895 ) ) ;
#15255 = CARTESIAN_POINT ( 'NONE',  ( 4.373195337096347224, -2.904765488536225515, 0.04124526979999709742 ) ) ;
#15256 = CARTESIAN_POINT ( 'NONE',  ( -27.76135144249999698, 3.399672736719999759E-15, 42.33858589270000294 ) ) ;
#15257 = CARTESIAN_POINT ( 'NONE',  ( -22.41290914069411500, 16.47772183393138690, 7.000000021000013284 ) ) ;
#15258 = VERTEX_POINT ( 'NONE', #2679 ) ;
#15259 = CARTESIAN_POINT ( 'NONE',  ( -1.657635364023947400, -6.345118362804027079, -12.55022317840000312 ) ) ;
#15260 = CARTESIAN_POINT ( 'NONE',  ( 1.602200344400662058, -4.514849430718075318, -29.31882401680000072 ) ) ;
#15261 = AXIS2_PLACEMENT_3D ( 'NONE', #27641, #28119, #25617 ) ;
#15262 = DIRECTION ( 'NONE',  ( 0.000000000000000000, 0.000000000000000000, -1.000000000000000000 ) ) ;
#15263 = CARTESIAN_POINT ( 'NONE',  ( -24.59348680947261556, -12.96247199543289241, 225.2894582296841861 ) ) ;
#15264 = CARTESIAN_POINT ( 'NONE',  ( -2.020725942269999909, -3.500000000000000000, 227.9588918784999976 ) ) ;
#15265 = AXIS2_PLACEMENT_3D ( 'NONE', #2051, #8966, #11797 ) ;
#15266 = DIRECTION ( 'NONE',  ( 0.000000000000000000, 1.000000000000000000, 0.000000000000000000 ) ) ;
#15267 = CARTESIAN_POINT ( 'NONE',  ( 9.499999999770000869, 21.70000000000000284, -60.10000000000000142 ) ) ;
#15268 = VECTOR ( 'NONE', #20125, 999.9999999999998863 ) ;
#15269 = VECTOR ( 'NONE', #19365, 1000.000000000000114 ) ;
#15271 = CARTESIAN_POINT ( 'NONE',  ( 19.80538173989999962, 19.50875420239999869, 226.9999998930000231 ) ) ;
#15270 = B_SPLINE_CURVE_WITH_KNOTS ( 'NONE', 3,
 ( #14627, #7071, #24216, #7226, #2658, #2815 ),
 .UNSPECIFIED., .F., .F.,
 ( 4, 2, 4 ),
 ( 0.000000000000000000, 0.5000000000000000000, 1.000000000000000000 ),
 .UNSPECIFIED. ) ;
#15272 = LINE ( 'NONE', #6131, #27820 ) ;
#15273 = DIRECTION ( 'NONE',  ( 0.000000000000000000, 0.000000000000000000, 1.000000000000000000 ) ) ;
#15274 = EDGE_LOOP ( 'NONE', ( #19472, #6345, #13254, #13560 ) ) ;
#15275 = CARTESIAN_POINT ( 'NONE',  ( -7.999999999723122812, -24.55065533306149916, -26.62378963206735349 ) ) ;
#15276 = DIRECTION ( 'NONE',  ( 1.000000000000000000, 0.000000000000000000, 0.000000000000000000 ) ) ;
#15277 = ORIENTED_EDGE ( 'NONE', *, *, #1552, .F. ) ;
#15278 = DIRECTION ( 'NONE',  ( 2.848302087110504847E-12, 0.8902635789277789646, -0.4554456718805243165 ) ) ;
#15279 = CARTESIAN_POINT ( 'NONE',  ( 4.960227444650000095, 16.90556345610000122, 230.0904314459999966 ) ) ;
#15280 = ORIENTED_EDGE ( 'NONE', *, *, #11250, .F. ) ;
#15281 = CARTESIAN_POINT ( 'NONE',  ( -0.5612696204402340960, -26.79446732153163424, 4.042548093418004029 ) ) ;
#15282 = ORIENTED_EDGE ( 'NONE', *, *, #2021, .F. ) ;
#15283 = ORIENTED_EDGE ( 'NONE', *, *, #21680, .F. ) ;
#15284 = SURFACE_SIDE_STYLE ('',( #10416 ) ) ;
#15285 = VERTEX_POINT ( 'NONE', #3133 ) ;
#15286 = DIRECTION ( 'NONE',  ( 0.000000000000000000, 0.000000000000000000, -1.000000000000000000 ) ) ;
#15287 = CARTESIAN_POINT ( 'NONE',  ( 8.700000000248291343, -24.65319937758141222, -30.30964379061154190 ) ) ;
#15289 = CARTESIAN_POINT ( 'NONE',  ( -24.83827471527357744, 12.48687850854618198, 4.999998581000003384 ) ) ;
#15288 = CIRCLE ( 'NONE', #19318, 1.100000000390000787 ) ;
#15290 = AXIS2_PLACEMENT_3D ( 'NONE', #24424, #2859, #29598 ) ;
#15291 = ORIENTED_EDGE ( 'NONE', *, *, #1666, .T. ) ;
#15292 = DIRECTION ( 'NONE',  ( 0.000000000000000000, 0.000000000000000000, -1.000000000000000000 ) ) ;
#15293 = AXIS2_PLACEMENT_3D ( 'NONE', #13801, #28268, #27962 ) ;
#15294 = EDGE_CURVE ( 'NONE', #26555, #24268, #29106, .T. ) ;
#15295 = CIRCLE ( 'NONE', #29839, 27.23548387100000312 ) ;
#15296 = CARTESIAN_POINT ( 'NONE',  ( -12.29999999969274072, -32.29251981524999593, -29.47202332494083521 ) ) ;
#15297 = ADVANCED_FACE ( 'NONE', ( #28790, #26748 ), #17159, .T. ) ;
#15298 = DIRECTION ( 'NONE',  ( 1.000000000000000000, 0.000000000000000000, 0.000000000000000000 ) ) ;
#15299 = CARTESIAN_POINT ( 'NONE',  ( -19.80535357367646654, 19.50875577052770993, 1.400000021000019634 ) ) ;
#15300 = VERTEX_POINT ( 'NONE', #22185 ) ;
#15301 = CARTESIAN_POINT ( 'NONE',  ( 2.914708617673698932, -3.631324690002109445, -3.105321867099997135 ) ) ;
#15302 = CARTESIAN_POINT ( 'NONE',  ( 5.503465972402116435, -2.627571514392686769, -20.28180150030001272 ) ) ;
#15303 = DIRECTION ( 'NONE',  ( 0.3633921898465289901, 0.9316362575375348731, 1.301042606982604374E-14 ) ) ;
#15304 = PLANE ( 'NONE',  #5455 ) ;
#15305 = STYLED_ITEM ( 'NONE', ( #24768 ), #20057 ) ;
#15306 = CARTESIAN_POINT ( 'NONE',  ( 0.8402705472655720431, -5.127977335047565255, -93.44632962453067648 ) ) ;
#15307 = CARTESIAN_POINT ( 'NONE',  ( -25.46187654339999895, 14.12439703449999939, 229.0000000000000000 ) ) ;
#15308 = ORIENTED_EDGE ( 'NONE', *, *, #27518, .T. ) ;
#15309 = CARTESIAN_POINT ( 'NONE',  ( -24.50000001620000134, 3.000285568850000245E-15, 189.9999999960000139 ) ) ;
#15310 = CARTESIAN_POINT ( 'NONE',  ( 2.507604248379858625, 2.484315071469196390, -0.6999999999999784173 ) ) ;
#15311 = DIRECTION ( 'NONE',  ( -1.000000000000000000, 0.000000000000000000, 0.000000000000000000 ) ) ;
#15312 = CARTESIAN_POINT ( 'NONE',  ( -23.20948082139999968, -13.40000000000000036, 3.900000000369999942 ) ) ;
#15313 = VECTOR ( 'NONE', #10365, 1000.000000000000000 ) ;
#15314 = ORIENTED_EDGE ( 'NONE', *, *, #4217, .F. ) ;
#15315 = CARTESIAN_POINT ( 'NONE',  ( 0.8945918243927832858, -4.819150861182647461, -58.74125695792500323 ) ) ;
#15316 = CARTESIAN_POINT ( 'NONE',  ( -8.699999999669005391, -18.23122067931867107, -34.51216076567753532 ) ) ;
#15317 = AXIS2_PLACEMENT_3D ( 'NONE', #26850, #16937, #2169 ) ;
#15318 = CARTESIAN_POINT ( 'NONE',  ( -0.1000000000151932966, -15.94902145824367246, -35.53273252498938461 ) ) ;
#15319 = CARTESIAN_POINT ( 'NONE',  ( -26.10391306214228990, 8.822478663265938437, 0.000000000000000000 ) ) ;
#15320 = CARTESIAN_POINT ( 'NONE',  ( -4.222785574039375156, 0.7211312973832428863, -68.10000000002500542 ) ) ;
#15321 = EDGE_LOOP ( 'NONE', ( #26851, #17520, #7321, #5027, #15935 ) ) ;
#15322 = EDGE_CURVE ( 'NONE', #9489, #22831, #644, .T. ) ;
#15323 = EDGE_LOOP ( 'NONE', ( #26131, #25728, #3247, #28173 ) ) ;
#15324 = CARTESIAN_POINT ( 'NONE',  ( -0.02159632328769568732, -0.1383635851000819539, -98.24333933864600965 ) ) ;
#15325 = SURFACE_STYLE_FILL_AREA ( #20046 ) ;
#15326 = ORIENTED_EDGE ( 'NONE', *, *, #27343, .T. ) ;
#15327 = CARTESIAN_POINT ( 'NONE',  ( -12.12499970569999874, 20.99999999999999645, -55.73512393480000071 ) ) ;
#15328 = CIRCLE ( 'NONE', #10814, 26.80000000000000071 ) ;
#15329 = CARTESIAN_POINT ( 'NONE',  ( 23.25311087529421172, 15.23597699658644800, 5.310552110000033466 ) ) ;
#15330 = CARTESIAN_POINT ( 'NONE',  ( 5.885062339963589295, 0.1407603604956381704, -63.26686508972500178 ) ) ;
#15331 = CARTESIAN_POINT ( 'NONE',  ( 0.000000000000000000, 0.000000000000000000, 115.0000000000000000 ) ) ;
#15332 = B_SPLINE_CURVE_WITH_KNOTS ( 'NONE', 3,
 ( #22238, #14695, #695, #10282, #15149, #24750, #3186, #22397, #842, #10434 ),
 .UNSPECIFIED., .F., .F.,
 ( 4, 2, 2, 2, 4 ),
 ( 0.000000000000000000, 0.2500000000000000000, 0.5000000000000000000, 0.7500000000000000000, 1.000000000000000000 ),
 .UNSPECIFIED. ) ;
#15333 = CARTESIAN_POINT ( 'NONE',  ( -2.098441946322436635, -3.287561928151557122, -68.10000000002500542 ) ) ;
#15334 = CARTESIAN_POINT ( 'NONE',  ( -24.93720648713954446, 13.79881813474513486, 3.899998581000013509 ) ) ;
#15335 = CARTESIAN_POINT ( 'NONE',  ( 11.08346179031908818, -28.41490585489483323, 43.60555127550001231 ) ) ;
#15336 = DIRECTION ( 'NONE',  ( 0.000000000000000000, -1.000000000000000000, 0.000000000000000000 ) ) ;
#15337 = ORIENTED_EDGE ( 'NONE', *, *, #23865, .T. ) ;
#15338 = UNCERTAINTY_MEASURE_WITH_UNIT (LENGTH_MEASURE( 1.000000000000000082E-05 ), #16215, 'distance_accuracy_value', 'NONE');
#15339 = CARTESIAN_POINT ( 'NONE',  ( 0.6805609921852766586, -26.79155681362076180, 5.876648811199404854 ) ) ;
#15340 = CARTESIAN_POINT ( 'NONE',  ( -26.93395387809999875, 3.298349105260000080E-15, 92.24324102360000666 ) ) ;
#15341 = VERTEX_POINT ( 'NONE', #14648 ) ;
#15342 = CARTESIAN_POINT ( 'NONE',  ( 14.75111860151799270, -31.99974791380525474, -29.71106056348426705 ) ) ;
#15343 = CARTESIAN_POINT ( 'NONE',  ( 3.162069896769252431, -2.100311282821142100, -35.69999999999999574 ) ) ;
#15344 = CARTESIAN_POINT ( 'NONE',  ( -23.81866173682177390, -14.33570044646243247, 6.099998581000020792 ) ) ;
#15345 = DIRECTION ( 'NONE',  ( 0.000000000000000000, 0.000000000000000000, 1.000000000000000000 ) ) ;
#15346 = CARTESIAN_POINT ( 'NONE',  ( -23.36339468011815157, -14.50559736696343727, 4.325031650548394779 ) ) ;
#15347 = CARTESIAN_POINT ( 'NONE',  ( 0.2775905903481815651, -3.807106439044698920, -0.6999999999999991784 ) ) ;
#15348 = CARTESIAN_POINT ( 'NONE',  ( -19.53673505992006554, -20.39066108913833020, -0.6999999999999784173 ) ) ;
#15349 = CARTESIAN_POINT ( 'NONE',  ( -0.1000000000709524162, -18.04864474153813347, -34.59380650647258904 ) ) ;
#15350 = AXIS2_PLACEMENT_3D ( 'NONE', #18, #7391, #4727 ) ;
#15351 = ORIENTED_EDGE ( 'NONE', *, *, #27315, .T. ) ;
#15352 =( NAMED_UNIT ( * ) SI_UNIT ( $, .STERADIAN. ) SOLID_ANGLE_UNIT ( ) );
#15353 = DIRECTION ( 'NONE',  ( 0.000000000000000000, 0.000000000000000000, 1.000000000000000000 ) ) ;
#15354 = EDGE_CURVE ( 'NONE', #6694, #22920, #9775, .T. ) ;
#15355 = CARTESIAN_POINT ( 'NONE',  ( -7.662090775718862545, -25.68204763724676454, 22.48967911107480333 ) ) ;
#15356 = CARTESIAN_POINT ( 'NONE',  ( -0.4969045691271392617, -28.49594262166942116, 5.506468674000009500 ) ) ;
#15357 = B_SPLINE_CURVE_WITH_KNOTS ( 'NONE', 1,
 ( #21869, #28771 ),
 .UNSPECIFIED., .F., .F.,
 ( 2, 2 ),
 ( -2.556017480449999863E-06, 0.7000000000009999335 ),
 .UNSPECIFIED. ) ;
#15358 = ORIENTED_EDGE ( 'NONE', *, *, #25806, .F. ) ;
#15359 = EDGE_CURVE ( 'NONE', #23036, #26756, #10947, .T. ) ;
#15360 = CARTESIAN_POINT ( 'NONE',  ( -9.000000000229999131, 20.99999999999999645, -53.60000000000000142 ) ) ;
#15361 = CARTESIAN_POINT ( 'NONE',  ( -9.993285220779425160, -25.61999708228226069, 115.0000000000000000 ) ) ;
#15362 = DIRECTION ( 'NONE',  ( 0.7071067811898220645, -0.2886612846638017538, -0.6455034180634621199 ) ) ;
#15363 = CARTESIAN_POINT ( 'NONE',  ( 5.433585117924402574, 2.226379967917181180, -61.69141554682499873 ) ) ;
#15364 = ORIENTED_EDGE ( 'NONE', *, *, #19701, .T. ) ;
#15365 = ORIENTED_EDGE ( 'NONE', *, *, #1804, .T. ) ;
#15366 = CARTESIAN_POINT ( 'NONE',  ( 8.700000000286674862, -20.29216153631914210, -40.76320817051012568 ) ) ;
#15367 = VERTEX_POINT ( 'NONE', #8709 ) ;
#15368 = ADVANCED_FACE ( 'NONE', ( #1648 ), #28534, .F. ) ;
#15369 = CARTESIAN_POINT ( 'NONE',  ( -2.986077861064811767, 1.962750821053097949, -41.77427253121008022 ) ) ;
#15370 = CARTESIAN_POINT ( 'NONE',  ( -12.29999999986958414, -27.39269908169872281, -31.40000000020000570 ) ) ;
#15371 = CARTESIAN_POINT ( 'NONE',  ( -12.75378086759999796, -32.00000000000000000, -31.28675134614999820 ) ) ;
#15372 = DIRECTION ( 'NONE',  ( 1.000000000000000000, -1.953112501701599149E-12, 2.703609717165946368E-12 ) ) ;
#15373 = CARTESIAN_POINT ( 'NONE',  ( -14.94562240850000023, -8.628859120750000500, 225.0000000000000000 ) ) ;
#15374 = DIRECTION ( 'NONE',  ( -1.000000000000000000, -6.565028073413479156E-24, -2.257144471327815248E-12 ) ) ;
#15375 = EDGE_LOOP ( 'NONE', ( #16869, #11049, #22062, #15733 ) ) ;
#15376 = CARTESIAN_POINT ( 'NONE',  ( 1.851108483524190662, -3.721478854253624124, -44.10000000002499121 ) ) ;
#15377 = CARTESIAN_POINT ( 'NONE',  ( 27.79539923781684507, 0.5057481689249235801, 8.000000000000007105 ) ) ;
#15378 = CARTESIAN_POINT ( 'NONE',  ( 3.710789578725085303, 2.835545959904683500, -23.86727430110000370 ) ) ;
#15379 = CARTESIAN_POINT ( 'NONE',  ( 23.73450314244648496, -12.44732035365262313, 4.781948426524514240 ) ) ;
#15380 = FACE_OUTER_BOUND ( 'NONE', #4102, .T. ) ;
#15381 = FACE_OUTER_BOUND ( 'NONE', #19266, .T. ) ;
#15382 = CARTESIAN_POINT ( 'NONE',  ( 2.534862810676351330, -4.171999357468123115, -46.16669147672499918 ) ) ;
#15383 = B_SPLINE_CURVE_WITH_KNOTS ( 'NONE', 3,
 ( #4617, #28069, #18936, #30908, #6985, #14072, #6514, #21462, #23676, #30600, #9495, #4318, #16264, #28692, #16720, #28538, #23526, #16113, #26339, #23370, #14385, #20997, #18626, #28223, #1960, #6666, #2423, #28387, #21306, #11553, #30747, #9176, #11704, #18778, #3444, #26487, #24867, #24133, #16884, #69, #12899, #20284, #9650, #9811 ),
 .UNSPECIFIED., .F., .F.,
 ( 4, 2, 2, 1, 1, 2, 2, 2, 2, 1, 1, 1, 2, 2, 2, 2, 1, 1, 1, 2, 2, 2, 2, 2, 2, 4 ),
 ( 0.000000000000000000, 0.1249999999999620304, 0.1874999999999430456, 0.2187499999999342470, 0.2343749999999298617, 0.2421874999999276412, 0.2499999999999254485, 0.3749999999998888667, 0.4374999999998705480, 0.4687499999998613887, 0.4843749999998567812, 0.4921874999998557265, 0.4960937499998562816, 0.4999999999998568923, 0.6249999999998990807, 0.6874999999999187317, 0.7187499999999298339, 0.7343749999999368283, 0.7421874999999389377, 0.7460937499999413802, 0.7499999999999437117, 0.8124999999999601430, 0.8437499999999666933, 0.8593749999999701350, 0.8749999999999734657, 1.000000000000000000 ),
 .UNSPECIFIED. ) ;
#15384 = CARTESIAN_POINT ( 'NONE',  ( -3.040504020835836041, -1.733590291693717145, -0.6999999999999784173 ) ) ;
#15385 = CARTESIAN_POINT ( 'NONE',  ( -1.484924240490000047, 1.484924240490000047, 226.6412452697800006 ) ) ;
#15386 = DIRECTION ( 'NONE',  ( 0.000000000000000000, 1.000000000000000000, 0.000000000000000000 ) ) ;
#15387 = EDGE_CURVE ( 'NONE', #19754, #18573, #27290, .T. ) ;
#15388 = CARTESIAN_POINT ( 'NONE',  ( -27.77512470430000135, -2.247288904110000173E-11, 229.2930777930000090 ) ) ;
#15389 = ADVANCED_FACE ( 'NONE', ( #29653, #13600 ), #10612, .T. ) ;
#15390 = CARTESIAN_POINT ( 'NONE',  ( -17.62526668112344908, -8.236461616547455122, -0.6999999999999784173 ) ) ;
#15391 = EDGE_LOOP ( 'NONE', ( #5337, #15314, #17743, #9837 ) ) ;
#15392 = CARTESIAN_POINT ( 'NONE',  ( 1.882647771056455976, 3.960165260869605408, -32.15113063600000487 ) ) ;
#15393 = ORIENTED_EDGE ( 'NONE', *, *, #8259, .T. ) ;
#15394 = CARTESIAN_POINT ( 'NONE',  ( 13.99999999979999821, 21.69999999929999390, -67.09999999999999432 ) ) ;
#15395 = CARTESIAN_POINT ( 'NONE',  ( -0.7556487780321456960, 4.453147011089717111, -51.65792092402499947 ) ) ;
#15396 = ORIENTED_EDGE ( 'NONE', *, *, #24409, .F. ) ;
#15397 = ORIENTED_EDGE ( 'NONE', *, *, #20365, .T. ) ;
#15398 =( NAMED_UNIT ( * ) PLANE_ANGLE_UNIT ( ) SI_UNIT ( $, .RADIAN. ) );
#15399 = ORIENTED_EDGE ( 'NONE', *, *, #14355, .T. ) ;
#15400 = ORIENTED_EDGE ( 'NONE', *, *, #22144, .T. ) ;
#15401 = ADVANCED_FACE ( 'NONE', ( #12970 ), #13436, .T. ) ;
#15402 = CARTESIAN_POINT ( 'NONE',  ( 24.31416967338466861, 13.47842985269137728, 4.493023686000019445 ) ) ;
#15403 = CARTESIAN_POINT ( 'NONE',  ( 17.47393819644387136, 9.934045360783191114, -4.336808689942018722E-16 ) ) ;
#15404 = DIRECTION ( 'NONE',  ( -1.595945597898660305E-12, -0.7071067811865475727, -0.7071067811865475727 ) ) ;
#15405 = CARTESIAN_POINT ( 'NONE',  ( 1.484924240490000047, -1.484924240490000047, 227.6412452697800006 ) ) ;
#15406 = CARTESIAN_POINT ( 'NONE',  ( -21.17667619210000041, 18.05244527720000036, 225.0000000000000000 ) ) ;
#15407 = ADVANCED_FACE ( 'NONE', ( #30278 ), #1333, .F. ) ;
#15408 = CARTESIAN_POINT ( 'NONE',  ( -4.804319815618600664, 1.211543436087829217, -0.6999999999999994005 ) ) ;
#15409 = CARTESIAN_POINT ( 'NONE',  ( -11.00000000000000000, 26.42151601322854759, -59.26168417594741555 ) ) ;
#15410 = CARTESIAN_POINT ( 'NONE',  ( -3.370970677383902103, -1.161062029692211173, 227.6835602974589108 ) ) ;
#15411 = CARTESIAN_POINT ( 'NONE',  ( 353541.3905933150672, -344862.5129886576324, 77944.25516062910901 ) ) ;
#15412 = ADVANCED_FACE ( 'NONE', ( #23051, #10928, #17985 ), #13278, .T. ) ;
#15413 = CARTESIAN_POINT ( 'NONE',  ( 5.466312515054250198, -2.792605348973308477, -11.91474735220000092 ) ) ;
#15414 = CARTESIAN_POINT ( 'NONE',  ( 4.437687981975763307, 3.340062028235890601, -31.36032172560000930 ) ) ;
#15415 = DIRECTION ( 'NONE',  ( 0.000000000000000000, 0.000000000000000000, -1.000000000000000000 ) ) ;
#15416 = DIRECTION ( 'NONE',  ( 0.9316362575375356503, 0.3633921898465274913, 0.000000000000000000 ) ) ;
#15417 = CARTESIAN_POINT ( 'NONE',  ( -4.785279987089964493, -31.71089578132167119, 1.000000000000000888 ) ) ;
#15418 = CARTESIAN_POINT ( 'NONE',  ( 18.26639035967037827, -8.979988381807324060, -0.6999999999999784173 ) ) ;
#15419 = CARTESIAN_POINT ( 'NONE',  ( 3.790912472548403578, -2.108217834232220422, -26.93037294500000201 ) ) ;
#15420 = CARTESIAN_POINT ( 'NONE',  ( 21.32490733757747137, 17.21310361452476201, -0.6999999999999784173 ) ) ;
#15421 = CARTESIAN_POINT ( 'NONE',  ( 8.000000000733132666, -29.34680062213522689, -26.49035620890133202 ) ) ;
#15422 = CARTESIAN_POINT ( 'NONE',  ( 27.79539923781684507, 0.5057481689249130330, 1.000000000000000888 ) ) ;
#15423 = EDGE_CURVE ( 'NONE', #7575, #2099, #28562, .T. ) ;
#15424 = ORIENTED_EDGE ( 'NONE', *, *, #619, .F. ) ;
#15425 = VECTOR ( 'NONE', #30936, 999.9999999999998863 ) ;
#15426 = EDGE_CURVE ( 'NONE', #15866, #30881, #6361, .T. ) ;
#15427 = CARTESIAN_POINT ( 'NONE',  ( -8.999999999970000886, 19.99999999999999645, -45.10000000000000142 ) ) ;
#15428 = CARTESIAN_POINT ( 'NONE',  ( 11.69999999989999928, 19.99999999999999645, -0.6999999999999992895 ) ) ;
#15429 = VERTEX_POINT ( 'NONE', #22726 ) ;
#15430 = VECTOR ( 'NONE', #5390, 1000.000000000000114 ) ;
#15431 = CARTESIAN_POINT ( 'NONE',  ( -1.828693153458612164, -3.500000000000001332, 227.9034567869048544 ) ) ;
#15432 = DIRECTION ( 'NONE',  ( 0.000000000000000000, 0.000000000000000000, 1.000000000000000000 ) ) ;
#15433 = VECTOR ( 'NONE', #29334, 1000.000000000000000 ) ;
#15434 = EDGE_LOOP ( 'NONE', ( #15099, #10755, #11211, #76 ) ) ;
#15435 = CARTESIAN_POINT ( 'NONE',  ( -5.797918472035167525, -115.0360660101943182, 22.14437208026542692 ) ) ;
#15436 = VERTEX_POINT ( 'NONE', #11088 ) ;
#15437 = EDGE_CURVE ( 'NONE', #20967, #16094, #18407, .T. ) ;
#15438 = ORIENTED_EDGE ( 'NONE', *, *, #20701, .F. ) ;
#15439 =( LENGTH_UNIT ( ) NAMED_UNIT ( * ) SI_UNIT ( .MILLI., .METRE. ) );
#15440 = ORIENTED_EDGE ( 'NONE', *, *, #5479, .F. ) ;
#15441 = CARTESIAN_POINT ( 'NONE',  ( -16.95738181089354057, 9.897562529807188980, -0.6999999999999783062 ) ) ;
#15442 = CARTESIAN_POINT ( 'NONE',  ( -17.89938223499811087, -9.307365792571914653, -0.6999999999999784173 ) ) ;
#15443 = DIRECTION ( 'NONE',  ( 0.8660254037843290176, 0.5000000000001900702, -0.000000000000000000 ) ) ;
#15444 = LINE ( 'NONE', #18258, #26892 ) ;
#15445 = CARTESIAN_POINT ( 'NONE',  ( -0.1113126278295820393, -21.81692582113983647, -30.17614928725404155 ) ) ;
#15446 = CARTESIAN_POINT ( 'NONE',  ( -24.31107512894012146, -13.48383474011653860, 5.495825983432886197 ) ) ;
#15447 = AXIS2_PLACEMENT_3D ( 'NONE', #10849, #8007, #950 ) ;
#15448 = CARTESIAN_POINT ( 'NONE',  ( 9.590600648852312560, -25.77356060526425452, 204.6037742833236166 ) ) ;
#15449 = CARTESIAN_POINT ( 'NONE',  ( 2.045342621092061552, -0.5496705570015011366, 226.6412452697799722 ) ) ;
#15450 = AXIS2_PLACEMENT_3D ( 'NONE', #5348, #19674, #29257 ) ;
#15451 = CARTESIAN_POINT ( 'NONE',  ( -1.949381390262891589, -5.750991590113663676, -1.175630512700004404 ) ) ;
#15452 = CARTESIAN_POINT ( 'NONE',  ( 4.354753084053718304, 0.1085053810021633369, -20.17661200060000581 ) ) ;
#15453 = CARTESIAN_POINT ( 'NONE',  ( -17.72558663041863269, -8.340546693701178071, -0.6999999999999783062 ) ) ;
#15454 = AXIS2_PLACEMENT_3D ( 'NONE', #3562, #5770, #13157 ) ;
#15455 = FACE_OUTER_BOUND ( 'NONE', #1597, .T. ) ;
#15456 = CARTESIAN_POINT ( 'NONE',  ( -21.60246165930000117, 17.31101082549999859, 230.6577119970000069 ) ) ;
#15457 = CARTESIAN_POINT ( 'NONE',  ( -12.12499970569999874, 20.99999999999999645, -55.73512393480000071 ) ) ;
#15458 = CARTESIAN_POINT ( 'NONE',  ( 27.79999999999999716, 2.355804440410000085E-11, 229.0000000000000000 ) ) ;
#15459 = CARTESIAN_POINT ( 'NONE',  ( 14.43445127310000053, -11.21796138520000063, 230.6999999999999886 ) ) ;
#15460 = CARTESIAN_POINT ( 'NONE',  ( 3.973196233977206671, -0.1784912441314041864, -40.72991899601151289 ) ) ;
#15461 = EDGE_CURVE ( 'NONE', #7351, #30811, #28164, .T. ) ;
#15462 = ORIENTED_EDGE ( 'NONE', *, *, #20299, .F. ) ;
#15463 = CARTESIAN_POINT ( 'NONE',  ( 4.311559700750661861, -2.373910439939187267, -57.55843849682501201 ) ) ;
#15464 = CARTESIAN_POINT ( 'NONE',  ( 4.638687372183706081, -18.46298696207763967, -30.14307165816331135 ) ) ;
#15465 = EDGE_CURVE ( 'NONE', #7630, #16094, #31059, .T. ) ;
#15466 = CARTESIAN_POINT ( 'NONE',  ( 5.763395275833943288, -2.111988417915284355, -5.836105321700000736 ) ) ;
#15467 = EDGE_LOOP ( 'NONE', ( #4220, #4446, #20851, #2039 ) ) ;
#15468 = EDGE_CURVE ( 'NONE', #14645, #9943, #10882, .T. ) ;
#15469 = CARTESIAN_POINT ( 'NONE',  ( -19.53673505992006554, -20.39066108913833020, -0.6999999999999784173 ) ) ;
#15470 = CIRCLE ( 'NONE', #18483, 4.000000000000001776 ) ;
#15471 = CARTESIAN_POINT ( 'NONE',  ( -4.224014620368086170, 0.7320701895516892321, -68.10000000002501963 ) ) ;
#15472 = EDGE_CURVE ( 'NONE', #18728, #3218, #15383, .T. ) ;
#15473 = ORIENTED_EDGE ( 'NONE', *, *, #1892, .T. ) ;
#15474 = VERTEX_POINT ( 'NONE', #29576 ) ;
#15475 = VERTEX_POINT ( 'NONE', #5659 ) ;
#15476 = VECTOR ( 'NONE', #6816, 1000.000000000000000 ) ;
#15477 = CARTESIAN_POINT ( 'NONE',  ( 3.230522845497924234, 0.1026436873742902073, -94.56600524946087205 ) ) ;
#15478 = ORIENTED_EDGE ( 'NONE', *, *, #24567, .T. ) ;
#15479 = DIRECTION ( 'NONE',  ( 0.000000000000000000, 1.000000000000000000, 0.000000000000000000 ) ) ;
#15480 = AXIS2_PLACEMENT_3D ( 'NONE', #26349, #12478, #7147 ) ;
#15481 = CARTESIAN_POINT ( 'NONE',  ( -7.861312627733067160, -0.9159326019477498360, -37.03243899222264446 ) ) ;
#15482 = CARTESIAN_POINT ( 'NONE',  ( 2.833778097863427714, 3.583098331959792660, -63.63768011632500787 ) ) ;
#15483 = CARTESIAN_POINT ( 'NONE',  ( -22.27803938659999972, -19.69272062099999943, 230.0000000000000000 ) ) ;
#15484 = CARTESIAN_POINT ( 'NONE',  ( 1.891787376696312029, -3.825877967903179577, -67.61367454182500580 ) ) ;
#15485 = CARTESIAN_POINT ( 'NONE',  ( 10.46446609389999871, 20.99999999999999645, -54.63553390589999736 ) ) ;
#15486 = CARTESIAN_POINT ( 'NONE',  ( -26.85688130224987091, -1.306556711637668622, -1.399999999999998579 ) ) ;
#15487 = AXIS2_PLACEMENT_3D ( 'NONE', #24059, #2803, #17420 ) ;
#15488 = ORIENTED_EDGE ( 'NONE', *, *, #14479, .T. ) ;
#15489 = CARTESIAN_POINT ( 'NONE',  ( -5.857861475075242019, -1.837656413297739766, -9.423230889000002719 ) ) ;
#15490 = CARTESIAN_POINT ( 'NONE',  ( 24.88589369718092215, -13.89120818692358483, 3.904029272000009154 ) ) ;
#15491 = CARTESIAN_POINT ( 'NONE',  ( 14.77204036655766650, -30.50348270133963169, -32.15076601107894305 ) ) ;
#15492 = ORIENTED_EDGE ( 'NONE', *, *, #13732, .T. ) ;
#15493 = CARTESIAN_POINT ( 'NONE',  ( 24.12694114270000156, -13.81062811039999971, 223.9040346120000038 ) ) ;
#15494 = CARTESIAN_POINT ( 'NONE',  ( 11.08346179031908640, -28.41490585489483678, 36.39444872449999480 ) ) ;
#15495 = CARTESIAN_POINT ( 'NONE',  ( -28.49999999959999641, -10.47094308429999998, 229.0000000000000000 ) ) ;
#15496 = CARTESIAN_POINT ( 'NONE',  ( 21.92393651391584086, 17.69663393520839989, 0.9999999989999952543 ) ) ;
#15497 = CARTESIAN_POINT ( 'NONE',  ( -8.727399452413349579, -25.34090985533206108, 206.0457211097556751 ) ) ;
#15498 = CARTESIAN_POINT ( 'NONE',  ( -5.162912894389027230, 3.035924517800103750, -44.84354844312500177 ) ) ;
#15499 = CARTESIAN_POINT ( 'NONE',  ( -23.39354070939840824, -15.01969650306709170, 5.760134161999996394 ) ) ;
#15500 = PLANE ( 'NONE',  #6234 ) ;
#15501 = VERTEX_POINT ( 'NONE', #22654 ) ;
#15502 = CARTESIAN_POINT ( 'NONE',  ( -26.05511412830000140, 14.93229958979999950, 229.0000000000000000 ) ) ;
#15503 = CARTESIAN_POINT ( 'NONE',  ( -9.738910687886859208, -24.96785170200599069, 27.46683069121352005 ) ) ;
#15504 = CARTESIAN_POINT ( 'NONE',  ( -0.2758148021258401417, -3.950156389878017649, -68.10000000002503384 ) ) ;
#15505 = PLANE ( 'NONE',  #8199 ) ;
#15506 = SHAPE_REPRESENTATION_RELATIONSHIP ( 'NONE' , 'NONE' ,  #16405, #25297 ) ;
#15507 = CARTESIAN_POINT ( 'NONE',  ( 14.69473318574859455, -25.93431317557370619, -33.55782932027766208 ) ) ;
#15508 = LINE ( 'NONE', #1359, #9936 ) ;
#15509 = CARTESIAN_POINT ( 'NONE',  ( -1.231152431062140007, -5.073857922501755269, -62.69311227092499905 ) ) ;
#15510 = VERTEX_POINT ( 'NONE', #21619 ) ;
#15511 = CARTESIAN_POINT ( 'NONE',  ( 18.04539700001577529, 20.00000247597757408, 230.6997258737370942 ) ) ;
#15512 = ORIENTED_EDGE ( 'NONE', *, *, #10047, .F. ) ;
#15514 = CARTESIAN_POINT ( 'NONE',  ( -4.663556906300703631, -30.90433882808243027, 0.7069209039999857502 ) ) ;
#15513 = TOROIDAL_SURFACE ( 'NONE', #6998, 29.80000000000000071, 3.000000000000000000 ) ;
#15515 = ORIENTED_EDGE ( 'NONE', *, *, #80, .F. ) ;
#15516 = ADVANCED_FACE ( 'NONE', ( #7445, #25010 ), #12012, .T. ) ;
#15517 = CARTESIAN_POINT ( 'NONE',  ( 0.000000000000000000, 0.000000000000000000, 88.33953982530000815 ) ) ;
#15518 = CARTESIAN_POINT ( 'NONE',  ( 24.98823331316959440, -13.70626928515100573, 3.904029301000005781 ) ) ;
#15519 = CARTESIAN_POINT ( 'NONE',  ( 23.23277120357798964, 15.26692725135965745, 4.999998581000003384 ) ) ;
#15520 = CARTESIAN_POINT ( 'NONE',  ( -17.49230054464816320, -24.30879446532417276, -32.61973445220952073 ) ) ;
#15521 = PLANE ( 'NONE',  #28009 ) ;
#15522 = LINE ( 'NONE', #12861, #13511 ) ;
#15523 = ORIENTED_EDGE ( 'NONE', *, *, #7842, .T. ) ;
#15524 = CARTESIAN_POINT ( 'NONE',  ( 10.99999999979999998, 20.99999999999999645, -58.51619795479999908 ) ) ;
#15525 = CARTESIAN_POINT ( 'NONE',  ( 27.29823224880000154, -5.927324070049999562E-14, 230.6577119970000069 ) ) ;
#15526 = EDGE_CURVE ( 'NONE', #2527, #15917, #19251, .T. ) ;
#15527 = TOROIDAL_SURFACE ( 'NONE', #29099, 30.50000000000000000, 3.000000000000000000 ) ;
#15528 = CARTESIAN_POINT ( 'NONE',  ( 3.710789578725101734, 2.835545959904678170, -23.36727430110000014 ) ) ;
#15529 = CARTESIAN_POINT ( 'NONE',  ( 23.31845629885299331, -13.20933888571149595, 3.912379060708174983 ) ) ;
#15530 = DIRECTION ( 'NONE',  ( -1.000000000000000000, 0.000000000000000000, 0.000000000000000000 ) ) ;
#15531 = ADVANCED_BREP_SHAPE_REPRESENTATION ( '', ( #21644, #17722 ), #13276 ) ;
#15532 = CARTESIAN_POINT ( 'NONE',  ( 0.1441797511781169050, -27.80021098851407402, 223.9000014190000627 ) ) ;
#15533 = CARTESIAN_POINT ( 'NONE',  ( -5.044271480141131470, 2.992596682328089841, -50.03267869292500336 ) ) ;
#15534 = AXIS2_PLACEMENT_3D ( 'NONE', #2762, #29490, #12355 ) ;
#15535 = LINE ( 'NONE', #3737, #11213 ) ;
#15536 = CARTESIAN_POINT ( 'NONE',  ( 1.841797396446240631, -26.73663745407121795, 210.0000000000000284 ) ) ;
#15537 = CARTESIAN_POINT ( 'NONE',  ( -20.03097513009040398, 19.99998374455136840, 229.7883118818511150 ) ) ;
#15538 = CARTESIAN_POINT ( 'NONE',  ( -12.12499970530000049, 21.69999999919999212, -55.73512393530000253 ) ) ;
#15539 = CARTESIAN_POINT ( 'NONE',  ( 8.160452367545499186, -25.52912514472581407, 23.07342428570553494 ) ) ;
#15540 = VERTEX_POINT ( 'NONE', #15110 ) ;
#15541 = CARTESIAN_POINT ( 'NONE',  ( 2.022420680230010870, -3.847796821814265300, -33.70721934059999825 ) ) ;
#15542 = ORIENTED_EDGE ( 'NONE', *, *, #16313, .F. ) ;
#15543 = ADVANCED_FACE ( 'NONE', ( #26642 ), #12391, .F. ) ;
#15544 = CARTESIAN_POINT ( 'NONE',  ( 13.40012576665181321, 21.69999999994393391, -68.94240556069520665 ) ) ;
#15545 = CARTESIAN_POINT ( 'NONE',  ( -4.064488300603595228, -4.392874523441014034, -50.67612412472499983 ) ) ;
#15546 = ORIENTED_EDGE ( 'NONE', *, *, #7989, .F. ) ;
#15547 = APPLICATION_PROTOCOL_DEFINITION ( 'draft international standard', 'automotive_design', 1998, #17015 ) ;
#15548 = ORIENTED_EDGE ( 'NONE', *, *, #5839, .F. ) ;
#15549 = ORIENTED_EDGE ( 'NONE', *, *, #24315, .T. ) ;
#15550 = CARTESIAN_POINT ( 'NONE',  ( 23.81866173088643635, 14.33570044285385947, 3.899998581000013509 ) ) ;
#15551 = CARTESIAN_POINT ( 'NONE',  ( 11.08346179031908285, -28.41490585489482967, 86.39444872449999480 ) ) ;
#15552 = CARTESIAN_POINT ( 'NONE',  ( -27.50000000000000000, 3.367667473009999970E-15, 86.39444872359999295 ) ) ;
#15553 = DIRECTION ( 'NONE',  ( 1.000000000000000000, 0.000000000000000000, 0.000000000000000000 ) ) ;
#15554 = CARTESIAN_POINT ( 'NONE',  ( -5.016375772021067547, 0.4838088423305476060, -0.6999999999999992895 ) ) ;
#15555 = CARTESIAN_POINT ( 'NONE',  ( 1.537204335059164872, 5.727607561491170785, -1.053410702900002160 ) ) ;
#15556 = CARTESIAN_POINT ( 'NONE',  ( 11.52349576909532303, 26.37260064581004215, -59.27948791368598336 ) ) ;
#15557 = CARTESIAN_POINT ( 'NONE',  ( 8.000000000836360314, -17.41770198678077719, -37.61454294949587052 ) ) ;
#15558 = VERTEX_POINT ( 'NONE', #29730 ) ;
#15559 = EDGE_CURVE ( 'NONE', #14877, #16822, #10991, .T. ) ;
#15560 = CARTESIAN_POINT ( 'NONE',  ( 6.034652528523337445, 2.501332855249893683, -12.09261350020000236 ) ) ;
#15561 = CARTESIAN_POINT ( 'NONE',  ( -1.932773295258156887, 4.259541830411037289, -31.72635571290000200 ) ) ;
#15562 = CARTESIAN_POINT ( 'NONE',  ( -27.23548387100000312, 8.881784196999999612E-15, 41.66046017469999896 ) ) ;
#15563 = CARTESIAN_POINT ( 'NONE',  ( 18.62349342026574917, 19.80369317695730302, 0.06728435000000199118 ) ) ;
#15564 = CARTESIAN_POINT ( 'NONE',  ( -2.407487872911075577, -2.830108685506040000, 227.7614631413448762 ) ) ;
#15565 = DIRECTION ( 'NONE',  ( 1.000000000000000000, -0.000000000000000000, 0.000000000000000000 ) ) ;
#15566 = CARTESIAN_POINT ( 'NONE',  ( 0.07512830594656044747, -4.346272141329931671, -33.41110030499999795 ) ) ;
#15567 = CARTESIAN_POINT ( 'NONE',  ( 20.30405755279999980, 20.00000000000000000, 228.1999999569999886 ) ) ;
#15568 = CARTESIAN_POINT ( 'NONE',  ( 14.85000000009999788, -27.00000000000000000, -28.39999999989999679 ) ) ;
#15569 = CARTESIAN_POINT ( 'NONE',  ( 21.70992212615148986, 18.50697891487987334, 5.000000000000004441 ) ) ;
#15570 = ORIENTED_EDGE ( 'NONE', *, *, #13374, .T. ) ;
#15571 = ORIENTED_EDGE ( 'NONE', *, *, #3470, .F. ) ;
#15572 = EDGE_CURVE ( 'NONE', #24391, #8738, #17041, .T. ) ;
#15573 = AXIS2_PLACEMENT_3D ( 'NONE', #20681, #30444, #6664 ) ;
#15574 = EDGE_CURVE ( 'NONE', #14751, #24648, #12161, .T. ) ;
#15575 = CARTESIAN_POINT ( 'NONE',  ( 23.98258507289250474, 15.39789216307533160, 5.760134169000008519 ) ) ;
#15576 = LINE ( 'NONE', #1276, #23819 ) ;
#15577 = B_SPLINE_CURVE_WITH_KNOTS ( 'NONE', 3,
 ( #537, #21931, #29147, #13950, #17188, #23563, #26790, #5234, #12009, #19720 ),
 .UNSPECIFIED., .F., .F.,
 ( 4, 2, 2, 2, 4 ),
 ( 0.000000000000000000, 0.2500000000000000000, 0.5000000000000000000, 0.7500000000000000000, 1.000000000000000000 ),
 .UNSPECIFIED. ) ;
#15578 = ORIENTED_EDGE ( 'NONE', *, *, #9715, .T. ) ;
#15579 = DIRECTION ( 'NONE',  ( 0.7071067811842725037, 0.2886612846624971307, 0.6455034180701249014 ) ) ;
#15580 = CARTESIAN_POINT ( 'NONE',  ( 2.773968441741427426, -2.033165918578674791, -36.48752789467021529 ) ) ;
#15581 = ORIENTED_EDGE ( 'NONE', *, *, #28962, .F. ) ;
#15582 = CARTESIAN_POINT ( 'NONE',  ( -9.219833965033632950, -25.90918750570071438, 24.42156808705805560 ) ) ;
#15583 = ORIENTED_EDGE ( 'NONE', *, *, #2023, .T. ) ;
#15584 = ORIENTED_EDGE ( 'NONE', *, *, #8610, .T. ) ;
#15585 = EDGE_CURVE ( 'NONE', #27858, #5618, #5963, .T. ) ;
#15586 =( LENGTH_UNIT ( ) NAMED_UNIT ( * ) SI_UNIT ( .MILLI., .METRE. ) );
#15587 = EDGE_LOOP ( 'NONE', ( #22985, #22494, #12396, #13589, #19553, #12298, #8529, #11305, #7100, #19944 ) ) ;
#15588 = CARTESIAN_POINT ( 'NONE',  ( 27.56257419730000180, 3.635153433429999645E-14, 230.5592437530000041 ) ) ;
#15589 = PRODUCT_DEFINITION_SHAPE ( 'NONE', 'NONE',  #54 ) ;
#15590 = CARTESIAN_POINT ( 'NONE',  ( 10.69999999930000101, -24.00000000000000000, -28.40000000000000213 ) ) ;
#15591 = LINE ( 'NONE', #25196, #14571 ) ;
#15592 = ORIENTED_EDGE ( 'NONE', *, *, #4950, .F. ) ;
#15593 = CARTESIAN_POINT ( 'NONE',  ( -24.83828730555975284, 12.48688483815296735, 5.104216618000034345 ) ) ;
#15594 = B_SPLINE_CURVE_WITH_KNOTS ( 'NONE', 3,
 ( #23721, #21355, #7030, #30951, #16466, #26227 ),
 .UNSPECIFIED., .F., .F.,
 ( 4, 2, 4 ),
 ( 0.000000000000000000, 0.5000000000000000000, 1.000000000000000000 ),
 .UNSPECIFIED. ) ;
#15595 = B_SPLINE_CURVE_WITH_KNOTS ( 'NONE', 3,
 ( #14367, #9628, #2703, #21914, #9789, #198 ),
 .UNSPECIFIED., .F., .F.,
 ( 4, 2, 4 ),
 ( 0.000000000000000000, 0.5000000000000000000, 1.000000000000000000 ),
 .UNSPECIFIED. ) ;
#15596 = CARTESIAN_POINT ( 'NONE',  ( -0.3775595308767857317, -28.49777658967402871, 4.319846982000025370 ) ) ;
#15597 = EDGE_LOOP ( 'NONE', ( #22412, #24690, #12490, #29169, #3342 ) ) ;
#15598 = ADVANCED_FACE ( 'NONE', ( #10389 ), #3295, .F. ) ;
#15599 = CARTESIAN_POINT ( 'NONE',  ( 7.365079183348029801, -26.49619795852259685, 208.0568234296057426 ) ) ;
#15600 = CARTESIAN_POINT ( 'NONE',  ( 24.18685237987300951, -13.70673315802992676, 3.927097088518238799 ) ) ;
#15601 = ORIENTED_EDGE ( 'NONE', *, *, #4892, .T. ) ;
#15602 = CARTESIAN_POINT ( 'NONE',  ( -4.757675747652303500, -1.918655839533711660, -1.934697434500002755 ) ) ;
#15603 = CARTESIAN_POINT ( 'NONE',  ( -0.7560282158644051620, 4.289996408053716515, -19.33583244400000822 ) ) ;
#15604 = CARTESIAN_POINT ( 'NONE',  ( -9.999999999919999993, -25.00000000000000000, -7.274962171499997687 ) ) ;
#15605 = CARTESIAN_POINT ( 'NONE',  ( 353532.1637640000554, -340227.0254469999345, -96277.77758659989922 ) ) ;
#15606 = CARTESIAN_POINT ( 'NONE',  ( 0.5632927345713620859, -3.521042344241311017, -88.52261276296684400 ) ) ;
#15607 = CARTESIAN_POINT ( 'NONE',  ( -22.44209336489999984, 17.98384493009999829, 229.7625741969999922 ) ) ;
#15608 = DIRECTION ( 'NONE',  ( -1.000000000000000000, 3.980999999999999294E-12, -1.940999999999999504E-12 ) ) ;
#15609 = CARTESIAN_POINT ( 'NONE',  ( -23.24667624907481667, -14.69156368041588934, 224.8543268298566602 ) ) ;
#15610 = EDGE_CURVE ( 'NONE', #17625, #29694, #21771, .T. ) ;
#15611 = AXIS2_PLACEMENT_3D ( 'NONE', #20806, #30876, #23174 ) ;
#15612 = PLANE ( 'NONE',  #23261 ) ;
#15613 = CARTESIAN_POINT ( 'NONE',  ( 7.908773014210000341, 16.35323874420000223, 230.6999999999999886 ) ) ;
#15614 = CARTESIAN_POINT ( 'NONE',  ( 4.811998177268387522, -8.737919599237365276, -33.21740102630603531 ) ) ;
#15615 = ORIENTED_EDGE ( 'NONE', *, *, #4671, .F. ) ;
#15616 = CARTESIAN_POINT ( 'NONE',  ( 5.975646968830259809, -0.1056191442178888718, -58.09793411332499602 ) ) ;
#15617 = CARTESIAN_POINT ( 'NONE',  ( -7.861312627756137594, -6.912605513598457208, -37.44547201166600559 ) ) ;
#15618 = VERTEX_POINT ( 'NONE', #27374 ) ;
#15619 = CARTESIAN_POINT ( 'NONE',  ( 0.2392016894930265591, 6.101552847015987879, -7.937690181100006903 ) ) ;
#15620 = VERTEX_POINT ( 'NONE', #13047 ) ;
#15621 = CARTESIAN_POINT ( 'NONE',  ( -3.552713678799999608E-15, 0.000000000000000000, 37.93968498539999956 ) ) ;
#15622 = DIRECTION ( 'NONE',  ( -0.7071067811896794009, -0.6355433650254203037, 0.3099752105697101134 ) ) ;
#15623 = ORIENTED_EDGE ( 'NONE', *, *, #17978, .T. ) ;
#15624 = ORIENTED_EDGE ( 'NONE', *, *, #20220, .T. ) ;
#15625 = ORIENTED_EDGE ( 'NONE', *, *, #19160, .T. ) ;
#15626 = DIRECTION ( 'NONE',  ( 0.000000000000000000, 0.000000000000000000, 1.000000000000000000 ) ) ;
#15627 = VERTEX_POINT ( 'NONE', #8315 ) ;
#15628 = DIRECTION ( 'NONE',  ( 0.000000000000000000, 0.000000000000000000, 1.000000000000000000 ) ) ;
#15629 = CARTESIAN_POINT ( 'NONE',  ( -8.699999999629596914, -20.29243514309546370, -40.76306209186606822 ) ) ;
#15630 = CARTESIAN_POINT ( 'NONE',  ( -1.313688977135577529, 5.115945099120181361, -65.45876360982501296 ) ) ;
#15631 = CARTESIAN_POINT ( 'NONE',  ( 1.079837148504761979, -28.48011631689465517, 5.965513408196154721 ) ) ;
#15632 = AXIS2_PLACEMENT_3D ( 'NONE', #7529, #24371, #12402 ) ;
#15633 = CARTESIAN_POINT ( 'NONE',  ( -28.03861306157277866, -0.5101735396241460219, -0.2432540810000105580 ) ) ;
#15634 = EDGE_CURVE ( 'NONE', #9121, #13665, #9761, .T. ) ;
#15635 = CARTESIAN_POINT ( 'NONE',  ( -17.41454186824532258, -23.48437545276489047, -24.65624529799447018 ) ) ;
#15636 = DIRECTION ( 'NONE',  ( 0.5000000000001894040, 0.8660254037843291286, 0.000000000000000000 ) ) ;
#15637 = ORIENTED_EDGE ( 'NONE', *, *, #11548, .F. ) ;
#15638 = EDGE_CURVE ( 'NONE', #453, #29484, #24431, .T. ) ;
#15639 = CARTESIAN_POINT ( 'NONE',  ( -0.8069922590487529357, 5.436669193145879042, -9.867720916600005054 ) ) ;
#15640 = CARTESIAN_POINT ( 'NONE',  ( 17.14656078602323319, -7.900182044548062166, -1.000005633855494125E-09 ) ) ;
#15641 = EDGE_CURVE ( 'NONE', #4159, #27653, #16347, .T. ) ;
#15642 = CARTESIAN_POINT ( 'NONE',  ( 9.999999999959999997, -29.06670649020000141, -26.22546295170000263 ) ) ;
#15643 = ORIENTED_EDGE ( 'NONE', *, *, #22114, .F. ) ;
#15644 = CARTESIAN_POINT ( 'NONE',  ( 3.862245930686361461, 0.3103938167200858689, 227.8554272724557279 ) ) ;
#15645 = CARTESIAN_POINT ( 'NONE',  ( -23.94167924027569327, -14.12976891190553452, 6.079852602000002548 ) ) ;
#15646 = CARTESIAN_POINT ( 'NONE',  ( 21.16705260770000052, -21.30254494060000070, 222.0000000000000000 ) ) ;
#15647 = LINE ( 'NONE', #6370, #20195 ) ;
#15648 = CARTESIAN_POINT ( 'NONE',  ( 8.000000000832923064, -18.43160947565852226, -34.96026953474216725 ) ) ;
#15649 = CARTESIAN_POINT ( 'NONE',  ( 5.066518387468507356, -3.138291312573631586, -49.33324460762499797 ) ) ;
#15650 = CARTESIAN_POINT ( 'NONE',  ( -23.29312071521372118, -15.17488101142239643, 5.506989586000016423 ) ) ;
#15651 = LINE ( 'NONE', #25580, #11765 ) ;
#15652 = ORIENTED_EDGE ( 'NONE', *, *, #14351, .F. ) ;
#15653 = CARTESIAN_POINT ( 'NONE',  ( 24.74993095443131352, -14.13250376055072266, 3.957489350000009676 ) ) ;
#15654 = CARTESIAN_POINT ( 'NONE',  ( 27.79999999990000248, 4.333901782529999025, 227.5999999999999943 ) ) ;
#15655 = CIRCLE ( 'NONE', #11644, 4.175165894169885483 ) ;
#15656 = B_SPLINE_CURVE_WITH_KNOTS ( 'NONE', 3,
 ( #8804, #16357, #30534, #28005 ),
 .UNSPECIFIED., .F., .F.,
 ( 4, 4 ),
 ( 0.000000000000000000, 1.000000000000000000 ),
 .UNSPECIFIED. ) ;
#15657 = CARTESIAN_POINT ( 'NONE',  ( 2.229356664414377853, -3.595762368830520916, -68.10000000002503384 ) ) ;
#15658 = CIRCLE ( 'NONE', #12646, 3.200000000000002398 ) ;
#15659 = CIRCLE ( 'NONE', #3103, 2.000000000000000000 ) ;
#15660 = CARTESIAN_POINT ( 'NONE',  ( -26.79556473285982321, -0.4875557887251183442, -0.6999999999999784173 ) ) ;
#15661 = CARTESIAN_POINT ( 'NONE',  ( -3.221943696565561677, -2.259922541635331239, -44.10000000002498410 ) ) ;
#15662 = PLANE ( 'NONE',  #29768 ) ;
#15663 = DIRECTION ( 'NONE',  ( -1.000000000000000000, 5.665498452320000818E-16, 0.000000000000000000 ) ) ;
#15664 = CARTESIAN_POINT ( 'NONE',  ( 5.896017893897736784, 2.415859114112482775, -60.89141554682500157 ) ) ;
#15665 = ORIENTED_EDGE ( 'NONE', *, *, #1965, .F. ) ;
#15666 = CARTESIAN_POINT ( 'NONE',  ( 19.97801547478277584, 19.99997970718940010, 229.8634922149824149 ) ) ;
#15667 = ORIENTED_EDGE ( 'NONE', *, *, #20592, .T. ) ;
#15668 = CARTESIAN_POINT ( 'NONE',  ( 14.20787920732396969, -27.27274267807110775, 0.5514294940000274980 ) ) ;
#15669 = ORIENTED_EDGE ( 'NONE', *, *, #26420, .F. ) ;
#15670 = CARTESIAN_POINT ( 'NONE',  ( -1.484924240490000047, 1.484924240490000047, 226.6412452697800006 ) ) ;
#15671 = CARTESIAN_POINT ( 'NONE',  ( 21.16705260759999874, -21.30254494060000070, 229.0000000000000000 ) ) ;
#15672 = CARTESIAN_POINT ( 'NONE',  ( 0.7509949761426776282, 3.448174246630131279, 0.000000000000000000 ) ) ;
#15673 = AXIS2_PLACEMENT_3D ( 'NONE', #923, #621, #22164 ) ;
#15674 = CARTESIAN_POINT ( 'NONE',  ( -26.13752726800887771, 9.883145870918147224, 8.000000000000007105 ) ) ;
#15675 = CARTESIAN_POINT ( 'NONE',  ( -12.30772508779121921, -22.00000000000000711, -27.95972194141362976 ) ) ;
#15676 = EDGE_CURVE ( 'NONE', #30352, #25224, #1725, .T. ) ;
#15677 = CARTESIAN_POINT ( 'NONE',  ( 5.638687372243864182, -5.597492073914120070, -34.74908987243544090 ) ) ;
#15678 = EDGE_LOOP ( 'NONE', ( #28341, #30523, #24769, #8715 ) ) ;
#15679 = CARTESIAN_POINT ( 'NONE',  ( 28.49528339128749366, 0.5184828350247233653, 1.000000000000000888 ) ) ;
#15680 = DIRECTION ( 'NONE',  ( 0.9316362575375356503, 0.3633921898465274913, 0.000000000000000000 ) ) ;
#15681 = CARTESIAN_POINT ( 'NONE',  ( 0.6688362735999796582, -27.79232735177769342, 225.8855372596424900 ) ) ;
#15682 = CARTESIAN_POINT ( 'NONE',  ( -2.788509597074717572, -2.169696472188583858, 230.8175759419288795 ) ) ;
#15683 = DIRECTION ( 'NONE',  ( 2.764840495839172918E-12, 0.9128796883888953273, -0.4082287037029531107 ) ) ;
#15684 = FACE_BOUND ( 'NONE', #29644, .T. ) ;
#15685 = CARTESIAN_POINT ( 'NONE',  ( -2.947640775130000104E-14, -27.50000000000000000, 226.0999999999999943 ) ) ;
#15686 = PLANE ( 'NONE',  #6129 ) ;
#15687 = CARTESIAN_POINT ( 'NONE',  ( -4.185672079393965461, 2.483218523716621107, -50.43267869292500194 ) ) ;
#15688 = DIRECTION ( 'NONE',  ( 0.7198537139083028835, -0.6941258031311204890, 0.000000000000000000 ) ) ;
#15689 = DIRECTION ( 'NONE',  ( -0.3642835349036590564, 0.000000000000000000, -0.9312880897971875793 ) ) ;
#15690 = DIRECTION ( 'NONE',  ( 0.000000000000000000, -2.256683728769999802E-12, -1.000000000000000000 ) ) ;
#15691 = CIRCLE ( 'NONE', #17204, 3.199999983039998774 ) ;
#15692 = DIRECTION ( 'NONE',  ( 0.000000000000000000, 1.000000000000000000, 0.000000000000000000 ) ) ;
#15693 = ORIENTED_EDGE ( 'NONE', *, *, #5031, .F. ) ;
#15694 = CARTESIAN_POINT ( 'NONE',  ( 0.08264113651937701754, -4.780899355463231970, -34.34860030499999795 ) ) ;
#15695 = ORIENTED_EDGE ( 'NONE', *, *, #14009, .T. ) ;
#15696 = CARTESIAN_POINT ( 'NONE',  ( -10.69999999999999929, -120.0000000000000000, -41.24671599700000257 ) ) ;
#15697 = CARTESIAN_POINT ( 'NONE',  ( 1.321824945545741814, 4.319062652178985218, -51.86125421262499202 ) ) ;
#15698 = VERTEX_POINT ( 'NONE', #30038 ) ;
#15699 = ADVANCED_FACE ( 'NONE', ( #23133 ), #6592, .F. ) ;
#15700 = SHAPE_DEFINITION_REPRESENTATION ( #8553, #20626 ) ;
#15701 = ORIENTED_EDGE ( 'NONE', *, *, #22817, .F. ) ;
#15702 = ORIENTED_EDGE ( 'NONE', *, *, #16401, .T. ) ;
#15703 = CARTESIAN_POINT ( 'NONE',  ( -17.90616261956523303, -9.270408387734455857, 0.000000000000000000 ) ) ;
#15704 = LINE ( 'NONE', #3436, #12455 ) ;
#15705 = DIRECTION ( 'NONE',  ( -0.7600087925169251024, -0.4151946956549595336, -0.4999999999969509945 ) ) ;
#15706 = B_SPLINE_CURVE_WITH_KNOTS ( 'NONE', 1,
 ( #16580, #16889 ),
 .UNSPECIFIED., .F., .F.,
 ( 2, 2 ),
 ( -0.0003775348956340000232, 0.7000000117410000167 ),
 .UNSPECIFIED. ) ;
#15707 = CYLINDRICAL_SURFACE ( 'NONE', #11437, 27.50000000000000000 ) ;
#15708 = B_SPLINE_CURVE_WITH_KNOTS ( 'NONE', 3,
 ( #5856, #15460, #25065, #27726, #1144, #3498, #13094, #24756, #6171, #3191 ),
 .UNSPECIFIED., .F., .F.,
 ( 4, 2, 2, 2, 4 ),
 ( 0.000000000000000000, 0.2500000000000000000, 0.5000000000000000000, 0.7500000000000000000, 1.000000000000000000 ),
 .UNSPECIFIED. ) ;
#15709 = CARTESIAN_POINT ( 'NONE',  ( -0.6483608311672878211, -27.49254329982247214, 4.090437960807658868 ) ) ;
#15710 = DIRECTION ( 'NONE',  ( -0.3090169943750401549, -0.9510565162951233331, 0.000000000000000000 ) ) ;
#15711 = CARTESIAN_POINT ( 'NONE',  ( -6.055223678858003389, -2.441925613954294860, -0.9971974345000036433 ) ) ;
#15712 = CARTESIAN_POINT ( 'NONE',  ( -3.333579493018210105, -1.225759174659744932, 227.6757455870635454 ) ) ;
#15713 = CARTESIAN_POINT ( 'NONE',  ( 26.30490654700000164, 9.885210762690000763, 222.0000000000000000 ) ) ;
#15714 = VERTEX_POINT ( 'NONE', #6284 ) ;
#15715 = CARTESIAN_POINT ( 'NONE',  ( -4.101794773660127902, 5.071170285176791914, -13.60352819870000474 ) ) ;
#15716 = CARTESIAN_POINT ( 'NONE',  ( 4.051823674760414384, -0.6775361292690335047, -35.24517599850000238 ) ) ;
#15717 = CYLINDRICAL_SURFACE ( 'NONE', #12661, 26.80000000000002203 ) ;
#15718 = B_SPLINE_CURVE_WITH_KNOTS ( 'NONE', 5,
 ( #2489, #12077, #22143, #14449, #19164, #23902 ),
 .UNSPECIFIED., .F., .F.,
 ( 6, 6 ),
 ( 66.71879030859999204, 88.69760957229999576 ),
 .UNSPECIFIED. ) ;
#15719 = DIRECTION ( 'NONE',  ( -7.764622278472185525E-13, -0.9341647027306024809, -0.3568421334038978099 ) ) ;
#15720 =( NAMED_UNIT ( * ) SI_UNIT ( $, .STERADIAN. ) SOLID_ANGLE_UNIT ( ) );
#15721 = CARTESIAN_POINT ( 'NONE',  ( 3.843559591276155540, -27.68757158912330496, 8.000000000000007105 ) ) ;
#15722 = CARTESIAN_POINT ( 'NONE',  ( -17.04621913067799710, -27.00000000000000355, -34.17350269210000135 ) ) ;
#15723 = CARTESIAN_POINT ( 'NONE',  ( 22.74701237783497731, -14.17144074696374290, 225.6389823648914330 ) ) ;
#15724 = DIRECTION ( 'NONE',  ( 0.000000000000000000, 0.000000000000000000, 1.000000000000000000 ) ) ;
#15725 = CARTESIAN_POINT ( 'NONE',  ( 0.8260714173989999187, -28.48835664879999996, 224.2403730839999980 ) ) ;
#15726 = ORIENTED_EDGE ( 'NONE', *, *, #15354, .F. ) ;
#15727 = ORIENTED_EDGE ( 'NONE', *, *, #10791, .F. ) ;
#15728 = AXIS2_PLACEMENT_3D ( 'NONE', #17319, #22363, #10398 ) ;
#15729 = AXIS2_PLACEMENT_3D ( 'NONE', #8400, #18000, #27451 ) ;
#15730 = EDGE_CURVE ( 'NONE', #29443, #23376, #16502, .T. ) ;
#15731 = CARTESIAN_POINT ( 'NONE',  ( -1.421085471519999843E-14, -3.552713678799999608E-15, 137.9396849850000137 ) ) ;
#15732 = CARTESIAN_POINT ( 'NONE',  ( 2.620483857039677567, 2.461162703741023527, 230.7813955785624387 ) ) ;
#15733 = ORIENTED_EDGE ( 'NONE', *, *, #5042, .T. ) ;
#15734 = CIRCLE ( 'NONE', #14250, 27.50000000000000000 ) ;
#15735 = FACE_OUTER_BOUND ( 'NONE', #18421, .T. ) ;
#15736 = DIRECTION ( 'NONE',  ( -1.000000000000000000, 4.717926049406357368E-15, -2.251139438558545733E-12 ) ) ;
#15737 = CARTESIAN_POINT ( 'NONE',  ( 1.422193333878468691, -4.930531469442030357, -0.7000165122823585051 ) ) ;
#15738 = VERTEX_POINT ( 'NONE', #27833 ) ;
#15739 = B_SPLINE_CURVE_WITH_KNOTS ( 'NONE', 3,
 ( #3739, #13339, #3900, #20735, #15860, #18202, #8924, #4057, #30336, #27810, #11139 ),
 .UNSPECIFIED., .F., .F.,
 ( 4, 1, 1, 1, 2, 2, 4 ),
 ( 0.000000000000000000, 0.2499999999999913958, 0.3749999999999870659, 0.4374999999999865663, 0.4687499999999862887, 0.4999999999999860112, 1.000000000000000000 ),
 .UNSPECIFIED. ) ;
#15740 = CARTESIAN_POINT ( 'NONE',  ( 0.000000000000000000, 0.000000000000000000, 186.3944487260000074 ) ) ;
#15741 = ORIENTED_EDGE ( 'NONE', *, *, #24537, .T. ) ;
#15742 = ADVANCED_FACE ( 'NONE', ( #3768 ), #4238, .F. ) ;
#15743 = ORIENTED_EDGE ( 'NONE', *, *, #21056, .F. ) ;
#15744 =( NAMED_UNIT ( * ) SI_UNIT ( $, .STERADIAN. ) SOLID_ANGLE_UNIT ( ) );
#15745 = ORIENTED_EDGE ( 'NONE', *, *, #13554, .T. ) ;
#15746 = CARTESIAN_POINT ( 'NONE',  ( 17.83931934289999788, 20.00000000000000000, 230.6999999999999886 ) ) ;
#15747 = ORIENTED_EDGE ( 'NONE', *, *, #23615, .T. ) ;
#15748 = CARTESIAN_POINT ( 'NONE',  ( -24.73474822280000041, -14.15859640590000090, 226.0959706989999916 ) ) ;
#15749 = DIRECTION ( 'NONE',  ( 0.000000000000000000, -1.000000000000000000, 0.000000000000000000 ) ) ;
#15750 = CARTESIAN_POINT ( 'NONE',  ( 3.421672250023957140, 1.629039945493292896, -35.69999999999999574 ) ) ;
#15751 = CARTESIAN_POINT ( 'NONE',  ( -6.982632971260602339, 5.672256964453205264, -40.24571374340602148 ) ) ;
#15752 = FACE_OUTER_BOUND ( 'NONE', #25515, .T. ) ;
#15753 = CARTESIAN_POINT ( 'NONE',  ( 2.411999711991697382, -2.822293950991988432, 227.7677604876778332 ) ) ;
#15754 = CARTESIAN_POINT ( 'NONE',  ( -11.52349576831824507, 26.37260064595716358, -59.27948791363240844 ) ) ;
#15755 = ADVANCED_FACE ( 'NONE', ( #18225 ), #18068, .F. ) ;
#15756 = VECTOR ( 'NONE', #8328, 1000.000000000000114 ) ;
#15757 = ORIENTED_EDGE ( 'NONE', *, *, #9844, .T. ) ;
#15758 = VECTOR ( 'NONE', #23961, 1000.000000000000000 ) ;
#15759 = EDGE_CURVE ( 'NONE', #6473, #10219, #30524, .T. ) ;
#15760 = CARTESIAN_POINT ( 'NONE',  ( 2.816286225276055433, -4.345042730952153320, -1.165939388299997770 ) ) ;
#15761 = CARTESIAN_POINT ( 'NONE',  ( 4.081868536579633222, 3.119100555900671257, -22.42977430109999659 ) ) ;
#15762 = DIRECTION ( 'NONE',  ( 0.000000000000000000, 0.000000000000000000, 1.000000000000000000 ) ) ;
#15763 = FACE_OUTER_BOUND ( 'NONE', #10566, .T. ) ;
#15764 = CARTESIAN_POINT ( 'NONE',  ( -1.609514238130545838, -3.181902231687246285, -88.52261276296684400 ) ) ;
#15765 = CARTESIAN_POINT ( 'NONE',  ( -27.29823224880000154, -2.891194551069999571E-14, 230.6577119970000069 ) ) ;
#15766 = CARTESIAN_POINT ( 'NONE',  ( 17.47295178686619010, 9.934232311478513822, -0.6999999999999785283 ) ) ;
#15767 = CARTESIAN_POINT ( 'NONE',  ( 8.999999999769999093, 20.97450841549535028, -44.83935997348105928 ) ) ;
#15768 = PRODUCT_DEFINITION ( 'UNKNOWN', '', #13345, #23564 ) ;
#15769 = CARTESIAN_POINT ( 'NONE',  ( -17.70100621815563713, 10.30852736142610659, 0.000000000000000000 ) ) ;
#15770 = CARTESIAN_POINT ( 'NONE',  ( 14.29505443750000104, -22.88289997660000097, 230.6999999999999886 ) ) ;
#15771 = CARTESIAN_POINT ( 'NONE',  ( 23.48807013355484585, -14.30280389817958842, 224.0869147245778947 ) ) ;
#15772 = ORIENTED_EDGE ( 'NONE', *, *, #20209, .T. ) ;
#15773 = CARTESIAN_POINT ( 'NONE',  ( -2.158984558600606007, 5.217364672555318883, -56.66652090042499879 ) ) ;
#15774 = CARTESIAN_POINT ( 'NONE',  ( 0.000000000000000000, 0.000000000000000000, 140.0000000000000000 ) ) ;
#15775 = VERTEX_POINT ( 'NONE', #25651 ) ;
#15776 = CARTESIAN_POINT ( 'NONE',  ( -18.95046173579999760, -18.95046173579999760, 86.78285841159998881 ) ) ;
#15777 = EDGE_LOOP ( 'NONE', ( #10252, #25453, #2289, #15801 ) ) ;
#15778 = B_SPLINE_CURVE_WITH_KNOTS ( 'NONE', 3,
 ( #23570, #2004, #17229, #29184, #7631, #10160, #26832, #19603, #29341, #29500, #5429, #5117, #7786, #9848, #7937, #22119, #17388, #3371, #3219, #24940, #24785, #15342, #5285, #26991, #5737, #10319 ),
 .UNSPECIFIED., .F., .F.,
 ( 4, 2, 2, 1, 1, 2, 2, 2, 2, 2, 1, 1, 2, 2, 4 ),
 ( 0.000000000000000000, 0.1249999999999930611, 0.1874999999999903133, 0.2187499999999897304, 0.2343749999999894529, 0.2421874999999900913, 0.2499999999999907296, 0.4999999999999993339, 0.6250000000000036637, 0.6875000000000068834, 0.7187500000000075495, 0.7343750000000088818, 0.7421875000000085487, 0.7500000000000082157, 1.000000000000000000 ),
 .UNSPECIFIED. ) ;
#15779 = CARTESIAN_POINT ( 'NONE',  ( -25.22069443620000229, -13.27363204220000092, 225.2084371580000095 ) ) ;
#15780 = EDGE_CURVE ( 'NONE', #11492, #3101, #23566, .T. ) ;
#15781 = FACE_OUTER_BOUND ( 'NONE', #2137, .T. ) ;
#15782 = CIRCLE ( 'NONE', #27836, 27.23548387080000310 ) ;
#15783 = EDGE_LOOP ( 'NONE', ( #19705, #29747, #13660, #11569, #17140, #26552 ) ) ;
#15784 = CARTESIAN_POINT ( 'NONE',  ( 10.69999999949999925, 19.99999999999999645, -2.302021179699999198 ) ) ;
#15785 = AXIS2_PLACEMENT_3D ( 'NONE', #5127, #6867, #21823 ) ;
#15786 = EDGE_LOOP ( 'NONE', ( #22484, #30182 ) ) ;
#15787 = AXIS2_PLACEMENT_3D ( 'NONE', #28359, #9474, #14202 ) ;
#15788 = ORIENTED_EDGE ( 'NONE', *, *, #29319, .F. ) ;
#15789 = CIRCLE ( 'NONE', #23849, 4.000000004070001225 ) ;
#15790 = VERTEX_POINT ( 'NONE', #1574 ) ;
#15791 = CARTESIAN_POINT ( 'NONE',  ( -12.29999999984293346, -24.44106610432582727, -30.36654950393056396 ) ) ;
#15792 = CARTESIAN_POINT ( 'NONE',  ( 23.24663841807412723, -14.69162354064478571, 4.903540289168272892 ) ) ;
#15793 = CARTESIAN_POINT ( 'NONE',  ( -4.568101251964836074, -0.2431723019727868862, -65.56421022022500722 ) ) ;
#15794 = ADVANCED_FACE ( 'NONE', ( #11161 ), #20757, .F. ) ;
#15795 = CARTESIAN_POINT ( 'NONE',  ( -13.40068078979999910, -26.90685836619999804, 229.9751244090000171 ) ) ;
#15796 = CARTESIAN_POINT ( 'NONE',  ( 0.000000000000000000, -2.000000000000000000, 227.6412452703700069 ) ) ;
#15797 = CARTESIAN_POINT ( 'NONE',  ( 0.000000000000000000, 3.552713678799999608E-15, 43.60555127550000520 ) ) ;
#15798 = EDGE_CURVE ( 'NONE', #1647, #21140, #1124, .T. ) ;
#15799 = CARTESIAN_POINT ( 'NONE',  ( 4.334836395473461224, -2.879286697580460519, -35.69999999999999574 ) ) ;
#15800 = CARTESIAN_POINT ( 'NONE',  ( -28.49999999959999641, -10.47094308429999998, 229.0000000000000000 ) ) ;
#15801 = ORIENTED_EDGE ( 'NONE', *, *, #2965, .F. ) ;
#15802 = CARTESIAN_POINT ( 'NONE',  ( -1.421085471519999843E-14, -1.421085471519999843E-14, 36.39444872449999480 ) ) ;
#15803 = CARTESIAN_POINT ( 'NONE',  ( -4.338779899226326009, -4.343559731693466652, -9.813991631000003935 ) ) ;
#15804 = CARTESIAN_POINT ( 'NONE',  ( 26.79999999930000243, -1.760380630484417619, 0.000000000000000000 ) ) ;
#15805 = ADVANCED_FACE ( 'NONE', ( #1415 ), #10855, .F. ) ;
#15806 = VECTOR ( 'NONE', #16202, 1000.000000000000000 ) ;
#15807 = B_SPLINE_CURVE_WITH_KNOTS ( 'NONE', 3,
 ( #15316, #24457, #555, #26967, #3194, #22406 ),
 .UNSPECIFIED., .F., .F.,
 ( 4, 2, 4 ),
 ( 0.000000000000000000, 0.5000000000000000000, 1.000000000000000000 ),
 .UNSPECIFIED. ) ;
#15808 = CARTESIAN_POINT ( 'NONE',  ( 14.85086212533918548, -29.59541620749952884, -32.67503844573987237 ) ) ;
#15809 = ORIENTED_EDGE ( 'NONE', *, *, #6584, .F. ) ;
#15810 = CARTESIAN_POINT ( 'NONE',  ( 25.22036945370000183, -13.27344566769999901, 224.7916409239999780 ) ) ;
#15811 = CARTESIAN_POINT ( 'NONE',  ( -24.61381496323305740, -14.36755986783201777, 6.042472825000033687 ) ) ;
#15812 = CIRCLE ( 'NONE', #27375, 27.50000000000000000 ) ;
#15813 = PRODUCT_DEFINITION ( 'UNKNOWN', '', #20381, #17836 ) ;
#15814 = DIRECTION ( 'NONE',  ( -3.924189347185962345E-12, 0.4082287037029531107, 0.9128796883888953273 ) ) ;
#15815 = CIRCLE ( 'NONE', #20829, 27.92857142840000151 ) ;
#15816 = CARTESIAN_POINT ( 'NONE',  ( 26.93696268452646336, 0.4901285798019155981, 0.000000000000000000 ) ) ;
#15817 = VECTOR ( 'NONE', #6596, 1000.000000000000000 ) ;
#15818 = LINE ( 'NONE', #3856, #13523 ) ;
#15819 = CARTESIAN_POINT ( 'NONE',  ( 3.630871288588910506, -4.685987307826644965, -52.50430438132499944 ) ) ;
#15820 = CARTESIAN_POINT ( 'NONE',  ( -11.59065746630000149, -24.20066399839999960, -1.404983722500002807 ) ) ;
#15821 = CARTESIAN_POINT ( 'NONE',  ( 27.50000000000000000, -3.367667472999999580E-15, 143.6055512739999926 ) ) ;
#15822 = ORIENTED_EDGE ( 'NONE', *, *, #18704, .F. ) ;
#15823 = CARTESIAN_POINT ( 'NONE',  ( 24.90302311548996883, -13.86047864964742793, 3.901342110999989288 ) ) ;
#15824 = DIRECTION ( 'NONE',  ( 0.3633921898465272138, -0.9316362575375356503, 0.000000000000000000 ) ) ;
#15825 = APPLICATION_CONTEXT ( 'automotive_design' ) ;
#15826 = CARTESIAN_POINT ( 'NONE',  ( 1.704635467467862764, -3.764872627205382738, -68.10000000002499121 ) ) ;
#15827 = EDGE_CURVE ( 'NONE', #24348, #27161, #29656, .T. ) ;
#15828 = VECTOR ( 'NONE', #26525, 1000.000000000000000 ) ;
#15829 = CARTESIAN_POINT ( 'NONE',  ( -16.83342759559999635, -9.000000000000001776, -1.399999999999998579 ) ) ;
#15830 = CARTESIAN_POINT ( 'NONE',  ( -3.764950641351794136, -1.323627178738328913, -44.10000000002499121 ) ) ;
#15831 = EDGE_CURVE ( 'NONE', #28749, #11807, #13896, .T. ) ;
#15832 = DIRECTION ( 'NONE',  ( 0.000000000000000000, -1.000000000000000000, 0.000000000000000000 ) ) ;
#15833 = CARTESIAN_POINT ( 'NONE',  ( 3.071220613210755346, 1.663153190280735494, -41.62814900322526768 ) ) ;
#15834 = CARTESIAN_POINT ( 'NONE',  ( 1.415268835070086828, -5.780081730205603563, -65.18397119102500881 ) ) ;
#15835 = VECTOR ( 'NONE', #23299, 1000.000000000000114 ) ;
#15836 = VERTEX_POINT ( 'NONE', #26261 ) ;
#15837 = EDGE_CURVE ( 'NONE', #10676, #16947, #15997, .T. ) ;
#15838 = CARTESIAN_POINT ( 'NONE',  ( -16.83342759582943060, -8.999999999996580513, -0.6999999999999784173 ) ) ;
#15839 = ORIENTED_EDGE ( 'NONE', *, *, #11985, .T. ) ;
#15840 = CARTESIAN_POINT ( 'NONE',  ( -19.56389390649999882, 19.56881929660000097, 229.4993219170000032 ) ) ;
#15841 = ORIENTED_EDGE ( 'NONE', *, *, #18887, .T. ) ;
#15842 = CARTESIAN_POINT ( 'NONE',  ( 24.07552037900000030, -13.90000980950000020, 226.1000014189999945 ) ) ;
#15843 = LINE ( 'NONE', #25605, #8005 ) ;
#15844 = CARTESIAN_POINT ( 'NONE',  ( 3.686970300939999667, 0.4978338539504151838, -70.82548838946271985 ) ) ;
#15845 = CARTESIAN_POINT ( 'NONE',  ( -25.52817993772956484, 13.14824702356417241, 8.000000000000007105 ) ) ;
#15846 = CARTESIAN_POINT ( 'NONE',  ( -24.12025211354654886, 13.88308537690706324, 8.000000000000007105 ) ) ;
#15847 = CARTESIAN_POINT ( 'NONE',  ( -12.41750254861463354, -21.99999999999999289, -27.00106416659522779 ) ) ;
#15848 = VECTOR ( 'NONE', #20329, 1000.000000000000000 ) ;
#15849 = CARTESIAN_POINT ( 'NONE',  ( 8.999999999770000869, 21.70000000000000284, -58.10000000000000142 ) ) ;
#15850 = ORIENTED_EDGE ( 'NONE', *, *, #1052, .F. ) ;
#15851 = CARTESIAN_POINT ( 'NONE',  ( 4.785280386532176244, 31.71089591181006639, 8.000000000000007105 ) ) ;
#15852 = DIRECTION ( 'NONE',  ( -1.224606353819999829E-16, -1.000000000000000000, 0.000000000000000000 ) ) ;
#15853 = DIRECTION ( 'NONE',  ( 2.764840495839172918E-12, 0.9128796883888953273, -0.4082287037029531107 ) ) ;
#15854 = CARTESIAN_POINT ( 'NONE',  ( 8.700000000284820345, -13.66682223737197610, -36.55330428411850363 ) ) ;
#15855 = CARTESIAN_POINT ( 'NONE',  ( -24.48873108229999929, -14.58042505439999914, 226.0425106499999970 ) ) ;
#15856 = DIRECTION ( 'NONE',  ( 0.000000000000000000, 0.000000000000000000, 1.000000000000000000 ) ) ;
#15857 = CARTESIAN_POINT ( 'NONE',  ( -7.707106507371444870, -5.692566414263196428, -27.29492500646317765 ) ) ;
#15858 = CARTESIAN_POINT ( 'NONE',  ( -15.86808677770000209, 10.47263190749999495, -1.399999999599998990 ) ) ;
#15859 = CARTESIAN_POINT ( 'NONE',  ( 5.943504367937093136, -0.4395870339238064362, -48.64442242802499550 ) ) ;
#15860 = CARTESIAN_POINT ( 'NONE',  ( 14.78339330455186662, -23.57315723864463308, -24.60498589874045194 ) ) ;
#15861 = CARTESIAN_POINT ( 'NONE',  ( 14.74534393132121579, -28.33174258796800871, -33.40462800574894686 ) ) ;
#15862 = CYLINDRICAL_SURFACE ( 'NONE', #22351, 3.500000000000000444 ) ;
#15863 = EDGE_CURVE ( 'NONE', #23914, #11684, #7217, .T. ) ;
#15864 = LINE ( 'NONE', #25631, #30839 ) ;
#15865 = B_SPLINE_CURVE_WITH_KNOTS ( 'NONE', 1,
 ( #25920, #4194 ),
 .UNSPECIFIED., .F., .F.,
 ( 2, 2 ),
 ( -2.555864960449999711E-06, 0.7000000000009999335 ),
 .UNSPECIFIED. ) ;
#15866 = VERTEX_POINT ( 'NONE', #9578 ) ;
#15867 = ADVANCED_FACE ( 'NONE', ( #18863 ), #28926, .F. ) ;
#15868 = CARTESIAN_POINT ( 'NONE',  ( 4.904813032679735230, 3.691647504909488564, -32.96032172560001072 ) ) ;
#15869 = EDGE_CURVE ( 'NONE', #7509, #12603, #21542, .T. ) ;
#15870 = ORIENTED_EDGE ( 'NONE', *, *, #11600, .T. ) ;
#15871 = CARTESIAN_POINT ( 'NONE',  ( -3.735326252960651239, -2.773461810559843421, -57.02895058492501335 ) ) ;
#15872 = ORIENTED_EDGE ( 'NONE', *, *, #10942, .T. ) ;
#15873 = APPLICATION_PROTOCOL_DEFINITION ( 'draft international standard', 'automotive_design', 1998, #4757 ) ;
#15874 = ORIENTED_EDGE ( 'NONE', *, *, #22076, .F. ) ;
#15875 = ORIENTED_EDGE ( 'NONE', *, *, #21123, .F. ) ;
#15876 = CARTESIAN_POINT ( 'NONE',  ( 8.000000000115440102, -60.75400889061143772, -3.446705952627092895 ) ) ;
#15877 = DIRECTION ( 'NONE',  ( 1.486658018913458559E-12, 0.9128796883888955493, -0.4082287037029524446 ) ) ;
#15878 = CARTESIAN_POINT ( 'NONE',  ( 4.638687372290002386, 3.765626869285956690, -39.31578811165251608 ) ) ;
#15879 = B_SPLINE_CURVE_WITH_KNOTS ( 'NONE', 3,
 ( #27886, #28350, #18747, #25998, #13882, #18277 ),
 .UNSPECIFIED., .F., .F.,
 ( 4, 2, 4 ),
 ( 0.000000000000000000, 0.5000000000000000000, 1.000000000000000000 ),
 .UNSPECIFIED. ) ;
#15880 = CYLINDRICAL_SURFACE ( 'NONE', #8399, 7.999999999999998224 ) ;
#15881 = DIRECTION ( 'NONE',  ( 0.3633921898465291567, 0.9316362575375348731, 0.000000000000000000 ) ) ;
#15882 = DIRECTION ( 'NONE',  ( 0.9915824307782121760, -0.1294769592320275942, 0.000000000000000000 ) ) ;
#15883 = CARTESIAN_POINT ( 'NONE',  ( -3.175770273322759518, 4.553269643686719270, -0.6276513541000027230 ) ) ;
#15884 = CARTESIAN_POINT ( 'NONE',  ( 1.226419552955990477, -1.601210460385421808, 230.8412452700000301 ) ) ;
#15885 = CARTESIAN_POINT ( 'NONE',  ( -0.6731456008920000400, -3.434453875705480108, -72.25672407562892374 ) ) ;
#15886 = CARTESIAN_POINT ( 'NONE',  ( 1.757687669117797835, -5.210066540036287996, -16.26414732020001352 ) ) ;
#15887 = CARTESIAN_POINT ( 'NONE',  ( -3.500772897184941446, -3.093025330206539802, -33.33447003410001486 ) ) ;
#15888 = FACE_OUTER_BOUND ( 'NONE', #3977, .T. ) ;
#15889 = CARTESIAN_POINT ( 'NONE',  ( 10.00000000000000000, -130.0000000000000000, -42.39999999999999858 ) ) ;
#15890 = CARTESIAN_POINT ( 'NONE',  ( 0.06886553588169999629, -27.80016486610000115, 223.9013487590000011 ) ) ;
#15891 = CARTESIAN_POINT ( 'NONE',  ( 15.33917451568712842, -24.20553497015958300, 8.000000000000007105 ) ) ;
#15892 = CARTESIAN_POINT ( 'NONE',  ( -19.80535357377644701, 19.50875577052588739, 0.9999999989999952543 ) ) ;
#15893 = EDGE_CURVE ( 'NONE', #7025, #2249, #27047, .T. ) ;
#15894 = CARTESIAN_POINT ( 'NONE',  ( 22.11577621125299586, 17.85147953289403944, -0.2432540810000105580 ) ) ;
#15895 = CARTESIAN_POINT ( 'NONE',  ( 8.000000000859367688, -29.57832802809286932, -26.81682687350731342 ) ) ;
#15896 = CARTESIAN_POINT ( 'NONE',  ( 8.700000000236576270, -29.80249410823907752, -29.47052640017699687 ) ) ;
#15897 = ORIENTED_EDGE ( 'NONE', *, *, #6513, .T. ) ;
#15898 = CARTESIAN_POINT ( 'NONE',  ( 2.215775945524685486, 3.162163484153768689, 230.6362108339230588 ) ) ;
#15899 = VERTEX_POINT ( 'NONE', #11784 ) ;
#15900 = CARTESIAN_POINT ( 'NONE',  ( -22.74701237787062169, -14.17144074690075328, 224.3610176349945391 ) ) ;
#15901 = CARTESIAN_POINT ( 'NONE',  ( 2.011424923818943888, -2.537138457451959539, -36.24172406371944533 ) ) ;
#15902 = CARTESIAN_POINT ( 'NONE',  ( 12.80098767942999771, -22.00000000000000000, -25.51324865327000069 ) ) ;
#15903 = VERTEX_POINT ( 'NONE', #19334 ) ;
#15904 = CARTESIAN_POINT ( 'NONE',  ( 3.915051063684143795, -2.600456723069958453, -44.15875473022499875 ) ) ;
#15905 = ORIENTED_EDGE ( 'NONE', *, *, #15191, .F. ) ;
#15906 = ORIENTED_EDGE ( 'NONE', *, *, #9079, .T. ) ;
#15907 = ORIENTED_EDGE ( 'NONE', *, *, #29880, .T. ) ;
#15908 = CARTESIAN_POINT ( 'NONE',  ( 18.87722420200000073, 21.16361474609999860, 229.7625741969999922 ) ) ;
#15909 = ORIENTED_EDGE ( 'NONE', *, *, #12189, .F. ) ;
#15910 = CARTESIAN_POINT ( 'NONE',  ( 7.908773014210000341, 16.35323874420000223, 230.6999999999999886 ) ) ;
#15911 = CARTESIAN_POINT ( 'NONE',  ( 0.000000000000000000, 3.552713678799999608E-15, 193.2171415880000040 ) ) ;
#15912 = CARTESIAN_POINT ( 'NONE',  ( 0.2722179827847738820, -28.49915599490020668, 3.920205022000022854 ) ) ;
#15913 = CARTESIAN_POINT ( 'NONE',  ( 14.84798480953660338, -22.00000000000000355, -28.62014973081917191 ) ) ;
#15914 = CARTESIAN_POINT ( 'NONE',  ( -10.69999999999999929, -30.00000000000000000, -28.40000000000000213 ) ) ;
#15915 = CARTESIAN_POINT ( 'NONE',  ( 23.84773733367773829, -14.28804811815363962, 4.437381894575493924 ) ) ;
#15916 = ADVANCED_FACE ( 'NONE', ( #16805 ), #12240, .T. ) ;
#15917 = VERTEX_POINT ( 'NONE', #4861 ) ;
#15918 = EDGE_CURVE ( 'NONE', #13159, #15501, #14462, .T. ) ;
#15919 = CARTESIAN_POINT ( 'NONE',  ( 1.334940606749785319, 4.973974987606708531, -2.990910702900007934 ) ) ;
#15920 = CARTESIAN_POINT ( 'NONE',  ( 3.375516224911109031, -2.766870103071180420, -23.49674734059999892 ) ) ;
#15921 = CARTESIAN_POINT ( 'NONE',  ( 24.50000001620000134, -3.000285568839999855E-15, 190.0000000039999861 ) ) ;
#15922 = CARTESIAN_POINT ( 'NONE',  ( 24.70448873180906446, -12.74983733560190302, 5.760266709000011254 ) ) ;
#15923 = CARTESIAN_POINT ( 'NONE',  ( 3.387276893882220641, -0.9936988735501727232, -91.06246442329681656 ) ) ;
#15924 = CARTESIAN_POINT ( 'NONE',  ( -1.650600432523903427, 3.499825479287930641, 227.8575818780827262 ) ) ;
#15925 = CARTESIAN_POINT ( 'NONE',  ( 9.897162125400441823, -25.37356426577149193, 38.33953982530000104 ) ) ;
#15926 = CARTESIAN_POINT ( 'NONE',  ( -1.100000000000000089, -26.77741585740000119, 5.000000000000000000 ) ) ;
#15927 = EDGE_CURVE ( 'NONE', #3457, #5941, #15005, .T. ) ;
#15928 = VECTOR ( 'NONE', #26060, 1000.000000000000227 ) ;
#15929 = CARTESIAN_POINT ( 'NONE',  ( -27.79999999970000246, -10.21376199200000201, 222.0000000000000000 ) ) ;
#15930 = CARTESIAN_POINT ( 'NONE',  ( 8.621538427680000893, 16.00851259929999770, 230.6999999999999886 ) ) ;
#15931 = CARTESIAN_POINT ( 'NONE',  ( -10.00000000049220006, -25.12044511663835422, -9.805662262113871819 ) ) ;
#15932 = VERTEX_POINT ( 'NONE', #27478 ) ;
#15933 = CARTESIAN_POINT ( 'NONE',  ( 4.831710525212951524, -2.520823095555479565, -60.51790713612500383 ) ) ;
#15934 = FACE_OUTER_BOUND ( 'NONE', #2975, .T. ) ;
#15935 = ORIENTED_EDGE ( 'NONE', *, *, #10016, .T. ) ;
#15936 = DIRECTION ( 'NONE',  ( -9.219194983962475343E-13, -0.9128796883888954383, 0.4082287037029530552 ) ) ;
#15937 = ORIENTED_EDGE ( 'NONE', *, *, #14557, .F. ) ;
#15938 = CARTESIAN_POINT ( 'NONE',  ( -26.80000000000000071, 1.776356839399999804E-15, -2.842170943039999687E-14 ) ) ;
#15939 = CARTESIAN_POINT ( 'NONE',  ( 26.80000000000001492, -1.754055898254314183, 186.7828584119999960 ) ) ;
#15940 = ORIENTED_EDGE ( 'NONE', *, *, #20994, .T. ) ;
#15941 = EDGE_CURVE ( 'NONE', #23024, #19165, #5925, .T. ) ;
#15942 = ORIENTED_EDGE ( 'NONE', *, *, #14693, .T. ) ;
#15943 = EDGE_LOOP ( 'NONE', ( #23707, #3484, #25398, #11273 ) ) ;
#15944 = CARTESIAN_POINT ( 'NONE',  ( -20.19076655603533510, -17.71015691556365468, 186.7828584120833284 ) ) ;
#15945 = FILL_AREA_STYLE ('',( #6348 ) ) ;
#15946 =( BOUNDED_CURVE ( )  B_SPLINE_CURVE ( 5, ( #13413, #25391, #18289, #10595, #30100, #22707, #6178, #8211, #8528, #1474, #6021, #853, #18129, #8685, #29940, #25545, #29781, #17964, #15466, #3981, #20038, #1151, #27576, #25069, #15619, #25226, #11065, #5709, #27731, #20662, #3827, #17659, #3656, #13578, #10743, #23029, #30257, #12953, #22563, #27272, #29635, #20344, #8368, #27422, #17814, #5860, #13253, #3502, #22871, #1313, #27896, #10908, #1007, #20500, #8064, #6340, #10444, #20189, #16700, #31037, #18451, #9475, #9156, #11378, #23184, #18759, #21440, #7115, #18917, #11218, #1627, #6646, #23345, #6807, #30428, #19076, #4453, #28360, #20974, #28049, #1788, #30886, #2092, #6492, #26317, #28671, #16093, #28516, #8845, #14053, #16403, #16244, #4763, #25861, #26162, #4299, #18607, #20818, #13894, #25705, #23657, #6962, #26010, #4135, #21133, #30580, #13734, #9006 ),
 .UNSPECIFIED., .F., .T. ) 
 B_SPLINE_CURVE_WITH_KNOTS ( ( 6, 3, 3, 3, 3, 3, 3, 3, 3, 3, 3, 3, 3, 3, 3, 3, 3, 3, 3, 3, 3, 3, 3, 3, 3, 3, 3, 3, 3, 3, 3, 3, 3, 3, 3, 6 ),
 ( 8.193316113699999903, 11.38862009670000042, 23.17260734259999921, 34.79167593860000096, 46.25425528950000142, 57.87229377410000097, 69.67120816000000616, 81.20502170430000888, 92.80704244430000927, 104.1208912060000102, 115.9269080290000034, 127.3307717769999954, 139.1306782750000082, 150.7654282180000109, 162.2434640489999822, 173.6637378899999931, 185.2020570420000070, 194.1769840820000184, 203.3038760180000111, 212.5853790139999830, 224.1393301890000203, 235.6932813649999900, 246.8715721780000081, 258.4996770380000157, 270.1277818960000445, 281.7035649139999691, 293.2822232819999613, 304.6732510989999696, 316.1434960830000023, 327.6894369340000139, 339.2353777880000507, 350.7813186390000055, 362.5843219139999860, 374.0573691040000313, 385.8560256169999434, 394.7457478480000077 ),
 .UNSPECIFIED. ) 
 CURVE ( )  GEOMETRIC_REPRESENTATION_ITEM ( )  RATIONAL_B_SPLINE_CURVE ( ( 0.2500000000000000000, 0.2500000000000000000, 0.2500000000000000000, 0.2500000000000000000, 0.2500000000000000000, 0.2500000000000000000, 0.2500000000000000000, 0.2500000000000000000, 0.2500000000000000000, 0.2500000000000000000, 0.2500000000000000000, 0.2500000000000000000, 0.2500000000000000000, 0.2500000000000000000, 0.2500000000000000000, 0.2500000000000000000, 0.2500000000000000000, 0.2500000000000000000, 0.2500000000000000000, 0.2500000000000000000, 0.2500000000000000000, 0.2500000000000000000, 0.2500000000000000000, 0.2500000000000000000, 0.2500000000000000000, 0.2500000000000000000, 0.2500000000000000000, 0.2500000000000000000, 0.2500000000000000000, 0.2500000000000000000, 0.2500000000000000000, 0.2500000000000000000, 0.2500000000000000000, 0.2500000000000000000, 0.2500000000000000000, 0.2500000000000000000, 0.2500000000000000000, 0.2500000000000000000, 0.2500000000000000000, 0.2500000000000000000, 0.2500000000000000000, 0.2500000000000000000, 0.2500000000000000000, 0.2500000000000000000, 0.2500000000000000000, 0.2500000000000000000, 0.2500000000000000000, 0.2500000000000000000, 0.2500000000000000000, 0.2500000000000000000, 0.2500000000000000000, 0.2500000000000000000, 0.2500000000000000000, 0.2500000000000000000, 0.2500000000000000000, 0.2500000000000000000, 0.2500000000000000000, 0.2500000000000000000, 0.2500000000000000000, 0.2500000000000000000, 0.2500000000000000000, 0.2500000000000000000, 0.2500000000000000000, 0.2500000000000000000, 0.2500000000000000000, 0.2500000000000000000, 0.2500000000000000000, 0.2500000000000000000, 0.2500000000000000000, 0.2500000000000000000, 0.2500000000000000000, 0.2500000000000000000, 0.2500000000000000000, 0.2500000000000000000, 0.2500000000000000000, 0.2500000000000000000, 0.2500000000000000000, 0.2500000000000000000, 0.2500000000000000000, 0.2500000000000000000, 0.2500000000000000000, 0.2500000000000000000, 0.2500000000000000000, 0.2500000000000000000, 0.2500000000000000000, 0.2500000000000000000, 0.2500000000000000000, 0.2500000000000000000, 0.2500000000000000000, 0.2500000000000000000, 0.2500000000000000000, 0.2500000000000000000, 0.2500000000000000000, 0.2500000000000000000, 0.2500000000000000000, 0.2500000000000000000, 0.2500000000000000000, 0.2500000000000000000, 0.2500000000000000000, 0.2500000000000000000, 0.2500000000000000000, 0.2500000000000000000, 0.2500000000000000000, 0.2500000000000000000, 0.2500000000000000000, 0.2500000000000000000, 0.2500000000000000000, 0.2500000000000000000 ) ) 
 REPRESENTATION_ITEM ( '' )  );
#15947 = VERTEX_POINT ( 'NONE', #1375 ) ;
#15948 = CARTESIAN_POINT ( 'NONE',  ( -9.738910687886855655, -24.96785170200598714, 115.0000000000000000 ) ) ;
#15949 = ADVANCED_FACE ( 'NONE', ( #21043 ), #6554, .T. ) ;
#15950 = CARTESIAN_POINT ( 'NONE',  ( 1.290548111051992519, -1.679300369702346085, 226.6412452697800006 ) ) ;
#15951 = CARTESIAN_POINT ( 'NONE',  ( -4.287590041606510916, 1.413705153860731034, -68.74019511502500279 ) ) ;
#15952 = CARTESIAN_POINT ( 'NONE',  ( 27.77512470430000135, 2.244249230899999945E-11, 229.2930777930000090 ) ) ;
#15953 = AXIS2_PLACEMENT_3D ( 'NONE', #25363, #28022, #6467 ) ;
#15954 = AXIS2_PLACEMENT_3D ( 'NONE', #25918, #8909, #28113 ) ;
#15955 = CARTESIAN_POINT ( 'NONE',  ( -17.99933668381276775, 20.17941515429619415, -0.6999999999999784173 ) ) ;
#15956 = CARTESIAN_POINT ( 'NONE',  ( -14.89627966379999968, -24.48058516850000288, 222.0000000000000000 ) ) ;
#15957 = CARTESIAN_POINT ( 'NONE',  ( 4.586950623478608158, -2.526155056066153648, -35.69999999999999574 ) ) ;
#15958 = CARTESIAN_POINT ( 'NONE',  ( -24.98823330661245379, 13.70626928206978690, 3.904029301000005781 ) ) ;
#15959 = PRODUCT_DEFINITION_CONTEXT ( 'detailed design', #6577, 'design' ) ;
#15960 = CARTESIAN_POINT ( 'NONE',  ( 1.086829820489895848, 5.988658659452708477, -14.02400681850000197 ) ) ;
#15961 = CARTESIAN_POINT ( 'NONE',  ( 20.19076655603537418, -17.71015691556361205, 136.7828584120000244 ) ) ;
#15962 = CARTESIAN_POINT ( 'NONE',  ( -28.49528339128749366, -0.5184828350247804307, 0.7595836940000044724 ) ) ;
#15963 = VERTEX_POINT ( 'NONE', #8279 ) ;
#15964 = DIRECTION ( 'NONE',  ( -1.000000000000000000, 5.687697999151106851E-16, -6.771501495036750356E-12 ) ) ;
#15965 = DIRECTION ( 'NONE',  ( 0.000000000000000000, -2.257145581549999994E-12, -1.000000000000000000 ) ) ;
#15966 = CARTESIAN_POINT ( 'NONE',  ( 8.903108651239925564, -22.82508830966962421, 190.0000000000000000 ) ) ;
#15967 = EDGE_CURVE ( 'NONE', #21131, #29406, #22767, .T. ) ;
#15968 = CARTESIAN_POINT ( 'NONE',  ( 27.00728089375858687, 4.961773542941180004, 0.02487529600000981667 ) ) ;
#15969 = CARTESIAN_POINT ( 'NONE',  ( -23.47117976039525189, -14.33053685688857826, 4.119508997195603150 ) ) ;
#15970 = CARTESIAN_POINT ( 'NONE',  ( -4.175165894169885483, -50.49316738903675628, -63.39999999999999858 ) ) ;
#15971 = CARTESIAN_POINT ( 'NONE',  ( 23.73992238019999945, -12.43607998449999918, 225.0000000000000000 ) ) ;
#15972 = CARTESIAN_POINT ( 'NONE',  ( 8.903108651239925564, -22.82508830966962421, 40.00000000000000000 ) ) ;
#15973 = ORIENTED_EDGE ( 'NONE', *, *, #12854, .T. ) ;
#15974 = CARTESIAN_POINT ( 'NONE',  ( 24.00289804085882039, -14.02635914341071732, 4.098597479000015475 ) ) ;
#15975 = CARTESIAN_POINT ( 'NONE',  ( 9.000000000029999114, 21.70000000000000284, -64.10000000000000853 ) ) ;
#15976 = CIRCLE ( 'NONE', #27527, 1.656072167390155281 ) ;
#15977 = CARTESIAN_POINT ( 'NONE',  ( 2.708282711769271156, -3.449188895666643884, -68.10000000002501963 ) ) ;
#15978 = ADVANCED_FACE ( 'NONE', ( #10970, #25130 ), #5363, .F. ) ;
#15979 = EDGE_CURVE ( 'NONE', #11115, #24784, #3726, .T. ) ;
#15980 = DIRECTION ( 'NONE',  ( -0.6941258031311203780, -0.7198537139083029945, 0.000000000000000000 ) ) ;
#15981 = CARTESIAN_POINT ( 'NONE',  ( -4.246760801282904119, 0.8971541554341054825, -44.10000000002499121 ) ) ;
#15982 = CARTESIAN_POINT ( 'NONE',  ( 14.75521759265608424, -23.38921439669723057, -32.08852866628550515 ) ) ;
#15983 = CARTESIAN_POINT ( 'NONE',  ( 0.000000000000000000, -55.00000000000000000, -43.39999999999999858 ) ) ;
#15984 = CARTESIAN_POINT ( 'NONE',  ( -1.313688977135577529, 5.115945099120181361, -66.95876360972499697 ) ) ;
#15985 = ORIENTED_EDGE ( 'NONE', *, *, #28751, .T. ) ;
#15986 = DIRECTION ( 'NONE',  ( 1.000000000000000000, -1.224606353819999829E-16, 0.000000000000000000 ) ) ;
#15987 = ADVANCED_FACE ( 'NONE', ( #20891 ), #8756, .T. ) ;
#15988 = VERTEX_POINT ( 'NONE', #16002 ) ;
#15989 = CARTESIAN_POINT ( 'NONE',  ( -27.79539923781770483, -0.5057481688778047157, 1.000000000000000888 ) ) ;
#15990 = VERTEX_POINT ( 'NONE', #25613 ) ;
#15991 = CARTESIAN_POINT ( 'NONE',  ( 23.83740787290000185, -14.30495753649999990, 226.0027499809999938 ) ) ;
#15992 = CARTESIAN_POINT ( 'NONE',  ( 10.69999999999999929, -27.00000000000000000, -28.40000000000000213 ) ) ;
#15993 = CYLINDRICAL_SURFACE ( 'NONE', #7474, 2.999999999999998668 ) ;
#15994 = CARTESIAN_POINT ( 'NONE',  ( -4.041451884379999804, 9.156941871420000667E-11, 230.5235986622430175 ) ) ;
#15995 = CIRCLE ( 'NONE', #13473, 4.000000004070001225 ) ;
#15996 = CARTESIAN_POINT ( 'NONE',  ( 0.2722179827847738820, -28.49915599490020668, 3.920205022000022854 ) ) ;
#15998 = ADVANCED_FACE ( 'NONE', ( #13642, #23246, #1687, #11287, #16151, #30490 ), #8912, .T. ) ;
#15997 = CIRCLE ( 'NONE', #3426, 2.100000000000000089 ) ;
#15999 = CARTESIAN_POINT ( 'NONE',  ( -16.04158896040112126, -9.763537949678049443, 0.000000000000000000 ) ) ;
#16000 = DIRECTION ( 'NONE',  ( 0.000000000000000000, 0.3420201433259318913, -0.9396926207858126157 ) ) ;
#16001 = ORIENTED_EDGE ( 'NONE', *, *, #3481, .T. ) ;
#16002 = CARTESIAN_POINT ( 'NONE',  ( 8.700000000289733748, -15.05693637256081097, -37.86809127166881694 ) ) ;
#16003 = CARTESIAN_POINT ( 'NONE',  ( -27.50000000000000000, 3.367667473009999970E-15, 115.0000000000000000 ) ) ;
#16004 = DIRECTION ( 'NONE',  ( -1.000000000000000000, 0.000000000000000000, 0.000000000000000000 ) ) ;
#16005 = FACE_OUTER_BOUND ( 'NONE', #27982, .T. ) ;
#16006 = CARTESIAN_POINT ( 'NONE',  ( 23.25801811797813556, -13.31593093537183492, 3.899999999996501820 ) ) ;
#16007 = CARTESIAN_POINT ( 'NONE',  ( 0.000000000000000000, 0.000000000000000000, 90.00000000000000000 ) ) ;
#16008 = CARTESIAN_POINT ( 'NONE',  ( 23.31033037370282202, 15.14834847481879265, 4.441258569420641678 ) ) ;
#16009 = CARTESIAN_POINT ( 'NONE',  ( -17.48715850607838007, 10.10369150396071625, -1.400000000000001910 ) ) ;
#16010 = CARTESIAN_POINT ( 'NONE',  ( 1.321824945545741814, 4.319062652178985218, -51.06125421262500197 ) ) ;
#16011 = EDGE_CURVE ( 'NONE', #30396, #30479, #21039, .T. ) ;
#16012 = DIRECTION ( 'NONE',  ( 0.000000000000000000, 0.000000000000000000, 1.000000000000000000 ) ) ;
#16013 = CARTESIAN_POINT ( 'NONE',  ( 14.83413420727321963, -29.02780189700713365, -33.00248536946025979 ) ) ;
#16014 = CARTESIAN_POINT ( 'NONE',  ( 3.465040867608843556, -0.9980531523770136415, 230.7751077600194094 ) ) ;
#16015 = CARTESIAN_POINT ( 'NONE',  ( -6.000000000000000000, -23.16799891216055940, -79.43914708545641190 ) ) ;
#16016 = ORIENTED_EDGE ( 'NONE', *, *, #284, .F. ) ;
#16017 = CARTESIAN_POINT ( 'NONE',  ( 10.69999999999999929, -27.00000000000000000, -31.39999999999999858 ) ) ;
#16018 = VECTOR ( 'NONE', #17504, 1000.000000000000114 ) ;
#16019 = ORIENTED_EDGE ( 'NONE', *, *, #9840, .T. ) ;
#16020 = CARTESIAN_POINT ( 'NONE',  ( 0.7746255519259798161, 4.866335056765463740, -55.16500058692498953 ) ) ;
#16021 = ORIENTED_EDGE ( 'NONE', *, *, #15979, .F. ) ;
#16022 = PRODUCT_CONTEXT ( 'NONE', #20224, 'mechanical' ) ;
#16023 = EDGE_LOOP ( 'NONE', ( #28172, #28951, #16364, #18530 ) ) ;
#16024 = ORIENTED_EDGE ( 'NONE', *, *, #1150, .F. ) ;
#16025 = CARTESIAN_POINT ( 'NONE',  ( 14.84835410051194948, -29.11010934775363523, -23.84443905029603172 ) ) ;
#16026 = CARTESIAN_POINT ( 'NONE',  ( 5.288280169994311386, -9.335552363041854207, -36.26372187282946413 ) ) ;
#16027 = CARTESIAN_POINT ( 'NONE',  ( -17.22797207741495029, -27.58333898473983581, -22.96328822816851201 ) ) ;
#16028 = VECTOR ( 'NONE', #26220, 999.9999999999998863 ) ;
#16029 = CARTESIAN_POINT ( 'NONE',  ( 5.445859840630000726, -10.81896303589999953, 231.9999991140000191 ) ) ;
#16030 = DIRECTION ( 'NONE',  ( -3.924189347185961537E-12, 0.4082287037029530552, 0.9128796883888952163 ) ) ;
#16031 = ADVANCED_FACE ( 'NONE', ( #18823 ), #11489, .T. ) ;
#16032 = CARTESIAN_POINT ( 'NONE',  ( -17.62526668104891314, 11.76353838341477953, 0.000000000000000000 ) ) ;
#16033 = CARTESIAN_POINT ( 'NONE',  ( -2.507187057889202819, 3.594686560818132204, -1.127651354099999725 ) ) ;
#16034 = DIRECTION ( 'NONE',  ( 0.000000000000000000, 0.000000000000000000, 1.000000000000000000 ) ) ;
#16035 = CARTESIAN_POINT ( 'NONE',  ( -10.69999999999999929, -27.00000000000000000, -28.40000000000000213 ) ) ;
#16036 = ADVANCED_FACE ( 'NONE', ( #12055 ), #24022, .F. ) ;
#16037 = CARTESIAN_POINT ( 'NONE',  ( 4.630235822890134578, 0.3309221515414850767, -14.64454535870000207 ) ) ;
#16038 = CARTESIAN_POINT ( 'NONE',  ( -2.100000000000000089, 2.220446049249999755E-16, 227.6412452697800006 ) ) ;
#16039 = AXIS2_PLACEMENT_3D ( 'NONE', #414, #22112, #17220 ) ;
#16040 = EDGE_CURVE ( 'NONE', #11379, #1647, #4137, .T. ) ;
#16041 = EDGE_CURVE ( 'NONE', #16579, #17696, #30790, .T. ) ;
#16042 = CONICAL_SURFACE ( 'NONE', #21583, 1.303225372841142260, 0.9162978572969998625 ) ;
#16043 = PLANE ( 'NONE',  #19751 ) ;
#16044 = CARTESIAN_POINT ( 'NONE',  ( -0.4946807661028205794, -26.79522487538596565, 5.993195172251796876 ) ) ;
#16045 = CARTESIAN_POINT ( 'NONE',  ( -19.80535357387461204, 19.50875577042408793, 0.9260390330000090042 ) ) ;
#16046 = CARTESIAN_POINT ( 'NONE',  ( -8.175142068926048111, -27.46593847456960091, 8.000000000000007105 ) ) ;
#16047 = LINE ( 'NONE', #18711, #30402 ) ;
#16048 = CARTESIAN_POINT ( 'NONE',  ( 25.95386538600433468, 9.395593539459452970, -0.6999999999999784173 ) ) ;
#16049 = B_SPLINE_CURVE_WITH_KNOTS ( 'NONE', 1,
 ( #6545, #30780 ),
 .UNSPECIFIED., .F., .F.,
 ( 2, 2 ),
 ( -0.7031504239110000221, -5.523706192445132501E-08 ),
 .UNSPECIFIED. ) ;
#16050 = DIRECTION ( 'NONE',  ( 0.000000000000000000, 0.000000000000000000, 1.000000000000000000 ) ) ;
#16051 = CARTESIAN_POINT ( 'NONE',  ( -8.999999999710000864, 21.35000000040000145, -51.10000000000000142 ) ) ;
#16052 = DIRECTION ( 'NONE',  ( -2.254056676789046554E-12, 0.05233595624287792208, -0.9986295347545773859 ) ) ;
#16053 = ORIENTED_EDGE ( 'NONE', *, *, #7866, .T. ) ;
#16054 = B_SPLINE_CURVE_WITH_KNOTS ( 'NONE', 1,
 ( #17806, #20182 ),
 .UNSPECIFIED., .F., .F.,
 ( 2, 2 ),
 ( -2.556331299420000144E-06, 0.7000000000009999335 ),
 .UNSPECIFIED. ) ;
#16055 = DIRECTION ( 'NONE',  ( -1.000000000000000000, 0.000000000000000000, 0.000000000000000000 ) ) ;
#16056 = CARTESIAN_POINT ( 'NONE',  ( -24.50074272580000212, -13.13701158840000005, 224.3191686030000369 ) ) ;
#16057 = CARTESIAN_POINT ( 'NONE',  ( 1.100000000000000089, -26.77741585740000119, 5.000000000000000000 ) ) ;
#16058 = ORIENTED_EDGE ( 'NONE', *, *, #10913, .T. ) ;
#16059 = CARTESIAN_POINT ( 'NONE',  ( 2.295476649252899293, -3.592865671589305698, -43.56966640442499994 ) ) ;
#16060 = ORIENTED_EDGE ( 'NONE', *, *, #9895, .F. ) ;
#16061 = VERTEX_POINT ( 'NONE', #14268 ) ;
#16062 = AXIS2_PLACEMENT_3D ( 'NONE', #15992, #21034, #6699 ) ;
#16063 = PRESENTATION_STYLE_ASSIGNMENT (( #4263 ) ) ;
#16064 = AXIS2_PLACEMENT_3D ( 'NONE', #27098, #17939, #5996 ) ;
#16065 = EDGE_LOOP ( 'NONE', ( #9161, #28521, #28205, #20890 ) ) ;
#16066 = CARTESIAN_POINT ( 'NONE',  ( 25.45460661299999927, 14.13620899630000061, 229.0000000000000000 ) ) ;
#16067 = ORIENTED_EDGE ( 'NONE', *, *, #17683, .T. ) ;
#16068 = CARTESIAN_POINT ( 'NONE',  ( -24.19505510210000310, -13.69211658319999891, 226.0798679069999935 ) ) ;
#16069 = SURFACE_SIDE_STYLE ('',( #6465 ) ) ;
#16070 = FACE_OUTER_BOUND ( 'NONE', #751, .T. ) ;
#16071 = CARTESIAN_POINT ( 'NONE',  ( 17.93011078765611543, -8.208160914697428368, 0.000000000000000000 ) ) ;
#16072 = DIRECTION ( 'NONE',  ( 0.3633921898465276024, -0.9316362575375355393, 0.000000000000000000 ) ) ;
#16073 = CARTESIAN_POINT ( 'NONE',  ( -2.073454313851445630, -3.930924299778634889, -38.89973510836055937 ) ) ;
#16074 = CARTESIAN_POINT ( 'NONE',  ( -7.999999999671841167, -13.47848852103334671, -35.10240435524886493 ) ) ;
#16075 = ORIENTED_EDGE ( 'NONE', *, *, #24613, .F. ) ;
#16076 = CARTESIAN_POINT ( 'NONE',  ( -2.624260084387257219, -3.463915187244964056, -3.728945369300004753 ) ) ;
#16077 = CARTESIAN_POINT ( 'NONE',  ( -4.555585884337687297, -4.059738318096004939, -24.24101932449999808 ) ) ;
#16078 = CARTESIAN_POINT ( 'NONE',  ( -2.639254916689323327, -27.37824394259287430, 210.0000000000000284 ) ) ;
#16079 = EDGE_CURVE ( 'NONE', #19872, #18447, #28550, .T. ) ;
#16080 = CARTESIAN_POINT ( 'NONE',  ( -2.900191202563959791, -2.037985736696075634, -90.52455892065360388 ) ) ;
#16081 = CARTESIAN_POINT ( 'NONE',  ( -1.014482461697403970, 3.499829073224391074, 227.7293001947028586 ) ) ;
#16082 = CARTESIAN_POINT ( 'NONE',  ( -11.69999999989999928, -24.11120071630000083, -1.399999999999998579 ) ) ;
#16083 = CARTESIAN_POINT ( 'NONE',  ( 9.000000000029999114, 20.99999999999999645, -45.10000000000000142 ) ) ;
#16084 = CARTESIAN_POINT ( 'NONE',  ( -17.59696597919420213, 10.20816091468181774, 0.000000000000000000 ) ) ;
#16085 = CARTESIAN_POINT ( 'NONE',  ( 1.592882851206511186, -27.75460863273100998, 5.208113774000016960 ) ) ;
#16086 = DIRECTION ( 'NONE',  ( -1.000000000000000000, 5.665498452320000818E-16, 0.000000000000000000 ) ) ;
#16087 = ORIENTED_EDGE ( 'NONE', *, *, #11751, .F. ) ;
#16088 = CARTESIAN_POINT ( 'NONE',  ( -4.050122923326521018, -2.059172231882739457, -61.96424626872499175 ) ) ;
#16089 = DIRECTION ( 'NONE',  ( -1.000000000000000000, 0.000000000000000000, 0.000000000000000000 ) ) ;
#16090 = EDGE_LOOP ( 'NONE', ( #25909, #14532, #29037, #24726 ) ) ;
#16091 = EDGE_LOOP ( 'NONE', ( #11593, #23123, #8035, #11087 ) ) ;
#16092 = CARTESIAN_POINT ( 'NONE',  ( -24.76521256262105553, -10.24325429074770533, 93.21714158839978381 ) ) ;
#16093 = CARTESIAN_POINT ( 'NONE',  ( 0.8594151385421661127, 6.036396974313712249, -29.00600711719999936 ) ) ;
#16094 = VERTEX_POINT ( 'NONE', #4826 ) ;
#16095 = CARTESIAN_POINT ( 'NONE',  ( -24.68204616399999907, -14.25020164319999871, 226.1000014189999945 ) ) ;
#16096 = CARTESIAN_POINT ( 'NONE',  ( -8.699999999707589637, -24.26136093481122558, -29.62468611113576955 ) ) ;
#16097 = ORIENTED_EDGE ( 'NONE', *, *, #11697, .T. ) ;
#16098 = ADVANCED_FACE ( 'NONE', ( #7177 ), #9541, .T. ) ;
#16099 = ORIENTED_EDGE ( 'NONE', *, *, #27103, .F. ) ;
#16100 = VERTEX_POINT ( 'NONE', #14113 ) ;
#16101 = CARTESIAN_POINT ( 'NONE',  ( 3.472061923294214036, -0.4504971222157764243, -91.21022378307108625 ) ) ;
#16102 = ORIENTED_EDGE ( 'NONE', *, *, #29602, .T. ) ;
#16103 = CARTESIAN_POINT ( 'NONE',  ( -9.999999999949999108, -30.49286765380000119, -21.04171673159999756 ) ) ;
#16104 = TOROIDAL_SURFACE ( 'NONE', #8044, 18.16530045470000232, 1.000000000000000000 ) ;
#16105 = CARTESIAN_POINT ( 'NONE',  ( 28.49528339128749366, 0.5184828350247753237, 8.000000000000007105 ) ) ;
#16106 = CARTESIAN_POINT ( 'NONE',  ( 4.962532606730165163, 2.397722036441031435, -66.05315453652499968 ) ) ;
#16107 = ADVANCED_FACE ( 'NONE', ( #19293 ), #9880, .F. ) ;
#16108 = CARTESIAN_POINT ( 'NONE',  ( 5.096711188909999635, -30.05771175659999983, 229.9751249150000092 ) ) ;
#16109 = CARTESIAN_POINT ( 'NONE',  ( -22.62479587716020291, 18.00962536120669810, 1.000000000000000888 ) ) ;
#16110 = CARTESIAN_POINT ( 'NONE',  ( -22.22795129429999861, -18.08627278310000008, 222.0000000000000000 ) ) ;
#16111 = CARTESIAN_POINT ( 'NONE',  ( 4.969670261926683708, -1.740894218915336911, -35.69999999999999574 ) ) ;
#16112 = ORIENTED_EDGE ( 'NONE', *, *, #14060, .T. ) ;
#16113 = CARTESIAN_POINT ( 'NONE',  ( -19.47854282320343700, 20.00003316006251097, -0.2808666865635076060 ) ) ;
#16114 = CARTESIAN_POINT ( 'NONE',  ( -3.222838750790782303, 3.984490938364168233, -12.66602819870000296 ) ) ;
#16115 = DIRECTION ( 'NONE',  ( 0.0001253086065159677936, 1.534587838753951648E-20, -0.9999999921488764709 ) ) ;
#16116 = B_SPLINE_CURVE_WITH_KNOTS ( 'NONE', 5,
 ( #9428, #30996, #28475, #2212, #28633, #11799, #16206, #11493, #6916, #25971, #6765, #4719 ),
 .UNSPECIFIED., .F., .F.,
 ( 6, 3, 3, 6 ),
 ( 0.000000000000000000, 1.357884647199999906, 2.715789078020000247, 3.784579751639999934 ),
 .UNSPECIFIED. ) ;
#16117 = CARTESIAN_POINT ( 'NONE',  ( -27.03594125075309762, -0.4919295335571652328, -0.6999999999999784173 ) ) ;
#16118 = ORIENTED_EDGE ( 'NONE', *, *, #28773, .F. ) ;
#16119 = CARTESIAN_POINT ( 'NONE',  ( 25.11738521000000190, -13.46751580659999981, 224.3193205009999929 ) ) ;
#16120 = CARTESIAN_POINT ( 'NONE',  ( -10.69999999999999929, -128.3726541643999894, -35.73121451845000252 ) ) ;
#16121 = CARTESIAN_POINT ( 'NONE',  ( 10.99999999979999998, 20.99999999990000887, -70.09999999999999432 ) ) ;
#16122 = CARTESIAN_POINT ( 'NONE',  ( 9.739400760072928875, -25.71769950840797847, 25.91465618243121938 ) ) ;
#16123 = CARTESIAN_POINT ( 'NONE',  ( -23.53263993762945461, -14.22965940626688131, 4.040453395607338294 ) ) ;
#16124 = CARTESIAN_POINT ( 'NONE',  ( 0.8648632234848976363, -6.342619565911398638, -49.76468436622499780 ) ) ;
#16125 = CARTESIAN_POINT ( 'NONE',  ( 9.999999999959999997, -24.87868334570000073, -26.27868334529999927 ) ) ;
#16126 = FACE_OUTER_BOUND ( 'NONE', #4989, .T. ) ;
#16127 = ORIENTED_EDGE ( 'NONE', *, *, #4472, .T. ) ;
#16128 = ADVANCED_FACE ( 'NONE', ( #30947 ), #4971, .T. ) ;
#16129 = CARTESIAN_POINT ( 'NONE',  ( -8.699999999988495603, -117.2796036019060466, 12.53378552382356403 ) ) ;
#16130 = CARTESIAN_POINT ( 'NONE',  ( 2.876789788197821718, -3.528003781030157437, -68.10000000002500542 ) ) ;
#16131 = CARTESIAN_POINT ( 'NONE',  ( -0.4822370987978389367, -3.496762477110187284, -0.6999999999999784173 ) ) ;
#16132 = CARTESIAN_POINT ( 'NONE',  ( -4.111734365088209664, -0.1631247855115738887, -44.10000000002499121 ) ) ;
#16133 = FILL_AREA_STYLE_COLOUR ( '', #27362 ) ;
#16134 = ORIENTED_EDGE ( 'NONE', *, *, #20770, .F. ) ;
#16135 = CARTESIAN_POINT ( 'NONE',  ( -10.52451944200266354, 6.422810504745973148, 232.6627637660202481 ) ) ;
#16136 = CARTESIAN_POINT ( 'NONE',  ( 5.807653394784360934, -2.603268055249425394, -67.27841551502500295 ) ) ;
#16137 = ORIENTED_EDGE ( 'NONE', *, *, #886, .T. ) ;
#16138 = EDGE_CURVE ( 'NONE', #20193, #23914, #18976, .T. ) ;
#16139 = DIRECTION ( 'NONE',  ( -0.9880370573969196046, 0.1542166437529879364, 0.000000000000000000 ) ) ;
#16140 = CARTESIAN_POINT ( 'NONE',  ( -2.091444806098883280, -2.888061030879386593, -88.52261276293990022 ) ) ;
#16141 = VERTEX_POINT ( 'NONE', #4660 ) ;
#16142 = CARTESIAN_POINT ( 'NONE',  ( -4.874695217770000255, 3.326860129169999958, 226.6412452697800006 ) ) ;
#16143 = DIRECTION ( 'NONE',  ( 0.000000000000000000, 1.000000000000000000, 0.000000000000000000 ) ) ;
#16144 = DIRECTION ( 'NONE',  ( 0.000000000000000000, 0.000000000000000000, 1.000000000000000000 ) ) ;
#16145 = CARTESIAN_POINT ( 'NONE',  ( -2.347741120694188055, 2.634769306325225102, 0.000000000000000000 ) ) ;
#16146 = B_SPLINE_CURVE_WITH_KNOTS ( 'NONE', 3,
 ( #2517, #2665, #24223, #9905, #17556, #15201 ),
 .UNSPECIFIED., .F., .F.,
 ( 4, 2, 4 ),
 ( 0.000000000000000000, 0.5000000000000000000, 1.000000000000000000 ),
 .UNSPECIFIED. ) ;
#16147 = CARTESIAN_POINT ( 'NONE',  ( 0.03635086285233400660, -28.50041301604787947, 3.997479608999987555 ) ) ;
#16148 = DIRECTION ( 'NONE',  ( 0.000000000000000000, -1.000000000000000000, 0.000000000000000000 ) ) ;
#16149 = CARTESIAN_POINT ( 'NONE',  ( -26.80000000069999899, 3.281945028329999726E-15, 230.0000000000000000 ) ) ;
#16150 = ORIENTED_EDGE ( 'NONE', *, *, #8448, .F. ) ;
#16151 = FACE_BOUND ( 'NONE', #967, .T. ) ;
#16152 = ADVANCED_FACE ( 'NONE', ( #23874 ), #23042, .T. ) ;
#16153 = CARTESIAN_POINT ( 'NONE',  ( 3.760007715734311251, -19.71206033683614578, -27.86495495662581945 ) ) ;
#16154 = LINE ( 'NONE', #25616, #24841 ) ;
#16155 = EDGE_CURVE ( 'NONE', #4760, #17409, #8452, .T. ) ;
#16156 = DIRECTION ( 'NONE',  ( 1.000000000000000000, 0.000000000000000000, 0.000000000000000000 ) ) ;
#16157 = MECHANICAL_DESIGN_GEOMETRIC_PRESENTATION_REPRESENTATION (  '', ( #25184 ), #27689 ) ;
#16158 = DIRECTION ( 'NONE',  ( 0.000000000000000000, 0.000000000000000000, 1.000000000000000000 ) ) ;
#16159 = CARTESIAN_POINT ( 'NONE',  ( 9.051856682629999540, 7.975114694340000199, 230.6412452697800006 ) ) ;
#16160 = CARTESIAN_POINT ( 'NONE',  ( -8.903108651239966420, -22.82508830966961000, 90.00000000000000000 ) ) ;
#16161 = DIRECTION ( 'NONE',  ( 1.000000000000000000, -1.843431230206220100E-12, 2.650498504954374861E-12 ) ) ;
#16162 = CARTESIAN_POINT ( 'NONE',  ( -4.064488300603595228, -4.392874523441014034, -50.19612412472499585 ) ) ;
#16163 = EDGE_CURVE ( 'NONE', #28640, #12600, #15778, .T. ) ;
#16164 = CARTESIAN_POINT ( 'NONE',  ( 0.000000000000000000, 20.99999999999999645, -44.10000000017154065 ) ) ;
#16165 = CARTESIAN_POINT ( 'NONE',  ( 24.36724931188768650, 13.38201648792073684, 4.999998581000003384 ) ) ;
#16166 = DIRECTION ( 'NONE',  ( 0.000000000000000000, 0.000000000000000000, -1.000000000000000000 ) ) ;
#16167 = DIRECTION ( 'NONE',  ( 0.000000000000000000, 0.000000000000000000, -1.000000000000000000 ) ) ;
#16168 = ORIENTED_EDGE ( 'NONE', *, *, #14195, .T. ) ;
#16169 = B_SPLINE_CURVE_WITH_KNOTS ( 'NONE', 5,
 ( #10445, #8213, #556, #20039, #29637, #10596 ),
 .UNSPECIFIED., .F., .F.,
 ( 6, 6 ),
 ( -17.34990440099999987, 0.000000000000000000 ),
 .UNSPECIFIED. ) ;
#16170 = CARTESIAN_POINT ( 'NONE',  ( 4.618385388201741826, 1.362661324479865099, -36.46909726779999517 ) ) ;
#16171 = EDGE_CURVE ( 'NONE', #9577, #12816, #14888, .T. ) ;
#16172 = ORIENTED_EDGE ( 'NONE', *, *, #6842, .F. ) ;
#16173 = CARTESIAN_POINT ( 'NONE',  ( -0.9891938378274514054, -4.753657830815118501, -53.32706695232499783 ) ) ;
#16174 = VERTEX_POINT ( 'NONE', #29038 ) ;
#16175 = SHAPE_DEFINITION_REPRESENTATION ( #15589, #20820 ) ;
#16176 = VECTOR ( 'NONE', #15565, 1000.000000000000000 ) ;
#16177 = ORIENTED_EDGE ( 'NONE', *, *, #18821, .T. ) ;
#16178 = CARTESIAN_POINT ( 'NONE',  ( -10.69999999999999929, -27.00000000000000000, -28.40000000000000213 ) ) ;
#16179 = PRODUCT ( 'MAS-156', 'MAS-156', '', ( #12809 ) ) ;
#16180 = ORIENTED_EDGE ( 'NONE', *, *, #12699, .T. ) ;
#16181 = CARTESIAN_POINT ( 'NONE',  ( 14.77468706462270376, -30.48866542731327911, -24.64097061684832468 ) ) ;
#16182 = EDGE_CURVE ( 'NONE', #10856, #21922, #6650, .T. ) ;
#16183 = CARTESIAN_POINT ( 'NONE',  ( 5.925670221678688065, -8.802561022165985349, -36.52367911919805721 ) ) ;
#16184 = CARTESIAN_POINT ( 'NONE',  ( 9.431516900800000658E-09, 2.029448609160000227E-09, 230.0000000000000000 ) ) ;
#16185 = CARTESIAN_POINT ( 'NONE',  ( 8.000000000468180161, -13.43844522892069371, -35.09918421751434892 ) ) ;
#16186 = CARTESIAN_POINT ( 'NONE',  ( -6.982632971260602339, 5.672256964628558329, -40.24571374304650107 ) ) ;
#16187 = CARTESIAN_POINT ( 'NONE',  ( 5.523879335194060936, -0.1907134851046367874, -1.685409721200002764 ) ) ;
#16188 = CARTESIAN_POINT ( 'NONE',  ( -26.80000000000000071, -9.846360514330001479, 230.6999999999999886 ) ) ;
#16189 = ORIENTED_EDGE ( 'NONE', *, *, #10606, .F. ) ;
#16190 = DIRECTION ( 'NONE',  ( 0.000000000000000000, 0.000000000000000000, -1.000000000000000000 ) ) ;
#16191 = CARTESIAN_POINT ( 'NONE',  ( -5.990533020055879732, -1.129328118392731950, -16.09949426530000238 ) ) ;
#16192 = CARTESIAN_POINT ( 'NONE',  ( 5.318140750231298064, 1.569125161471404573, -34.53159726779999517 ) ) ;
#16193 = ADVANCED_FACE ( 'NONE', ( #24480 ), #26246, .T. ) ;
#16194 = VECTOR ( 'NONE', #17538, 999.9999999999998863 ) ;
#16195 = CARTESIAN_POINT ( 'NONE',  ( 24.29903249413439781, 13.50560429725452849, 4.442423594862364489 ) ) ;
#16196 = CARTESIAN_POINT ( 'NONE',  ( 1.115119965759999943, -28.47834310740000063, 224.7918990269999995 ) ) ;
#16197 = CARTESIAN_POINT ( 'NONE',  ( 27.84775205013805888, -6.760390605069130032, 8.000000000000007105 ) ) ;
#16198 = CARTESIAN_POINT ( 'NONE',  ( -15.49562240950000103, -7.676231176589999983, 225.0000000000000000 ) ) ;
#16199 = B_SPLINE_SURFACE_WITH_KNOTS ( 'NONE', 5, 1, ( 
 ( #7551, #17141 ),
 ( #4572, #23782 ),
 ( #2223, #7090 ),
 ( #16678, #4733 ),
 ( #14342, #23941 ),
 ( #2378, #11964 ),
 ( #22, #18354 ),
 ( #2986, #7846 ),
 ( #17451, #15991 ),
 ( #27056, #10961 ),
 ( #12576, #22340 ),
 ( #8001, #11118 ),
 ( #25446, #27786 ),
 ( #6235, #5493 ),
 ( #10229, #15842 ) ),
 .UNSPECIFIED., .F., .F., .F.,
 ( 6, 3, 3, 3, 6 ),
 ( 2, 2 ),
 ( 0.000000000000000000, 0.5238999883160000426, 1.047799976630000129, 1.571699964950000084, 1.746333294390000068 ),
 ( -0.7000000000009999335, 2.555882182119999914E-06 ),
 .UNSPECIFIED. ) ;
#16200 = CARTESIAN_POINT ( 'NONE',  ( 0.000000000000000000, 0.000000000000000000, 230.6412452697800006 ) ) ;
#16201 = CARTESIAN_POINT ( 'NONE',  ( -23.68823177905599309, -12.53428999867805160, 4.513393846701676537 ) ) ;
#16202 = DIRECTION ( 'NONE',  ( 0.000000000000000000, 0.000000000000000000, -1.000000000000000000 ) ) ;
#16203 = CARTESIAN_POINT ( 'NONE',  ( 20.30396079652883756, 20.00000000004620304, 1.000000000000000888 ) ) ;
#16204 = VERTEX_POINT ( 'NONE', #12510 ) ;
#16205 = B_SPLINE_CURVE_WITH_KNOTS ( 'NONE', 3,
 ( #22659, #25332, #27222, #29583, #1102, #29427, #3147, #17762, #27379, #15263, #5665, #12905 ),
 .UNSPECIFIED., .F., .F.,
 ( 4, 2, 2, 2, 2, 4 ),
 ( 0.000000000000000000, 0.2499999999999890643, 0.4999999999999781286, 0.6249999999999726885, 0.7499999999999671374, 1.000000000000000000 ),
 .UNSPECIFIED. ) ;
#16206 = CARTESIAN_POINT ( 'NONE',  ( -10.63581336909999919, 19.99999999999999645, -1.053405123100002783 ) ) ;
#16207 = LINE ( 'NONE', #25822, #15243 ) ;
#16208 = EDGE_CURVE ( 'NONE', #15627, #2709, #20628, .T. ) ;
#16209 = AXIS2_PLACEMENT_3D ( 'NONE', #8261, #30303, #3869 ) ;
#16210 = CARTESIAN_POINT ( 'NONE',  ( 0.09454741856676797396, -5.198049559341232140, -0.7000607835638984477 ) ) ;
#16211 = VERTEX_POINT ( 'NONE', #578 ) ;
#16212 = VERTEX_POINT ( 'NONE', #19759 ) ;
#16213 = ORIENTED_EDGE ( 'NONE', *, *, #4381, .T. ) ;
#16214 = EDGE_CURVE ( 'NONE', #1526, #19354, #2629, .T. ) ;
#16215 =( LENGTH_UNIT ( ) NAMED_UNIT ( * ) SI_UNIT ( .MILLI., .METRE. ) );
#16216 = ORIENTED_EDGE ( 'NONE', *, *, #11149, .F. ) ;
#16217 = DIRECTION ( 'NONE',  ( 1.000000000000000000, 0.000000000000000000, 0.000000000000000000 ) ) ;
#16218 = ORIENTED_EDGE ( 'NONE', *, *, #26802, .F. ) ;
#16219 = AXIS2_PLACEMENT_3D ( 'NONE', #18441, #13091, #29933 ) ;
#16220 = CARTESIAN_POINT ( 'NONE',  ( -25.27354923189999880, 12.75979636610000156, 229.0000000000000000 ) ) ;
#16221 = DIRECTION ( 'NONE',  ( 0.3090169943750400994, -0.9510565162951234441, 0.000000000000000000 ) ) ;
#16222 = CARTESIAN_POINT ( 'NONE',  ( 3.650208047081187512, 0.9579503420338048025, -35.69999999999999574 ) ) ;
#16223 = CARTESIAN_POINT ( 'NONE',  ( -6.505665861548826534, 6.032487712052573059, -40.42141001841366688 ) ) ;
#16224 = CARTESIAN_POINT ( 'NONE',  ( 12.69530690868993617, -23.62822639411161418, -1.399999999999998801 ) ) ;
#16225 = CARTESIAN_POINT ( 'NONE',  ( -8.699999999648399651, -15.36399602968765521, -37.98537634616555181 ) ) ;
#16226 = CARTESIAN_POINT ( 'NONE',  ( -18.62349881349999947, 19.80369232029999793, 229.9327143820000003 ) ) ;
#16227 = VERTEX_POINT ( 'NONE', #24322 ) ;
#16228 = CARTESIAN_POINT ( 'NONE',  ( -1.295942751353782674, 4.166547562507306957, -5.274955258300003891 ) ) ;
#16229 = CARTESIAN_POINT ( 'NONE',  ( -3.253989917302557267, -2.899813084402114161, -24.34101932450000305 ) ) ;
#16230 = FACE_OUTER_BOUND ( 'NONE', #15391, .T. ) ;
#16231 = CARTESIAN_POINT ( 'NONE',  ( -17.83931601680000156, 20.00000000000000000, 230.7000111870000012 ) ) ;
#16232 = CARTESIAN_POINT ( 'NONE',  ( 1.645798001274432654, 3.499999999995804689, 227.8506595042291565 ) ) ;
#16233 = CARTESIAN_POINT ( 'NONE',  ( -25.46368746807222649, 12.80129684246671751, 5.147587686977050048 ) ) ;
#16234 = CARTESIAN_POINT ( 'NONE',  ( -2.020725942159999899, -3.500000000000000000, 229.2412452703699728 ) ) ;
#16235 = CARTESIAN_POINT ( 'NONE',  ( 27.09307779339999911, 1.384329942100000039E-12, 229.9751247039999953 ) ) ;
#16236 = CARTESIAN_POINT ( 'NONE',  ( 1.605176535610508326, -27.75389821387976852, 4.999998581000003384 ) ) ;
#16237 = CARTESIAN_POINT ( 'NONE',  ( 0.000000000000000000, 0.000000000000000000, 140.0000000000000000 ) ) ;
#16238 = ORIENTED_EDGE ( 'NONE', *, *, #21056, .T. ) ;
#16239 = CARTESIAN_POINT ( 'NONE',  ( 2.637655088286928962, -3.673227524439524050, -61.52197827312500067 ) ) ;
#16240 = CONICAL_SURFACE ( 'NONE', #2192, 0.9999999999991036059, 0.7853981633970000820 ) ;
#16241 = CARTESIAN_POINT ( 'NONE',  ( -1.386473475049334159, -1.583312407435810254, 226.6412452697799722 ) ) ;
#16242 = ORIENTED_EDGE ( 'NONE', *, *, #20758, .F. ) ;
#16243 = LINE ( 'NONE', #18606, #7737 ) ;
#16244 = CARTESIAN_POINT ( 'NONE',  ( -3.231711866632715147, -5.662799918003592836, -30.67642233980000199 ) ) ;
#16245 = EDGE_LOOP ( 'NONE', ( #22826, #14938, #9004, #3585 ) ) ;
#16246 = CARTESIAN_POINT ( 'NONE',  ( 18.95046173579999760, -18.95046173579999760, 136.7828584120000244 ) ) ;
#16247 = FACE_OUTER_BOUND ( 'NONE', #1088, .T. ) ;
#16248 = VERTEX_POINT ( 'NONE', #2769 ) ;
#16249 = ORIENTED_EDGE ( 'NONE', *, *, #26237, .T. ) ;
#16250 = ORIENTED_EDGE ( 'NONE', *, *, #12590, .T. ) ;
#16251 = FILL_AREA_STYLE_COLOUR ( '', #11803 ) ;
#16252 = ORIENTED_EDGE ( 'NONE', *, *, #28848, .T. ) ;
#16253 = DIRECTION ( 'NONE',  ( -1.000000000000000000, 5.665498452320000818E-16, 0.000000000000000000 ) ) ;
#16254 = EDGE_CURVE ( 'NONE', #31001, #27054, #7851, .T. ) ;
#16255 = CARTESIAN_POINT ( 'NONE',  ( -8.699999999628206027, -18.27232546675181268, -40.96725586010739306 ) ) ;
#16256 = CARTESIAN_POINT ( 'NONE',  ( -5.007939960741254026, -2.959237434304809788, -67.52382590962501752 ) ) ;
#16257 = AXIS2_PLACEMENT_3D ( 'NONE', #9114, #13689, #16050 ) ;
#16258 = CARTESIAN_POINT ( 'NONE',  ( 12.80098767942999771, -32.00000000000000000, -31.28675134584999640 ) ) ;
#16259 = VECTOR ( 'NONE', #8855, 1000.000000000000000 ) ;
#16260 = DIRECTION ( 'NONE',  ( -1.000000000000000000, 5.687697913155423197E-16, -6.771501495041734442E-12 ) ) ;
#16261 = CARTESIAN_POINT ( 'NONE',  ( -23.69219497580000322, -16.12132049240000242, 222.0000000000000000 ) ) ;
#16262 = CARTESIAN_POINT ( 'NONE',  ( -23.65805500392816896, -12.59178324492199508, 5.597929191016143946 ) ) ;
#16263 = ORIENTED_EDGE ( 'NONE', *, *, #14582, .F. ) ;
#16264 = CARTESIAN_POINT ( 'NONE',  ( -19.89484633387414902, 20.00030665124463169, 0.04277443887995936722 ) ) ;
#16265 = CARTESIAN_POINT ( 'NONE',  ( 3.665953941183818010, 4.858601989977915814, -14.22796858840000311 ) ) ;
#16266 = B_SPLINE_CURVE_WITH_KNOTS ( 'NONE', 3,
 ( #21670, #12065, #19304, #16776 ),
 .UNSPECIFIED., .F., .F.,
 ( 4, 4 ),
 ( 0.000000000000000000, 1.000000000000000000 ),
 .UNSPECIFIED. ) ;
#16267 = CARTESIAN_POINT ( 'NONE',  ( 20.19452343149548668, -17.70639519314953958, 0.000000000000000000 ) ) ;
#16268 = CARTESIAN_POINT ( 'NONE',  ( -28.45300238704230367, -0.5177135156027794505, 0.5017677510000262409 ) ) ;
#16269 = ORIENTED_EDGE ( 'NONE', *, *, #17127, .F. ) ;
#16270 = CARTESIAN_POINT ( 'NONE',  ( 16.06675444873834380, 10.97998838177521286, -0.6999999999999784173 ) ) ;
#16271 = CARTESIAN_POINT ( 'NONE',  ( -11.49999999969999998, -27.00000000000000000, -28.40000000000541647 ) ) ;
#16272 = CARTESIAN_POINT ( 'NONE',  ( 28.49999999979999998, -7.466149220249999274, 222.0000000000000000 ) ) ;
#16273 = CARTESIAN_POINT ( 'NONE',  ( 4.696583076644019528, -27.09716880376584314, 20.40570884047772893 ) ) ;
#16274 = CARTESIAN_POINT ( 'NONE',  ( 23.06380069550898781, -13.64989377374051216, 3.928509483758267251 ) ) ;
#16275 = LINE ( 'NONE', #4798, #18205 ) ;
#16276 = LINE ( 'NONE', #1976, #27800 ) ;
#16277 = DIRECTION ( 'NONE',  ( 0.000000000000000000, 0.000000000000000000, -1.000000000000000000 ) ) ;
#16278 = CIRCLE ( 'NONE', #1209, 3.999999999669999973 ) ;
#16279 = ORIENTED_EDGE ( 'NONE', *, *, #6748, .F. ) ;
#16280 = CARTESIAN_POINT ( 'NONE',  ( -9.999999999969999109, -29.12127062080000073, -30.52127062269999769 ) ) ;
#16281 = CARTESIAN_POINT ( 'NONE',  ( 16.06675444876397307, -9.020011618195203695, -0.6999999999999784173 ) ) ;
#16282 = VECTOR ( 'NONE', #6, 1000.000000000000000 ) ;
#16284 = EDGE_CURVE ( 'NONE', #29399, #9436, #20688, .T. ) ;
#16283 = VECTOR ( 'NONE', #9230, 1000.000000000000000 ) ;
#16285 = AXIS2_PLACEMENT_3D ( 'NONE', #1969, #16581, #9034 ) ;
#16286 = AXIS2_PLACEMENT_3D ( 'NONE', #3435, #6109, #15248 ) ;
#16287 = CARTESIAN_POINT ( 'NONE',  ( 2.536848156347102368, -3.492023641679737000, -68.10000000002503384 ) ) ;
#16288 = FACE_OUTER_BOUND ( 'NONE', #4450, .T. ) ;
#16289 = CARTESIAN_POINT ( 'NONE',  ( -4.140705449094239654, 0.009913425260839086456, -44.10000000002497700 ) ) ;
#16290 = ORIENTED_EDGE ( 'NONE', *, *, #16783, .F. ) ;
#16291 = CARTESIAN_POINT ( 'NONE',  ( -10.69999999930000101, -29.12132034360000077, -30.52132034359999935 ) ) ;
#16292 =( GEOMETRIC_REPRESENTATION_CONTEXT ( 3 ) GLOBAL_UNCERTAINTY_ASSIGNED_CONTEXT ( ( #14724 ) ) GLOBAL_UNIT_ASSIGNED_CONTEXT ( ( #13777, #9832, #12346 ) ) REPRESENTATION_CONTEXT ( 'NONE', 'WORKASPACE' ) );
#16293 = CARTESIAN_POINT ( 'NONE',  ( 5.352151167818264277, -2.399090168609281370, -68.07841551502500010 ) ) ;
#16294 = ORIENTED_EDGE ( 'NONE', *, *, #12709, .T. ) ;
#16295 = FACE_OUTER_BOUND ( 'NONE', #24121, .T. ) ;
#16296 = CARTESIAN_POINT ( 'NONE',  ( -3.542914729026271914, -0.003443490030646811917, -88.52261276311425320 ) ) ;
#16297 = ORIENTED_EDGE ( 'NONE', *, *, #22578, .T. ) ;
#16299 = DIRECTION ( 'NONE',  ( -0.6986477033484088661, 0.1090476345698817712, -0.7071067811870476172 ) ) ;
#16298 = VECTOR ( 'NONE', #21706, 1000.000000000000000 ) ;
#16300 = AXIS2_PLACEMENT_3D ( 'NONE', #4803, #24000, #21785 ) ;
#16301 = AXIS2_PLACEMENT_3D ( 'NONE', #30261, #18292, #30889 ) ;
#16302 = CARTESIAN_POINT ( 'NONE',  ( 27.76135144259999876, -3.399672736709999763E-15, 42.33858589270000294 ) ) ;
#16303 = LINE ( 'NONE', #9809, #18994 ) ;
#16304 = UNCERTAINTY_MEASURE_WITH_UNIT (LENGTH_MEASURE( 1.000000000000000082E-05 ), #1680, 'distance_accuracy_value', 'NONE');
#16305 = CIRCLE ( 'NONE', #22843, 27.50000000000000000 ) ;
#16306 = DIRECTION ( 'NONE',  ( 1.595945597898660305E-12, -0.7071067811865475727, 0.7071067811865475727 ) ) ;
#16307 = CARTESIAN_POINT ( 'NONE',  ( -16.19903397984253957, -9.902734965364627939, 0.000000000000000000 ) ) ;
#16308 = DIRECTION ( 'NONE',  ( -1.000000000000000000, 5.665498452320000818E-16, 0.000000000000000000 ) ) ;
#16309 = EDGE_LOOP ( 'NONE', ( #23302, #29861, #16134, #7161 ) ) ;
#16310 = DIRECTION ( 'NONE',  ( 0.000000000000000000, 0.000000000000000000, -1.000000000000000000 ) ) ;
#16311 = FACE_OUTER_BOUND ( 'NONE', #15943, .T. ) ;
#16312 = CARTESIAN_POINT ( 'NONE',  ( 18.80688676539999804, 20.00000167889999858, 230.5857114979999949 ) ) ;
#16313 = EDGE_CURVE ( 'NONE', #28151, #20047, #19910, .T. ) ;
#16314 = CARTESIAN_POINT ( 'NONE',  ( -15.99701729020289243, -9.715560209340530662, 0.000000000000000000 ) ) ;
#16315 = CARTESIAN_POINT ( 'NONE',  ( 16.89818815097801519, -10.07643063672789019, -0.6999999999999785283 ) ) ;
#16316 = CARTESIAN_POINT ( 'NONE',  ( 8.609713997930001028, 8.450495286409998030, 230.6412452697800006 ) ) ;
#16317 = FACE_OUTER_BOUND ( 'NONE', #20979, .T. ) ;
#16318 = CARTESIAN_POINT ( 'NONE',  ( 13.73773747404255552, -26.37022765825810922, 0.000000000000000000 ) ) ;
#16319 = CARTESIAN_POINT ( 'NONE',  ( 4.390418465362644795, -3.559810858784186127, -55.40923804942499942 ) ) ;
#16320 = CARTESIAN_POINT ( 'NONE',  ( 0.1708583496781539146, 4.358252033550397364, -7.437690181100002462 ) ) ;
#16321 = ADVANCED_FACE ( 'NONE', ( #5886 ), #29964, .F. ) ;
#16322 = CARTESIAN_POINT ( 'NONE',  ( -27.79539923781770128, -0.5057481688779147389, 8.000000000000007105 ) ) ;
#16323 = CARTESIAN_POINT ( 'NONE',  ( -7.358672349382085365, -6.804754899618653319, -34.16026844937522355 ) ) ;
#16324 = CARTESIAN_POINT ( 'NONE',  ( -7.000000000000000000, -15.18061163548115466, -76.53197586718597734 ) ) ;
#16325 = VECTOR ( 'NONE', #17021, 1000.000000000000114 ) ;
#16326 = VECTOR ( 'NONE', #8926, 1000.000000000000000 ) ;
#16327 = CARTESIAN_POINT ( 'NONE',  ( 14.00000000000000000, 21.70000000000000284, -62.80809897700000022 ) ) ;
#16328 = CARTESIAN_POINT ( 'NONE',  ( -23.56565371570000167, -14.74874063799999924, 224.4928788709999878 ) ) ;
#16329 = ORIENTED_EDGE ( 'NONE', *, *, #28483, .T. ) ;
#16330 = ADVANCED_FACE ( 'NONE', ( #28075 ), #27761, .F. ) ;
#16331 = CARTESIAN_POINT ( 'NONE',  ( 2.743362564037614248, -4.941860934411918649, -55.58172062782499268 ) ) ;
#16332 = VERTEX_POINT ( 'NONE', #30127 ) ;
#16333 = ITEM_DEFINED_TRANSFORMATION ( 'NONE', 'NONE', #30929,  #17722 ) ;
#16334 = EDGE_LOOP ( 'NONE', ( #2336, #14634, #1768, #8083 ) ) ;
#16335 = ORIENTED_EDGE ( 'NONE', *, *, #12673, .T. ) ;
#16336 = CIRCLE ( 'NONE', #11801, 3.000000000000001332 ) ;
#16337 = PRESENTATION_LAYER_ASSIGNMENT (  '', '', ( #14357 ) ) ;
#16338 = CYLINDRICAL_SURFACE ( 'NONE', #24331, 2.500000000000000888 ) ;
#16339 = CARTESIAN_POINT ( 'NONE',  ( 0.000000000000000000, 0.000000000000000000, 115.0000000000000000 ) ) ;
#16340 = CARTESIAN_POINT ( 'NONE',  ( 23.73992238019999945, -12.43607998449999918, 5.000000000000000000 ) ) ;
#16341 = DIRECTION ( 'NONE',  ( 1.000000000000000000, 0.000000000000000000, 0.000000000000000000 ) ) ;
#16342 = CARTESIAN_POINT ( 'NONE',  ( -27.66290831536099759, -7.787312998881454895, 1.000000000000000888 ) ) ;
#16343 = DIRECTION ( 'NONE',  ( -0.3090169943750401549, -0.9510565162951233331, 0.000000000000000000 ) ) ;
#16344 = CARTESIAN_POINT ( 'NONE',  ( 4.781918068392163157, 0.6270375808061986467, -4.689479598399999283 ) ) ;
#16345 = CARTESIAN_POINT ( 'NONE',  ( 5.353429552090000598, -31.57167681289999805, 229.4982322489999831 ) ) ;
#16346 = ORIENTED_EDGE ( 'NONE', *, *, #26394, .F. ) ;
#16347 = LINE ( 'NONE', #13678, #18510 ) ;
#16348 = CARTESIAN_POINT ( 'NONE',  ( -5.990533020055879732, -1.129328118392731950, -16.69949426530000025 ) ) ;
#16349 = CARTESIAN_POINT ( 'NONE',  ( 0.1051796283266584475, -6.084780997910130829, -32.81110030499999652 ) ) ;
#16350 = CARTESIAN_POINT ( 'NONE',  ( 24.36724931188768650, 13.38201648792073684, 4.999998581000003384 ) ) ;
#16351 = CARTESIAN_POINT ( 'NONE',  ( -18.31085446006445494, 19.88197403644849004, 0.02160863700001458554 ) ) ;
#16352 = CARTESIAN_POINT ( 'NONE',  ( -7.999999999628064629, -15.40335946066103645, -40.52613281826078406 ) ) ;
#16353 = CARTESIAN_POINT ( 'NONE',  ( -2.020725942109999895, 3.500000000090000007, 227.9588918784999976 ) ) ;
#16354 = ADVANCED_FACE ( 'NONE', ( #8238 ), #14664, .F. ) ;
#16355 = CARTESIAN_POINT ( 'NONE',  ( 27.35479945376005873, 9.902747534594007917, 0.7595836940000044724 ) ) ;
#16356 = PLANE ( 'NONE',  #16257 ) ;
#16357 = CARTESIAN_POINT ( 'NONE',  ( -20.97469196846414974, 18.32172385076221488, 4.666666738000063930 ) ) ;
#16358 = PRODUCT_DEFINITION_FORMATION_WITH_SPECIFIED_SOURCE ( 'ANY', '', #18097, .NOT_KNOWN. ) ;
#16359 = CARTESIAN_POINT ( 'NONE',  ( -12.51132621223302799, 21.69999999994217177, -69.72125039903896493 ) ) ;
#16360 = EDGE_LOOP ( 'NONE', ( #21376, #4017, #11730, #16180 ) ) ;
#16361 = CARTESIAN_POINT ( 'NONE',  ( 6.400666314641494381, -16.58906712865265831, -74.91625619803754432 ) ) ;
#16362 = DIRECTION ( 'NONE',  ( 1.000000000000000000, -1.381176317861079950E-13, 9.436729139529790430E-14 ) ) ;
#16363 = DIRECTION ( 'NONE',  ( -1.000000000000000000, 0.000000000000000000, 0.000000000000000000 ) ) ;
#16364 = ORIENTED_EDGE ( 'NONE', *, *, #30476, .F. ) ;
#16365 = EDGE_CURVE ( 'NONE', #10911, #8911, #11093, .T. ) ;
#16366 = CARTESIAN_POINT ( 'NONE',  ( -4.251810618965843780, 2.500173132353668226, -45.59354844312499466 ) ) ;
#16367 = EDGE_LOOP ( 'NONE', ( #8112, #21173, #25156, #27291 ) ) ;
#16368 = ORIENTED_EDGE ( 'NONE', *, *, #13945, .F. ) ;
#16369 = EDGE_CURVE ( 'NONE', #13888, #29654, #27926, .T. ) ;
#16370 = SURFACE_STYLE_USAGE ( .BOTH. , #23936 ) ;
#16371 = ORIENTED_EDGE ( 'NONE', *, *, #25781, .T. ) ;
#16372 = DIRECTION ( 'NONE',  ( 1.000000000000000000, 0.000000000000000000, 0.000000000000000000 ) ) ;
#16373 = EDGE_CURVE ( 'NONE', #28074, #5070, #26651, .T. ) ;
#16374 = ORIENTED_EDGE ( 'NONE', *, *, #27306, .T. ) ;
#16375 = CARTESIAN_POINT ( 'NONE',  ( 6.258113739069999681, 17.06910001600000015, 230.6999999999999886 ) ) ;
#16376 = CARTESIAN_POINT ( 'NONE',  ( 23.23277125981546476, 15.26692728828886025, 4.999998581000003384 ) ) ;
#16377 = CARTESIAN_POINT ( 'NONE',  ( -24.38199545545641911, -14.75707035126829147, 3.901343066999990228 ) ) ;
#16378 = CARTESIAN_POINT ( 'NONE',  ( -17.49999999969999820, -22.00000000000000000, -25.51324865424999899 ) ) ;
#16379 = ADVANCED_FACE ( 'NONE', ( #16429 ), #23835, .T. ) ;
#16380 = CARTESIAN_POINT ( 'NONE',  ( 18.59033486452720041, 20.00000077194644277, -0.6230606123292589116 ) ) ;
#16381 = DIRECTION ( 'NONE',  ( 0.000000000000000000, 1.000000000000000000, 0.000000000000000000 ) ) ;
#16382 = DIRECTION ( 'NONE',  ( 9.219194983962475343E-13, 0.9128796883888954383, -0.4082287037029530552 ) ) ;
#16383 = CARTESIAN_POINT ( 'NONE',  ( -19.36637386170000141, 20.00000465049999931, 230.3591670750000162 ) ) ;
#16384 = ORIENTED_EDGE ( 'NONE', *, *, #26178, .T. ) ;
#16385 = CARTESIAN_POINT ( 'NONE',  ( 2.246931792404676997, -6.149078805876593279, -6.260585232200001293 ) ) ;
#16386 = CARTESIAN_POINT ( 'NONE',  ( -0.5718866478877175918, 5.491608289559616551, -24.88903409330000116 ) ) ;
#16387 = DIRECTION ( 'NONE',  ( -0.1090476345695678556, -0.6986477033489640887, -0.7071067811865474617 ) ) ;
#16388 = B_SPLINE_CURVE_WITH_KNOTS ( 'NONE', 3,
 ( #12248, #19499, #2966, #24070, #9734, #4869 ),
 .UNSPECIFIED., .F., .F.,
 ( 4, 2, 4 ),
 ( 0.000000000000000000, 0.5000000000000000000, 1.000000000000000000 ),
 .UNSPECIFIED. ) ;
#16389 = EDGE_CURVE ( 'NONE', #15903, #25954, #24733, .T. ) ;
#16390 = PLANE ( 'NONE',  #22732 ) ;
#16391 = CARTESIAN_POINT ( 'NONE',  ( -0.6197578588520477050, 3.499936541727148409, 227.6700366507586466 ) ) ;
#16392 = DIRECTION ( 'NONE',  ( 1.000000000000000000, -9.219999999999999084E-13, 4.710999999999999616E-12 ) ) ;
#16393 = DIRECTION ( 'NONE',  ( 0.000000000000000000, 0.000000000000000000, -1.000000000000000000 ) ) ;
#16394 = ADVANCED_FACE ( 'NONE', ( #18783 ), #28393, .F. ) ;
#16395 = DIRECTION ( 'NONE',  ( 1.000000000000000000, 0.000000000000000000, 0.000000000000000000 ) ) ;
#16396 = FACE_OUTER_BOUND ( 'NONE', #18209, .T. ) ;
#16397 = CARTESIAN_POINT ( 'NONE',  ( -12.69498943403903546, -23.62838044921069169, -1.399999999999998579 ) ) ;
#16398 = ORIENTED_EDGE ( 'NONE', *, *, #20888, .T. ) ;
#16399 = CARTESIAN_POINT ( 'NONE',  ( -5.182433330280534989, 2.850054831770709285, -59.01908057272500230 ) ) ;
#16400 = CARTESIAN_POINT ( 'NONE',  ( -24.70074544867652122, 14.21822122508601716, 6.002806299999996043 ) ) ;
#16401 = EDGE_CURVE ( 'NONE', #5736, #17991, #30776, .T. ) ;
#16402 = DIRECTION ( 'NONE',  ( 0.000000000000000000, 0.000000000000000000, 1.000000000000000000 ) ) ;
#16403 = CARTESIAN_POINT ( 'NONE',  ( 2.039164074698236906, -5.746172002732055084, -30.25632401680000783 ) ) ;
#16404 = VERTEX_POINT ( 'NONE', #28544 ) ;
#16405 = SHAPE_REPRESENTATION ( 'Drive Spring', ( #17722 ), #11232 ) ;
#16406 = CARTESIAN_POINT ( 'NONE',  ( -19.80526803560000104, 19.50877411510000314, 227.0000000000000000 ) ) ;
#16407 = CARTESIAN_POINT ( 'NONE',  ( 13.46591332798936236, 21.70000000000094786, -56.74462838232277306 ) ) ;
#16408 = ORIENTED_EDGE ( 'NONE', *, *, #14020, .T. ) ;
#16409 = EDGE_LOOP ( 'NONE', ( #21567, #16058, #23998, #19117 ) ) ;
#16410 = ORIENTED_EDGE ( 'NONE', *, *, #21521, .F. ) ;
#16411 =( NAMED_UNIT ( * ) PLANE_ANGLE_UNIT ( ) SI_UNIT ( $, .RADIAN. ) );
#16412 = ORIENTED_EDGE ( 'NONE', *, *, #3370, .F. ) ;
#16413 = FACE_OUTER_BOUND ( 'NONE', #25193, .T. ) ;
#16414 = CYLINDRICAL_SURFACE ( 'NONE', #609, 1.099999999999999867 ) ;
#16415 = CARTESIAN_POINT ( 'NONE',  ( -1.449312944839797890, 3.998683954144016894, -69.15099036452500059 ) ) ;
#16416 = CARTESIAN_POINT ( 'NONE',  ( 20.62869472290000061, -20.76074184889999685, 229.2930768649999891 ) ) ;
#16417 = B_SPLINE_CURVE_WITH_KNOTS ( 'NONE', 5,
 ( #9969, #26795, #16577, #26185, #22235, #14999, #3641, #5697, #17647 ),
 .UNSPECIFIED., .F., .F.,
 ( 6, 3, 6 ),
 ( 0.000000000000000000, 53.20205529499999386, 91.13698440880000362 ),
 .UNSPECIFIED. ) ;
#16418 = APPLICATION_CONTEXT ( 'automotive_design' ) ;
#16419 = CARTESIAN_POINT ( 'NONE',  ( 6.438687372205746051, -7.245008774379918748, -33.94554228741176161 ) ) ;
#16420 = CARTESIAN_POINT ( 'NONE',  ( -0.9776373403070000023, -28.64054450000000074, 222.0000000000000000 ) ) ;
#16421 = CARTESIAN_POINT ( 'NONE',  ( 5.239171942370466795, -0.3666422309894779019, -35.69999999999999574 ) ) ;
#16422 = VERTEX_POINT ( 'NONE', #26038 ) ;
#16423 = CARTESIAN_POINT ( 'NONE',  ( -22.71519155902493381, -14.22192772757401258, 225.5575347055555255 ) ) ;
#16424 = CARTESIAN_POINT ( 'NONE',  ( -3.711147652395973662, 4.588201686596787177, -12.60352819870001184 ) ) ;
#16425 = CARTESIAN_POINT ( 'NONE',  ( -7.999999999695856623, -18.27877680370596636, -30.94409471158115110 ) ) ;
#16426 = EDGE_CURVE ( 'NONE', #453, #4391, #15706, .T. ) ;
#16427 = CARTESIAN_POINT ( 'NONE',  ( 4.456723356677985137, -11.49589600330395989, 232.6627637151898966 ) ) ;
#16428 = VERTEX_POINT ( 'NONE', #23377 ) ;
#16429 = FACE_OUTER_BOUND ( 'NONE', #4687, .T. ) ;
#16430 = CARTESIAN_POINT ( 'NONE',  ( 1.632956991020356519, -28.45346066249067007, 4.791883387999989807 ) ) ;
#16431 = CARTESIAN_POINT ( 'NONE',  ( 3.040504021322313122, 1.733590290792417887, 0.000000000000000000 ) ) ;
#16432 = LINE ( 'NONE', #17012, #20699 ) ;
#16433 = EDGE_CURVE ( 'NONE', #2249, #18378, #26189, .T. ) ;
#16434 = DIRECTION ( 'NONE',  ( -0.9316362575375349842, 0.3633921898465292122, -0.000000000000000000 ) ) ;
#16435 = EDGE_CURVE ( 'NONE', #28713, #9163, #10101, .T. ) ;
#16436 = FACE_OUTER_BOUND ( 'NONE', #24781, .T. ) ;
#16437 = DIRECTION ( 'NONE',  ( -1.000000000000000000, 5.665498452320000818E-16, 0.000000000000000000 ) ) ;
#16439 = EDGE_CURVE ( 'NONE', #28570, #19740, #19712, .T. ) ;
#16438 = CARTESIAN_POINT ( 'NONE',  ( 8.000000000250640397, -26.29778505802628885, -31.34318562232667915 ) ) ;
#16440 = ORIENTED_EDGE ( 'NONE', *, *, #3929, .F. ) ;
#16441 = CARTESIAN_POINT ( 'NONE',  ( 10.69999999989999928, -25.00000000000000000, -14.32712675259999813 ) ) ;
#16442 = DIRECTION ( 'NONE',  ( 0.000000000000000000, -1.000000000000000000, 0.000000000000000000 ) ) ;
#16443 = CARTESIAN_POINT ( 'NONE',  ( 2.333807673937585925, -4.208960876372860760, -68.10000000002503384 ) ) ;
#16444 = VECTOR ( 'NONE', #15292, 1000.000000000000000 ) ;
#16445 = CARTESIAN_POINT ( 'NONE',  ( -11.69999999989999928, -2.500000000000002220, -2.399999999999999467 ) ) ;
#16446 = DIRECTION ( 'NONE',  ( -5.962915006522622422E-16, -0.4383711467890810676, -0.8987940462991651502 ) ) ;
#16447 = ORIENTED_EDGE ( 'NONE', *, *, #2934, .F. ) ;
#16448 = CARTESIAN_POINT ( 'NONE',  ( 27.92857142909999979, -3.420150602509999660E-15, 37.93968498519999599 ) ) ;
#16449 = CARTESIAN_POINT ( 'NONE',  ( 1.644051155559919764, -5.677575162961061572, -68.18367649352499882 ) ) ;
#16450 = ORIENTED_EDGE ( 'NONE', *, *, #30180, .T. ) ;
#16451 = CARTESIAN_POINT ( 'NONE',  ( -249983.7073439999076, 207571.5457919999899, 379978.1891180000966 ) ) ;
#16452 = CARTESIAN_POINT ( 'NONE',  ( -18.92356980859999993, 19.72862807099999927, 229.8505673220000176 ) ) ;
#16453 = ORIENTED_EDGE ( 'NONE', *, *, #5154, .F. ) ;
#16454 = DIRECTION ( 'NONE',  ( 0.7600087925169251024, 0.4151946956549595336, -0.4999999999969509945 ) ) ;
#16455 = CARTESIAN_POINT ( 'NONE',  ( 0.2860395612620135197, -27.49884598709296668, 223.9280906791276493 ) ) ;
#16456 = CARTESIAN_POINT ( 'NONE',  ( 27.23548387180000319, -3.335274659869999873E-15, 41.66046017409999536 ) ) ;
#16457 = DIRECTION ( 'NONE',  ( 1.000000000000000000, 6.668066630619518976E-24, -2.257150022442225012E-12 ) ) ;
#16458 = VECTOR ( 'NONE', #15553, 1000.000000000000000 ) ;
#16459 = CARTESIAN_POINT ( 'NONE',  ( 10.00000000000000000, -130.0000000000000000, -41.82335799894999440 ) ) ;
#16460 = DIRECTION ( 'NONE',  ( 0.000000000000000000, 0.000000000000000000, -1.000000000000000000 ) ) ;
#16461 = VERTEX_POINT ( 'NONE', #1814 ) ;
#16462 = CARTESIAN_POINT ( 'NONE',  ( 24.49999999589999788, -3.000285566359999846E-15, 90.00000000000000000 ) ) ;
#16463 = CARTESIAN_POINT ( 'NONE',  ( 24.43762869010000216, -14.66515636309999948, 226.0027499809999938 ) ) ;
#16464 = LINE ( 'NONE', #18366, #25871 ) ;
#16465 = CARTESIAN_POINT ( 'NONE',  ( -26.95773186790000153, 8.656139590820000507, 224.8000000000000114 ) ) ;
#16466 = CARTESIAN_POINT ( 'NONE',  ( 8.700000000231835173, -28.43890284012990577, -25.73830582827173785 ) ) ;
#16467 = CARTESIAN_POINT ( 'NONE',  ( -0.3831792618880000556, -28.49793954440000121, 226.0423263479999889 ) ) ;
#16468 = CONICAL_SURFACE ( 'NONE', #30027, 0.9999999999991034949, 0.7853981633970000820 ) ;
#16469 = CARTESIAN_POINT ( 'NONE',  ( -24.50348397099046593, 13.13223627435659857, 3.957489296000010981 ) ) ;
#16470 = CYLINDRICAL_SURFACE ( 'NONE', #8571, 1.100000000000002309 ) ;
#16471 = CARTESIAN_POINT ( 'NONE',  ( -4.541600168151706640, -0.1148504950298593758, -53.15673954922500144 ) ) ;
#16472 = CARTESIAN_POINT ( 'NONE',  ( -8.000000000474178918, -29.73863906514523947, -27.17531388891475075 ) ) ;
#16473 = CARTESIAN_POINT ( 'NONE',  ( -27.71720220739999974, -1.978370540369999998E-11, 229.4485730569999760 ) ) ;
#16474 = CARTESIAN_POINT ( 'NONE',  ( 3.187192794176077815, -1.479400473301520913, 230.8301842479609149 ) ) ;
#16475 = VERTEX_POINT ( 'NONE', #28698 ) ;
#16476 = CIRCLE ( 'NONE', #10957, 26.80000000000000071 ) ;
#16477 = CARTESIAN_POINT ( 'NONE',  ( -12.24455124192851407, 21.69999999999989626, -55.78348256257161353 ) ) ;
#16478 = CARTESIAN_POINT ( 'NONE',  ( 10.69999999997499351, -26.21515828619547861, -31.32227941849448882 ) ) ;
#16479 = EDGE_CURVE ( 'NONE', #10036, #26756, #9160, .T. ) ;
#16480 = CARTESIAN_POINT ( 'NONE',  ( -0.9606962270921406422, -4.447130805931738706, -55.93033560642499680 ) ) ;
#16481 = EDGE_LOOP ( 'NONE', ( #25317, #9810, #8294, #1744 ) ) ;
#16482 = CIRCLE ( 'NONE', #16977, 26.80000000000000071 ) ;
#16483 = ORIENTED_EDGE ( 'NONE', *, *, #14557, .T. ) ;
#16485 = CARTESIAN_POINT ( 'NONE',  ( -17.42785659857645086, -30.42600657595649949, -32.19550051884773012 ) ) ;
#16484 = AXIS2_PLACEMENT_3D ( 'NONE', #7248, #21891, #24398 ) ;
#16486 = ORIENTED_EDGE ( 'NONE', *, *, #27010, .T. ) ;
#16487 = CARTESIAN_POINT ( 'NONE',  ( 14.81460958102700332, -30.17431306372085231, -24.45952979736321353 ) ) ;
#16488 = EDGE_CURVE ( 'NONE', #1557, #27319, #7475, .T. ) ;
#16489 = DIRECTION ( 'NONE',  ( 0.000000000000000000, 0.3420201433259318913, -0.9396926207858126157 ) ) ;
#16490 = LINE ( 'NONE', #6884, #8915 ) ;
#16491 = PRODUCT_DEFINITION_SHAPE ( 'NONE', 'NONE',  #31136 ) ;
#16492 = CARTESIAN_POINT ( 'NONE',  ( -10.82908725742657730, -27.76276047461854901, 186.7828584120000244 ) ) ;
#16493 = CARTESIAN_POINT ( 'NONE',  ( 20.30396079662882158, 20.00000000004802203, 3.000000000000002665 ) ) ;
#16494 = DIRECTION ( 'NONE',  ( 9.219210260491733511E-13, 0.9128796883888953273, -0.4082287037029530552 ) ) ;
#16495 = CARTESIAN_POINT ( 'NONE',  ( 0.1879441846346346090, 4.794077236920960772, -7.000190181100000686 ) ) ;
#16496 = CARTESIAN_POINT ( 'NONE',  ( 5.361384718760000112, -31.61859215129999967, 229.2404163060000144 ) ) ;
#16497 = ORIENTED_EDGE ( 'NONE', *, *, #14009, .F. ) ;
#16498 = CARTESIAN_POINT ( 'NONE',  ( -24.34159889609999894, -14.82483853620000147, 224.0986003170000060 ) ) ;
#16499 = CIRCLE ( 'NONE', #12991, 4.000000004070001225 ) ;
#16500 = CARTESIAN_POINT ( 'NONE',  ( -2.345194346458620682, -4.011532291445383258, -15.68182079290000175 ) ) ;
#16501 = CARTESIAN_POINT ( 'NONE',  ( 26.33366376410667797, 9.374780377579124746, 8.000000000000007105 ) ) ;
#16502 = B_SPLINE_CURVE_WITH_KNOTS ( 'NONE', 1,
 ( #25326, #8471 ),
 .UNSPECIFIED., .F., .F.,
 ( 2, 2 ),
 ( -2.556331278550000249E-06, 0.7000000000009999335 ),
 .UNSPECIFIED. ) ;
#16503 = CARTESIAN_POINT ( 'NONE',  ( -10.00404318770000067, -25.00000000000000000, -2.271680403899995149 ) ) ;
#16504 = AXIS2_PLACEMENT_3D ( 'NONE', #4101, #2216, #1749 ) ;
#16505 = CARTESIAN_POINT ( 'NONE',  ( 23.05336736746781767, -19.64267831869096881, -0.6577119969999878357 ) ) ;
#16506 = DIRECTION ( 'NONE',  ( 0.000000000000000000, -1.000000000000000000, 2.257145581549999994E-12 ) ) ;
#16507 = DIRECTION ( 'NONE',  ( -1.000000000000000000, 0.000000000000000000, 0.000000000000000000 ) ) ;
#16508 = CARTESIAN_POINT ( 'NONE',  ( -19.68703433251029722, 19.53817007346649248, 0.6302326600000074386 ) ) ;
#16509 = CARTESIAN_POINT ( 'NONE',  ( 7.000000000277405654, -5.572998883592096497, -27.02754848641193419 ) ) ;
#16510 = CARTESIAN_POINT ( 'NONE',  ( 3.387192064160615690, -0.9942423616359961080, 226.6412452697750268 ) ) ;
#16511 = CARTESIAN_POINT ( 'NONE',  ( 0.000000000000000000, -17.25771824150000100, 5.000000000000000000 ) ) ;
#16512 = VECTOR ( 'NONE', #223, 1000.000000000000000 ) ;
#16513 = ADVANCED_FACE ( 'NONE', ( #4324 ), #13922, .F. ) ;
#16514 = CARTESIAN_POINT ( 'NONE',  ( -3.484426971583858279, -2.194289969034543208, -69.67698578303701140 ) ) ;
#16515 = VERTEX_POINT ( 'NONE', #29004 ) ;
#16516 = CYLINDRICAL_SURFACE ( 'NONE', #3198, 2.999999999999999556 ) ;
#16517 = CARTESIAN_POINT ( 'NONE',  ( 10.79293894529999953, 19.99999999999999645, -1.960370163500001262 ) ) ;
#16518 = FACE_OUTER_BOUND ( 'NONE', #23775, .T. ) ;
#16519 = EDGE_LOOP ( 'NONE', ( #4786, #17202, #23508, #21100 ) ) ;
#16520 = CARTESIAN_POINT ( 'NONE',  ( -1.877135327876712667, -5.132840123261955156, -44.78640794712499940 ) ) ;
#16521 = ORIENTED_EDGE ( 'NONE', *, *, #27513, .F. ) ;
#16522 = EDGE_LOOP ( 'NONE', ( #10352, #27428, #28105, #27690, #28842 ) ) ;
#16523 = VECTOR ( 'NONE', #13756, 1000.000000000000000 ) ;
#16524 = CARTESIAN_POINT ( 'NONE',  ( 0.000000000000000000, 0.000000000000000000, 0.000000000000000000 ) ) ;
#16525 = VERTEX_POINT ( 'NONE', #8054 ) ;
#16526 = DIRECTION ( 'NONE',  ( 0.000000000000000000, 0.000000000000000000, 1.000000000000000000 ) ) ;
#16527 = ORIENTED_EDGE ( 'NONE', *, *, #1863, .T. ) ;
#16528 = DIRECTION ( 'NONE',  ( 1.224606353819999829E-16, 1.000000000000000000, 0.000000000000000000 ) ) ;
#16529 = CARTESIAN_POINT ( 'NONE',  ( 24.29089620522634263, 14.90695587088477581, 3.920145809000019632 ) ) ;
#16530 = EDGE_CURVE ( 'NONE', #17371, #8301, #11992, .T. ) ;
#16531 = CARTESIAN_POINT ( 'NONE',  ( -23.87963657974984955, -15.55698410977798929, 4.493007575000013354 ) ) ;
#16532 = CARTESIAN_POINT ( 'NONE',  ( 0.2440535278923537388, 4.404678305699071927, -35.69999999999998863 ) ) ;
#16533 = DIRECTION ( 'NONE',  ( 0.3633921898465272138, -0.9316362575375356503, 1.850371707708593498E-14 ) ) ;
#16534 = AXIS2_PLACEMENT_3D ( 'NONE', #7342, #19452, #24330 ) ;
#16535 = PLANE ( 'NONE',  #28102 ) ;
#16536 = FACE_OUTER_BOUND ( 'NONE', #12387, .T. ) ;
#16537 = FACE_OUTER_BOUND ( 'NONE', #16945, .T. ) ;
#16538 = B_SPLINE_CURVE_WITH_KNOTS ( 'NONE', 3,
 ( #16057, #30385, #13381, #11494, #8811, #21097, #9120, #1435, #20619, #11341, #27693, #30217, #8649, #6608 ),
 .UNSPECIFIED., .F., .F.,
 ( 4, 2, 2, 2, 2, 2, 4 ),
 ( 0.000000000000000000, 0.2500000000000027756, 0.3750000000000041078, 0.4375000000000041633, 0.5000000000000042188, 0.7500000000000022204, 1.000000000000000000 ),
 .UNSPECIFIED. ) ;
#16539 = CARTESIAN_POINT ( 'NONE',  ( -2.150134890876696847, -3.785840986416655340, -7.185065142700006291 ) ) ;
#16540 = CARTESIAN_POINT ( 'NONE',  ( 1.984841800599668638, 5.152205253018144582, -25.09462237480000368 ) ) ;
#16541 = CARTESIAN_POINT ( 'NONE',  ( -23.20948082139999968, -13.40000000000000036, 223.8999999999999773 ) ) ;
#16542 = EDGE_CURVE ( 'NONE', #30146, #3507, #30393, .T. ) ;
#16543 = CARTESIAN_POINT ( 'NONE',  ( 24.36724935763797006, 13.38201651305720574, 4.999998581000003384 ) ) ;
#16544 = CARTESIAN_POINT ( 'NONE',  ( -24.93720648713954446, 13.79881813474513486, 6.099998581000020792 ) ) ;
#16545 = CARTESIAN_POINT ( 'NONE',  ( 1.387648159808060999, -4.113210426322157609, -15.26414732020000464 ) ) ;
#16546 = EDGE_CURVE ( 'NONE', #22644, #9824, #14545, .T. ) ;
#16547 = CARTESIAN_POINT ( 'NONE',  ( 18.06288090037109839, 10.34626908989090133, -1.400000000000002132 ) ) ;
#16548 = CARTESIAN_POINT ( 'NONE',  ( 0.6243462152986178904, -28.49342029039284085, 6.095948809000023338 ) ) ;
#16549 = CARTESIAN_POINT ( 'NONE',  ( -25.32382120361955913, -8.841433100612317020, -1.399999999999998579 ) ) ;
#16550 = ORIENTED_EDGE ( 'NONE', *, *, #15585, .F. ) ;
#16551 = ORIENTED_EDGE ( 'NONE', *, *, #25585, .F. ) ;
#16552 = DIRECTION ( 'NONE',  ( 0.000000000000000000, 0.7113488923935510355, -0.7028390664230811380 ) ) ;
#16553 = CYLINDRICAL_SURFACE ( 'NONE', #29883, 3.500000000000003109 ) ;
#16554 = CIRCLE ( 'NONE', #978, 3.491271820589999741 ) ;
#16555 = ORIENTED_EDGE ( 'NONE', *, *, #30982, .T. ) ;
#16556 = CARTESIAN_POINT ( 'NONE',  ( -5.797918471703387588, -5.490503403362547274, -26.84307236416243470 ) ) ;
#16557 = FACE_OUTER_BOUND ( 'NONE', #4860, .T. ) ;
#16558 = ORIENTED_EDGE ( 'NONE', *, *, #12253, .T. ) ;
#16559 = VERTEX_POINT ( 'NONE', #7900 ) ;
#16560 = VERTEX_POINT ( 'NONE', #7601 ) ;
#16561 =( NAMED_UNIT ( * ) PLANE_ANGLE_UNIT ( ) SI_UNIT ( $, .RADIAN. ) );
#16562 = ORIENTED_EDGE ( 'NONE', *, *, #17928, .T. ) ;
#16563 = B_SPLINE_CURVE_WITH_KNOTS ( 'NONE', 3,
 ( #23501, #16241, #19502, #23654, #16976, #24217, #30726, #21280 ),
 .UNSPECIFIED., .F., .F.,
 ( 4, 2, 2, 4 ),
 ( 0.000000000000000000, 0.2499999999999998890, 0.4999999999999997780, 1.000000000000000000 ),
 .UNSPECIFIED. ) ;
#16564 = CARTESIAN_POINT ( 'NONE',  ( -17.49999999969999820, -24.38109793998400932, -29.91497134778435907 ) ) ;
#16565 = EDGE_CURVE ( 'NONE', #16141, #10785, #546, .T. ) ;
#16566 = FACE_OUTER_BOUND ( 'NONE', #18724, .T. ) ;
#16567 = CARTESIAN_POINT ( 'NONE',  ( 0.2945360517547964130, 4.690762039826936736, -68.55875473022499023 ) ) ;
#16568 = EDGE_LOOP ( 'NONE', ( #8492, #12347, #7500, #12884, #18207, #14941, #17138, #10291, #3499, #2565 ) ) ;
#16569 = CARTESIAN_POINT ( 'NONE',  ( 19.90445648569999904, -20.03186682420000153, 230.0000000000000000 ) ) ;
#16570 = DIRECTION ( 'NONE',  ( 1.347073341475313442E-12, -0.9800962620158550909, -0.1985228379369698981 ) ) ;
#16571 = CARTESIAN_POINT ( 'NONE',  ( 27.16602884410000129, -9.122302432779999748, 222.0000000000000000 ) ) ;
#16572 = CARTESIAN_POINT ( 'NONE',  ( 3.534785842709389669, -3.329260007524329712, -0.6997833233010605225 ) ) ;
#16573 = ORIENTED_EDGE ( 'NONE', *, *, #4504, .F. ) ;
#16574 = EDGE_CURVE ( 'NONE', #8147, #11115, #10158, .T. ) ;
#16575 = CARTESIAN_POINT ( 'NONE',  ( 11.57608395239999943, -24.17108566339999953, -0.7028182531999965788 ) ) ;
#16576 = CARTESIAN_POINT ( 'NONE',  ( -2.345194346458620682, -4.011532291445383258, -15.68182079290000175 ) ) ;
#16577 = CARTESIAN_POINT ( 'NONE',  ( -23.10935684530000245, -20.42749692129999772, 228.9999999990000106 ) ) ;
#16578 = FACE_OUTER_BOUND ( 'NONE', #8816, .T. ) ;
#16579 = VERTEX_POINT ( 'NONE', #5242 ) ;
#16580 = CARTESIAN_POINT ( 'NONE',  ( 22.97596755210000197, 15.65128466780000061, 222.0000000000000000 ) ) ;
#16581 = DIRECTION ( 'NONE',  ( 0.000000000000000000, -2.257145581549999994E-12, -1.000000000000000000 ) ) ;
#16582 = CARTESIAN_POINT ( 'NONE',  ( -28.01992793520000191, 5.907563698139999708, 222.0000000000000000 ) ) ;
#16583 = CARTESIAN_POINT ( 'NONE',  ( 17.93011078763067090, 11.79183908526299085, -0.6999999999999784173 ) ) ;
#16584 = CARTESIAN_POINT ( 'NONE',  ( 1.100000000000000089, -26.77741585740000119, 225.0000000000000000 ) ) ;
#16585 = CYLINDRICAL_SURFACE ( 'NONE', #14740, 2.000000000000000444 ) ;
#16586 = CARTESIAN_POINT ( 'NONE',  ( 10.69999999997821583, -125.3091097352362056, -32.74879024719411547 ) ) ;
#16587 = ORIENTED_EDGE ( 'NONE', *, *, #26796, .F. ) ;
#16588 = CARTESIAN_POINT ( 'NONE',  ( -10.69999999999999929, -24.00003454060000152, -28.41820959990000262 ) ) ;
#16589 = CARTESIAN_POINT ( 'NONE',  ( 16.06937396340397939, -9.163977451780842998, -0.6999999999999784173 ) ) ;
#16590 = VECTOR ( 'NONE', #13992, 1000.000000000000000 ) ;
#16591 = DIRECTION ( 'NONE',  ( 1.000000000000000000, -1.843431230198065828E-12, 2.650498504953516580E-12 ) ) ;
#16592 = CARTESIAN_POINT ( 'NONE',  ( -4.854067883769174863, 0.05624032484770506712, -68.10000000002500542 ) ) ;
#16593 = B_SPLINE_CURVE_WITH_KNOTS ( 'NONE', 5,
 ( #8904, #4349, #9061, #1529, #11586, #13634 ),
 .UNSPECIFIED., .F., .F.,
 ( 6, 6 ),
 ( -2.319814964989999950, 0.000000000000000000 ),
 .UNSPECIFIED. ) ;
#16594 = CARTESIAN_POINT ( 'NONE',  ( 10.69999999999999929, -24.00000000000000000, -28.40000000000000213 ) ) ;
#16595 = CARTESIAN_POINT ( 'NONE',  ( 3.796508223180000030, 11.43135311160000001, 230.6412452697800006 ) ) ;
#16596 = ORIENTED_EDGE ( 'NONE', *, *, #3808, .F. ) ;
#16597 = LINE ( 'NONE', #9357, #9427 ) ;
#16598 = EDGE_CURVE ( 'NONE', #13120, #13901, #24600, .T. ) ;
#16599 = CARTESIAN_POINT ( 'NONE',  ( -5.606848515966891711, 1.848691355091094835, -69.22019511502500677 ) ) ;
#16600 = AXIS2_PLACEMENT_3D ( 'NONE', #13223, #20912, #30510 ) ;
#16601 = ORIENTED_EDGE ( 'NONE', *, *, #14195, .F. ) ;
#16602 = CARTESIAN_POINT ( 'NONE',  ( -7.999999999693439889, -7.565603753653322272, -31.48340496202311911 ) ) ;
#16603 = EDGE_CURVE ( 'NONE', #17295, #5944, #5086, .T. ) ;
#16604 = EDGE_CURVE ( 'NONE', #15836, #7991, #15001, .T. ) ;
#16605 = CARTESIAN_POINT ( 'NONE',  ( 1.387947292976102087, 4.364053279572885025, -60.46492395752500215 ) ) ;
#16606 = VERTEX_POINT ( 'NONE', #19413 ) ;
#16607 = CARTESIAN_POINT ( 'NONE',  ( -7.105427357599999217E-15, 0.000000000000000000, 86.78285841159998881 ) ) ;
#16608 = CARTESIAN_POINT ( 'NONE',  ( -24.41841039498785193, -14.69667350221323865, 3.899998581000013509 ) ) ;
#16609 = FACE_OUTER_BOUND ( 'NONE', #22689, .T. ) ;
#16610 = UNCERTAINTY_MEASURE_WITH_UNIT (LENGTH_MEASURE( 1.000000000000000082E-05 ), #5103, 'distance_accuracy_value', 'NONE');
#16611 = CARTESIAN_POINT ( 'NONE',  ( 10.82908725742653999, -27.76276047461857033, 86.78285841159998881 ) ) ;
#16612 = CARTESIAN_POINT ( 'NONE',  ( -6.000000000000000000, -29.27600094726834712, -81.66227801707495360 ) ) ;
#16613 = CARTESIAN_POINT ( 'NONE',  ( 8.700000000115439391, -60.75400889061209142, -3.446705952623797309 ) ) ;
#16614 = ORIENTED_EDGE ( 'NONE', *, *, #2412, .F. ) ;
#16615 = CARTESIAN_POINT ( 'NONE',  ( 24.93720649360215802, -13.79881813812812297, 6.099998581000020792 ) ) ;
#16616 = CARTESIAN_POINT ( 'NONE',  ( 24.15870318760000046, -15.11998207899999969, 225.5069924249999929 ) ) ;
#16617 = DIRECTION ( 'NONE',  ( 0.000000000000000000, 0.000000000000000000, 1.000000000000000000 ) ) ;
#16618 = CARTESIAN_POINT ( 'NONE',  ( -22.83911268609999823, 16.42879705509999866, 227.5999999999999943 ) ) ;
#16619 = CARTESIAN_POINT ( 'NONE',  ( 16.40303402077768169, -9.791839085275103827, -0.6999999999999784173 ) ) ;
#16620 = CARTESIAN_POINT ( 'NONE',  ( 3.550686852090000366E-05, -28.50022181210000127, 226.1000014189999945 ) ) ;
#16621 = LINE ( 'NONE', #11166, #13192 ) ;
#16622 = CARTESIAN_POINT ( 'NONE',  ( -24.78870452934888746, 12.58522324287992866, 4.492873454000012146 ) ) ;
#16623 = DIRECTION ( 'NONE',  ( 0.000000000000000000, 0.000000000000000000, 1.000000000000000000 ) ) ;
#16624 = CARTESIAN_POINT ( 'NONE',  ( 4.942443250116775211, -2.327596941721505441, -51.49872167392499733 ) ) ;
#16625 = AXIS2_PLACEMENT_3D ( 'NONE', #27455, #17397, #26846 ) ;
#16626 = CARTESIAN_POINT ( 'NONE',  ( 9.000000000000000000, 21.70000000000000284, -51.10000000017000588 ) ) ;
#16627 = DIRECTION ( 'NONE',  ( 0.000000000000000000, 0.000000000000000000, 1.000000000000000000 ) ) ;
#16628 = CARTESIAN_POINT ( 'NONE',  ( 24.83401022448529005, 13.98326749045440032, 5.760125282000011282 ) ) ;
#16629 = ORIENTED_EDGE ( 'NONE', *, *, #13726, .T. ) ;
#16630 = CARTESIAN_POINT ( 'NONE',  ( 10.89131017139999891, -24.73114799960000099, -1.811764705899998606 ) ) ;
#16631 = EDGE_LOOP ( 'NONE', ( #13026, #22949, #18017, #2663 ) ) ;
#16632 = CARTESIAN_POINT ( 'NONE',  ( -24.07583586439999834, -13.90018868249999962, 223.9000014189999774 ) ) ;
#16633 = CARTESIAN_POINT ( 'NONE',  ( -2.948077164825098517, -3.495793300896359312, -59.57407541852499833 ) ) ;
#16634 = VERTEX_POINT ( 'NONE', #7750 ) ;
#16635 = EDGE_CURVE ( 'NONE', #20468, #25887, #15691, .T. ) ;
#16636 = ORIENTED_EDGE ( 'NONE', *, *, #1150, .T. ) ;
#16637 = CARTESIAN_POINT ( 'NONE',  ( -17.46645031549716620, -30.09476775824673211, -32.38680219110657532 ) ) ;
#16638 = EDGE_CURVE ( 'NONE', #5682, #5141, #15332, .T. ) ;
#16639 = ORIENTED_EDGE ( 'NONE', *, *, #19706, .T. ) ;
#16640 = CARTESIAN_POINT ( 'NONE',  ( 20.30405755279999980, 20.00000000000000000, 229.0000000000000000 ) ) ;
#16641 = CARTESIAN_POINT ( 'NONE',  ( 8.699999999546083274, -16.84112679186181083, -33.19732076799427034 ) ) ;
#16642 = CARTESIAN_POINT ( 'NONE',  ( -3.063879268240000009, -1.673804873600000187, 227.6412452699999847 ) ) ;
#16643 = VECTOR ( 'NONE', #19494, 1000.000000000000114 ) ;
#16644 = DIRECTION ( 'NONE',  ( 1.000000000000000000, 0.000000000000000000, 0.000000000000000000 ) ) ;
#16645 = CARTESIAN_POINT ( 'NONE',  ( -27.08859402333795430, -0.4928875713624365495, 0.02487529600000981667 ) ) ;
#16646 = FACE_OUTER_BOUND ( 'NONE', #1014, .T. ) ;
#16647 = CARTESIAN_POINT ( 'NONE',  ( -3.866727543631055308, 3.949224786475222349, -3.568732180600000525 ) ) ;
#16648 = CARTESIAN_POINT ( 'NONE',  ( -22.27803938659999972, -19.69272062099999943, 230.6999999999999886 ) ) ;
#16649 = ORIENTED_EDGE ( 'NONE', *, *, #22688, .F. ) ;
#16650 = CARTESIAN_POINT ( 'NONE',  ( -2.624330064346227509, -4.375605581812514799, -44.10000000002499121 ) ) ;
#16651 = CARTESIAN_POINT ( 'NONE',  ( 5.503465972402116435, -2.627571514392686769, -20.88180150029999993 ) ) ;
#16652 = DIRECTION ( 'NONE',  ( -1.000000000000000000, 0.000000000000000000, -6.771000000000000128E-12 ) ) ;
#16653 = B_SPLINE_CURVE_WITH_KNOTS ( 'NONE', 5,
 ( #11720, #23693, #2127, #26199, #21321, #14090, #4636, #16736, #7154 ),
 .UNSPECIFIED., .F., .F.,
 ( 6, 3, 6 ),
 ( 0.000000000000000000, 1.646696146390000060, 2.782752057450000205 ),
 .UNSPECIFIED. ) ;
#16654 = CARTESIAN_POINT ( 'NONE',  ( 24.49999999589999788, -3.000285566359999846E-15, 40.00000000000000000 ) ) ;
#16655 = CARTESIAN_POINT ( 'NONE',  ( 0.000000000000000000, -15.86465192213301556, -74.65259062561435144 ) ) ;
#16656 = CARTESIAN_POINT ( 'NONE',  ( -4.945984810541346199, -1.782911138613007207, -43.66497819512500200 ) ) ;
#16657 = DIRECTION ( 'NONE',  ( 1.000000000000000000, -1.843431230208684678E-12, 2.650498504958264790E-12 ) ) ;
#16658 = CYLINDRICAL_SURFACE ( 'NONE', #25314, 3.000000000000000000 ) ;
#16659 = LINE ( 'NONE', #5165, #11789 ) ;
#16660 = EDGE_CURVE ( 'NONE', #13541, #17736, #19860, .T. ) ;
#16661 = DIRECTION ( 'NONE',  ( 0.000000000000000000, -0.9396926207858125046, -0.3420201433259318358 ) ) ;
#16662 = AXIS2_PLACEMENT_3D ( 'NONE', #5779, #27032, #15075 ) ;
#16663 = EDGE_LOOP ( 'NONE', ( #20465, #14375, #22464, #23297 ) ) ;
#16664 = CARTESIAN_POINT ( 'NONE',  ( 6.585786437629999490, -16.41511111490214603, -74.85294138696069410 ) ) ;
#16665 = CARTESIAN_POINT ( 'NONE',  ( -15.94126856070501930, -9.659453305974544435, -0.6999999999999783062 ) ) ;
#16666 = CARTESIAN_POINT ( 'NONE',  ( -7.999999999651500993, -14.33807524410660328, -37.46575453387659849 ) ) ;
#16667 = TOROIDAL_SURFACE ( 'NONE', #14167, 29.80000000000000071, 3.000000000000000000 ) ;
#16668 = ORIENTED_EDGE ( 'NONE', *, *, #14444, .T. ) ;
#16669 = AXIS2_PLACEMENT_3D ( 'NONE', #7810, #24193, #26702 ) ;
#16670 = DIRECTION ( 'NONE',  ( 0.3633921898465291567, 0.9316362575375349842, 0.000000000000000000 ) ) ;
#16671 = CARTESIAN_POINT ( 'NONE',  ( -3.917812474729757799, -3.807994372373406211, -48.00083066912500129 ) ) ;
#16672 = ORIENTED_EDGE ( 'NONE', *, *, #4497, .F. ) ;
#16673 = EDGE_LOOP ( 'NONE', ( #2633, #18924, #11538, #22073 ) ) ;
#16674 = CARTESIAN_POINT ( 'NONE',  ( 0.000000000000000000, 0.000000000000000000, 0.000000000000000000 ) ) ;
#16675 = ORIENTED_EDGE ( 'NONE', *, *, #17652, .T. ) ;
#16676 = DIRECTION ( 'NONE',  ( -3.133604487004501508E-12, -0.3568421334038989756, 0.9341647027306019258 ) ) ;
#16677 = ORIENTED_EDGE ( 'NONE', *, *, #9606, .F. ) ;
#16678 = CARTESIAN_POINT ( 'NONE',  ( 24.11883219139999923, -15.18335225210000061, 225.3105549429999996 ) ) ;
#16679 = CARTESIAN_POINT ( 'NONE',  ( -5.069890653733686747, -10.00948981598860854, -35.93502061437225592 ) ) ;
#16680 = CARTESIAN_POINT ( 'NONE',  ( -23.98258507372315051, -15.39789217239198571, 4.239862999000004962 ) ) ;
#16681 = CARTESIAN_POINT ( 'NONE',  ( 0.7667278788745763851, 4.120231142481624254, -35.70000000000000284 ) ) ;
#16682 = CARTESIAN_POINT ( 'NONE',  ( 20.02191110107359506, 20.00001381684630530, 0.1993976363602749657 ) ) ;
#16683 = CARTESIAN_POINT ( 'NONE',  ( -24.88589369081283920, 13.89120818323882922, 6.095967889000020179 ) ) ;
#16684 = CARTESIAN_POINT ( 'NONE',  ( -14.89999999913999851, -22.00000000000000000, -31.28675134614999820 ) ) ;
#16685 = AXIS2_PLACEMENT_3D ( 'NONE', #12829, #14728, #3066 ) ;
#16686 = CARTESIAN_POINT ( 'NONE',  ( -20.15234898259999952, 20.00000753509999996, 229.6283026800000187 ) ) ;
#16687 = CARTESIAN_POINT ( 'NONE',  ( -3.630162863991669209, -2.403661707492378508, -6.889929326000000742 ) ) ;
#16688 = CARTESIAN_POINT ( 'NONE',  ( 2.193772516446764076, 5.694542648089183423, -26.09462237480000724 ) ) ;
#16689 = CARTESIAN_POINT ( 'NONE',  ( 1.758512962375676780, -3.081546181689937658, 0.000000000000000000 ) ) ;
#16690 = CARTESIAN_POINT ( 'NONE',  ( 23.28210887557342446, -13.27420452015669738, 226.1000000000000227 ) ) ;
#16691 = CARTESIAN_POINT ( 'NONE',  ( 24.54452541844319668, 14.48555669908156851, 6.079852602000002548 ) ) ;
#16692 = LINE ( 'NONE', #4754, #22691 ) ;
#16693 = CARTESIAN_POINT ( 'NONE',  ( 0.7763070146520680836, 4.277613328189620923, -14.02400681850000197 ) ) ;
#16694 = EDGE_CURVE ( 'NONE', #16896, #16475, #13831, .T. ) ;
#16695 = DIRECTION ( 'NONE',  ( 0.2815395311429196301, 0.9595496299847262600, 0.000000000000000000 ) ) ;
#16696 = CARTESIAN_POINT ( 'NONE',  ( -1.014482461663960056, -3.499829073223180931, 230.7531903453067628 ) ) ;
#16697 = ORIENTED_EDGE ( 'NONE', *, *, #17883, .F. ) ;
#16698 = ADVANCED_FACE ( 'NONE', ( #1462 ), #31022, .T. ) ;
#16699 = DIRECTION ( 'NONE',  ( -1.000000000000000000, 5.063197467948052462E-16, -2.257212216284997029E-12 ) ) ;
#16700 = CARTESIAN_POINT ( 'NONE',  ( -6.228182343209494043, 0.8662545139425728014, -19.25159460730001371 ) ) ;
#16701 = ORIENTED_EDGE ( 'NONE', *, *, #30200, .T. ) ;
#16702 = DIRECTION ( 'NONE',  ( -0.7071067811842725037, -0.2886612846624971307, -0.6455034180701249014 ) ) ;
#16703 = FACE_OUTER_BOUND ( 'NONE', #11271, .T. ) ;
#16705 = ORIENTED_EDGE ( 'NONE', *, *, #4502, .T. ) ;
#16704 = AXIS2_PLACEMENT_3D ( 'NONE', #23723, #30367, #20761 ) ;
#16706 = ORIENTED_EDGE ( 'NONE', *, *, #8864, .T. ) ;
#16707 = EDGE_LOOP ( 'NONE', ( #27392, #15462, #9554, #8189 ) ) ;
#16708 = B_SPLINE_CURVE_WITH_KNOTS ( 'NONE', 5,
 ( #28768, #24068, #3736, #26575, #6904, #7065 ),
 .UNSPECIFIED., .F., .F.,
 ( 6, 6 ),
 ( -7.118285296629999870, 0.000000000000000000 ),
 .UNSPECIFIED. ) ;
#16709 = ORIENTED_EDGE ( 'NONE', *, *, #11604, .F. ) ;
#16710 = CARTESIAN_POINT ( 'NONE',  ( -17.49999999970000175, -25.16060904162269907, -30.80181682675910437 ) ) ;
#16711 = DIRECTION ( 'NONE',  ( 0.000000000000000000, 0.000000000000000000, -1.000000000000000000 ) ) ;
#16712 = EDGE_CURVE ( 'NONE', #12087, #7544, #21119, .T. ) ;
#16713 = CARTESIAN_POINT ( 'NONE',  ( 8.000000000000000000, -15.86465192213301556, -74.65259062561435144 ) ) ;
#16714 = VERTEX_POINT ( 'NONE', #23793 ) ;
#16715 = CARTESIAN_POINT ( 'NONE',  ( 18.95046173579999760, -18.95046173579999760, -2.842170943039999687E-14 ) ) ;
#16716 = CARTESIAN_POINT ( 'NONE',  ( 24.60328987762038366, -12.94293973087761707, 225.1457708194568852 ) ) ;
#16717 = CARTESIAN_POINT ( 'NONE',  ( -17.49268987145706689, -32.00023133968888089, -28.84848335963180332 ) ) ;
#16718 = CARTESIAN_POINT ( 'NONE',  ( 0.2462945485050000161, -28.49939181889999773, 226.0797949779999954 ) ) ;
#16719 = ORIENTED_EDGE ( 'NONE', *, *, #1764, .T. ) ;
#16720 = CARTESIAN_POINT ( 'NONE',  ( -19.67781185827837831, 20.00028292424892840, -0.1456647343256203542 ) ) ;
#16721 = CARTESIAN_POINT ( 'NONE',  ( 2.992916622598568388, -2.824380467281232487, -18.03565260999999964 ) ) ;
#16722 = DIRECTION ( 'NONE',  ( 1.000000000000000000, 0.000000000000000000, 0.000000000000000000 ) ) ;
#16723 = DIRECTION ( 'NONE',  ( 0.3633921898465272138, -0.9316362575375356503, -2.775557561562890089E-14 ) ) ;
#16724 = AXIS2_PLACEMENT_3D ( 'NONE', #13020, #17729, #20257 ) ;
#16725 = ORIENTED_EDGE ( 'NONE', *, *, #14494, .T. ) ;
#16726 = CARTESIAN_POINT ( 'NONE',  ( -23.53065194457538567, -14.80430352413842421, 4.036042474887940656 ) ) ;
#16727 = CARTESIAN_POINT ( 'NONE',  ( -23.50695179570000093, -14.84192241259999889, 225.0000014190000002 ) ) ;
#16728 = CARTESIAN_POINT ( 'NONE',  ( 22.63992238019999803, -14.34133587289999845, 5.000000000000000000 ) ) ;
#16729 = DIRECTION ( 'NONE',  ( 1.553705081258627072E-12, -0.7253743710120287291, 0.6883545756940268046 ) ) ;
#16730 = LINE ( 'NONE', #14550, #10688 ) ;
#16731 = ADVANCED_FACE ( 'NONE', ( #6633 ), #28658, .T. ) ;
#16732 = FACE_OUTER_BOUND ( 'NONE', #8303, .T. ) ;
#16733 = CARTESIAN_POINT ( 'NONE',  ( 10.69999999999999929, -120.5233595624000174, -31.26042064949999855 ) ) ;
#16734 = EDGE_LOOP ( 'NONE', ( #3248, #21624, #1175, #25313 ) ) ;
#16735 = PLANE ( 'NONE',  #16300 ) ;
#16736 = CARTESIAN_POINT ( 'NONE',  ( -7.999999999660801109, -18.34164001289334678, -36.27507178818978417 ) ) ;
#16737 = B_SPLINE_CURVE_WITH_KNOTS ( 'NONE', 3,
 ( #16728, #12021, #14547, #29156, #231, #14697, #17196, #19105, #9818, #28845, #16891, #19415, #31066, #26496 ),
 .UNSPECIFIED., .F., .F.,
 ( 4, 2, 2, 2, 2, 2, 4 ),
 ( 0.000000000000000000, 0.2500000000000003886, 0.3750000000000010547, 0.4375000000000007772, 0.5000000000000005551, 0.7500000000000002220, 1.000000000000000000 ),
 .UNSPECIFIED. ) ;
#16738 = CARTESIAN_POINT ( 'NONE',  ( -27.85770179432011417, 4.285683232258365116, 0.7069222069999991920 ) ) ;
#16739 = CARTESIAN_POINT ( 'NONE',  ( 9.999999999945847762, -28.83786139299247608, -19.12343975076440827 ) ) ;
#16740 = VECTOR ( 'NONE', #5853, 1000.000000000000000 ) ;
#16741 = ORIENTED_EDGE ( 'NONE', *, *, #9104, .T. ) ;
#16742 = EDGE_CURVE ( 'NONE', #14204, #22999, #6689, .T. ) ;
#16743 = VECTOR ( 'NONE', #7149, 1000.000000000000114 ) ;
#16744 = CARTESIAN_POINT ( 'NONE',  ( -0.5632927345598660596, 3.521042344314967210, -88.52261276241718235 ) ) ;
#16745 = PRODUCT_DEFINITION_SHAPE ( 'NONE', 'NONE',  #31138 ) ;
#16746 = FILL_AREA_STYLE ('',( #16904 ) ) ;
#16747 = AXIS2_PLACEMENT_3D ( 'NONE', #5985, #13537, #18088 ) ;
#16748 = ORIENTED_EDGE ( 'NONE', *, *, #23688, .F. ) ;
#16749 = CARTESIAN_POINT ( 'NONE',  ( 23.83437493589245193, 15.62616282937172940, 5.290530241274704615 ) ) ;
#16750 = CIRCLE ( 'NONE', #3185, 2.999999999999997780 ) ;
#16751 = CARTESIAN_POINT ( 'NONE',  ( 1.644051155559919764, -5.677575162961061572, -67.70367649352500905 ) ) ;
#16752 = ORIENTED_EDGE ( 'NONE', *, *, #28936, .T. ) ;
#16753 = CARTESIAN_POINT ( 'NONE',  ( 1.723678405763061194, 4.474283509182772178, -27.03212237480000013 ) ) ;
#16754 = CYLINDRICAL_SURFACE ( 'NONE', #19947, 1.099999999999999201 ) ;
#16755 = B_SPLINE_CURVE_WITH_KNOTS ( 'NONE', 3,
 ( #1058, #910, #456, #12693, #19940, #29529, #15213, #17568, #29215, #26869, #27175, #17711 ),
 .UNSPECIFIED., .F., .F.,
 ( 4, 2, 2, 2, 2, 4 ),
 ( 0.000000000000000000, 0.2500000000000010547, 0.5000000000000021094, 0.6250000000000016653, 0.7500000000000011102, 1.000000000000000000 ),
 .UNSPECIFIED. ) ;
#16756 = ADVANCED_FACE ( 'NONE', ( #1773, #28348, #6793, #4583, #25996, #31023 ), #16390, .F. ) ;
#16757 = CARTESIAN_POINT ( 'NONE',  ( -3.985743628842679076, -2.180176701716177057, -53.34982952342500084 ) ) ;
#16758 = CARTESIAN_POINT ( 'NONE',  ( 20.30405755279999980, 20.00000000000000000, 226.9999998930000231 ) ) ;
#16759 = CARTESIAN_POINT ( 'NONE',  ( 1.099929244070992018, -27.47799402545701852, 224.8543268301346814 ) ) ;
#16760 = CARTESIAN_POINT ( 'NONE',  ( 24.02382125689999981, -13.98923529139999999, 223.9040349389999847 ) ) ;
#16761 = LINE ( 'NONE', #7481, #17826 ) ;
#16762 = AXIS2_PLACEMENT_3D ( 'NONE', #3983, #13737, #4302 ) ;
#16763 = DIRECTION ( 'NONE',  ( 0.000000000000000000, -2.257145581549999994E-12, -1.000000000000000000 ) ) ;
#16764 = ORIENTED_EDGE ( 'NONE', *, *, #28591, .T. ) ;
#16765 = CARTESIAN_POINT ( 'NONE',  ( 3.162069896769252875, -2.100311282821142100, -35.69999999999999574 ) ) ;
#16766 = VECTOR ( 'NONE', #16167, 1000.000000000000000 ) ;
#16767 = AXIS2_PLACEMENT_3D ( 'NONE', #3420, #17433, #22477 ) ;
#16768 = DIRECTION ( 'NONE',  ( 1.000000000000000000, -0.000000000000000000, -2.257150022439999944E-12 ) ) ;
#16769 = CARTESIAN_POINT ( 'NONE',  ( -26.95773186790000153, 8.656139628340000058, 222.0000000000000000 ) ) ;
#16770 = PLANE ( 'NONE',  #6104 ) ;
#16771 = AXIS2_PLACEMENT_3D ( 'NONE', #25399, #23932, #28057 ) ;
#16772 = CARTESIAN_POINT ( 'NONE',  ( -0.9902521520840001923, -27.78273347009999839, 225.5064930660000186 ) ) ;
#16773 = CARTESIAN_POINT ( 'NONE',  ( -19.80526744909999692, 19.50877353739999975, 229.0000000010000178 ) ) ;
#16774 = EDGE_CURVE ( 'NONE', #28706, #18380, #10489, .T. ) ;
#16775 = CARTESIAN_POINT ( 'NONE',  ( -24.98823330661245379, 13.70626928206978690, 3.904029301000005781 ) ) ;
#16776 = CARTESIAN_POINT ( 'NONE',  ( -5.114250173070000294, -17.43050732980000106, 230.0000000000000000 ) ) ;
#16777 = EDGE_CURVE ( 'NONE', #16560, #10061, #24753, .T. ) ;
#16778 = B_SPLINE_SURFACE_WITH_KNOTS ( 'NONE', 5, 5, ( 
 ( #3360, #5572, #22724, #24623, #15633, #15171, #3056, #718, #24776 ),
 ( #12967, #25086, #17982, #5876, #22577, #29650, #25244, #7927, #10152 ),
 ( #1021, #19749, #12653, #3211, #8079, #12819, #10309, #867, #3516 ),
 ( #13115, #22111, #10460, #1170, #17672, #29332, #10609, #17376, #27285 ),
 ( #5728, #26981, #29955, #20204, #5420, #10761, #29795, #27594, #16109 ),
 ( #1955, #15955, #25878, #23202, #4155, #30596, #11549, #27915, #6821 ) ),
 .UNSPECIFIED., .F., .F., .F.,
 ( 6, 6 ),
 ( 6, 3, 6 ),
 ( 0.000000000000000000, 24.33438218110000051 ),
 ( 8.011061266649999624, 9.372561696260000019, 10.73406212590000131 ),
 .UNSPECIFIED. ) ;
#16779 = CARTESIAN_POINT ( 'NONE',  ( -7.999999999729824118, -28.31424580201955621, -25.69835907506571715 ) ) ;
#16780 = CARTESIAN_POINT ( 'NONE',  ( 7.638583728930123939, 3.790177027337138238, -39.32776202378852304 ) ) ;
#16781 = CARTESIAN_POINT ( 'NONE',  ( 7.707106507606773960, -115.2381290211091738, 21.69251943803729787 ) ) ;
#16782 = ORIENTED_EDGE ( 'NONE', *, *, #4064, .T. ) ;
#16783 = EDGE_CURVE ( 'NONE', #29610, #28095, #14358, .T. ) ;
#16784 = DIRECTION ( 'NONE',  ( -0.9316362575375349842, 0.3633921898465292122, -0.000000000000000000 ) ) ;
#16785 = ORIENTED_EDGE ( 'NONE', *, *, #26769, .F. ) ;
#16786 = DIRECTION ( 'NONE',  ( 0.000000000000000000, -0.9128796883888953273, 0.4082287037029526666 ) ) ;
#16787 = AXIS2_PLACEMENT_3D ( 'NONE', #26654, #21942, #9823 ) ;
#16788 = CARTESIAN_POINT ( 'NONE',  ( -5.325262776965995926, 2.643762325383679279, -57.27877225282499296 ) ) ;
#16789 = CIRCLE ( 'NONE', #15785, 6.000000000000001776 ) ;
#16790 = VERTEX_POINT ( 'NONE', #14040 ) ;
#16791 = VECTOR ( 'NONE', #5826, 1000.000000000000000 ) ;
#16792 = VECTOR ( 'NONE', #10899, 1000.000000000000000 ) ;
#16793 = AXIS2_PLACEMENT_3D ( 'NONE', #8913, #15680, #25290 ) ;
#16794 = ORIENTED_EDGE ( 'NONE', *, *, #4587, .T. ) ;
#16795 = CYLINDRICAL_SURFACE ( 'NONE', #9579, 8.000000000000000000 ) ;
#16796 = VERTEX_POINT ( 'NONE', #14659 ) ;
#16797 =( NAMED_UNIT ( * ) SI_UNIT ( $, .STERADIAN. ) SOLID_ANGLE_UNIT ( ) );
#16798 = CARTESIAN_POINT ( 'NONE',  ( 18.26639035967037827, -8.979988381807324060, -0.6999999989999727834 ) ) ;
#16799 = CARTESIAN_POINT ( 'NONE',  ( 16.20123158649999695, 11.52736809289999620, -1.399999999999998579 ) ) ;
#16800 = LINE ( 'NONE', #6741, #27497 ) ;
#16801 = CARTESIAN_POINT ( 'NONE',  ( -20.30403093128963476, 20.00000000003735323, 1.400000021000019634 ) ) ;
#16802 = CARTESIAN_POINT ( 'NONE',  ( -1.641527485091622385, 5.277626912542655369, -3.774955258300002114 ) ) ;
#16803 = CARTESIAN_POINT ( 'NONE',  ( 17.16657240420000008, 10.97998838177520931, 0.5194763363741543571 ) ) ;
#16804 = EDGE_LOOP ( 'NONE', ( #25028, #27231, #19372, #30513 ) ) ;
#16805 = FACE_OUTER_BOUND ( 'NONE', #7807, .T. ) ;
#16806 = CARTESIAN_POINT ( 'NONE',  ( -19.80535357377644701, 19.50875577052588739, 3.000000106999994642 ) ) ;
#16807 = CARTESIAN_POINT ( 'NONE',  ( -6.228182343209494043, 0.8662545139425728014, -19.85159460730000092 ) ) ;
#16808 = CARTESIAN_POINT ( 'NONE',  ( -0.6677117243936687707, -27.79242653425564669, 225.8866279824144669 ) ) ;
#16809 = CARTESIAN_POINT ( 'NONE',  ( -25.84755624059999946, 9.037785233809998431, 230.6999999999999886 ) ) ;
#16810 = ADVANCED_FACE ( 'NONE', ( #19534 ), #7563, .F. ) ;
#16811 = CARTESIAN_POINT ( 'NONE',  ( -24.37165444408190851, 14.77472139917419369, 4.999998581000003384 ) ) ;
#16812 = DIRECTION ( 'NONE',  ( -1.000000000000000000, 5.665498452320000818E-16, 0.000000000000000000 ) ) ;
#16813 = CARTESIAN_POINT ( 'NONE',  ( -17.83930458829795640, 19.99999999999961631, -0.6999999999999784173 ) ) ;
#16814 = AXIS2_PLACEMENT_3D ( 'NONE', #7714, #19989, #8322 ) ;
#16815 = B_SPLINE_CURVE_WITH_KNOTS ( 'NONE', 3,
 ( #26783, #26477, #28680, #9325, #4919, #7585, #17180, #18927, #14376, #12314, #26326, #31047, #16710, #28525, #16564, #12458, #6976, #19398 ),
 .UNSPECIFIED., .F., .F.,
 ( 4, 2, 2, 2, 2, 2, 2, 2, 4 ),
 ( 0.000000000000000000, 0.1250000000000001665, 0.2500000000000003331, 0.3750000000000004996, 0.5000000000000006661, 0.6250000000000008882, 0.7500000000000005551, 0.8750000000000002220, 1.000000000000000000 ),
 .UNSPECIFIED. ) ;
#16816 = DIRECTION ( 'NONE',  ( -1.000000000000000000, 0.000000000000000000, 0.000000000000000000 ) ) ;
#16817 = EDGE_CURVE ( 'NONE', #4458, #8842, #19378, .T. ) ;
#16818 = CARTESIAN_POINT ( 'NONE',  ( 8.000000000647496279, -17.71277672293419769, -33.66803003880371392 ) ) ;
#16819 = CARTESIAN_POINT ( 'NONE',  ( 4.096142159599999388, 4.096142159599999388, 227.6412452697800006 ) ) ;
#16820 = EDGE_CURVE ( 'NONE', #12087, #18533, #348, .T. ) ;
#16821 = CARTESIAN_POINT ( 'NONE',  ( -10.00000000000000000, 21.70000000000000284, -62.10000000000000142 ) ) ;
#16822 = VERTEX_POINT ( 'NONE', #505 ) ;
#16823 = CARTESIAN_POINT ( 'NONE',  ( 8.700000000245104559, -24.05709603917588524, -27.69722300140832871 ) ) ;
#16824 =( REPRESENTATION_RELATIONSHIP ('NONE','NONE', #2712, #527 ) REPRESENTATION_RELATIONSHIP_WITH_TRANSFORMATION ( #26862 )SHAPE_REPRESENTATION_RELATIONSHIP( ) );
#16825 = DIRECTION ( 'NONE',  ( 1.000000000000000000, -8.856532914347465582E-13, 1.659169102000414711E-12 ) ) ;
#16826 = AXIS2_PLACEMENT_3D ( 'NONE', #5461, #7364, #7660 ) ;
#16827 = CARTESIAN_POINT ( 'NONE',  ( -7.999999999650268201, -15.05691661382650537, -37.86814300153927348 ) ) ;
#16828 = MECHANICAL_DESIGN_GEOMETRIC_PRESENTATION_REPRESENTATION (  '', ( #29380 ), #21358 ) ;
#16829 = VERTEX_POINT ( 'NONE', #5508 ) ;
#16830 = CARTESIAN_POINT ( 'NONE',  ( 24.83827472153076599, -12.48687851163286133, 4.895780544000027490 ) ) ;
#16831 = CARTESIAN_POINT ( 'NONE',  ( -0.6751951171115599948, 5.935132877056520151, -48.74410749642499496 ) ) ;
#16832 = ORIENTED_EDGE ( 'NONE', *, *, #3445, .F. ) ;
#16833 = ORIENTED_EDGE ( 'NONE', *, *, #4464, .F. ) ;
#16834 = CARTESIAN_POINT ( 'NONE',  ( 0.000000000000000000, 0.000000000000000000, 0.000000000000000000 ) ) ;
#16835 = ORIENTED_EDGE ( 'NONE', *, *, #6074, .F. ) ;
#16836 = B_SPLINE_CURVE_WITH_KNOTS ( 'NONE', 3,
 ( #11750, #11904, #24028, #2470, #117, #17085, #9696, #19301, #4977, #14588, #21820, #19453 ),
 .UNSPECIFIED., .F., .F.,
 ( 4, 2, 2, 2, 2, 4 ),
 ( 0.000000000000000000, 0.2499999999999878431, 0.4999999999999756861, 0.6249999999999715783, 0.7499999999999674705, 1.000000000000000000 ),
 .UNSPECIFIED. ) ;
#16837 = DIRECTION ( 'NONE',  ( 1.000000000000000000, 0.000000000000000000, 0.000000000000000000 ) ) ;
#16838 = ORIENTED_EDGE ( 'NONE', *, *, #26750, .T. ) ;
#16840 = CARTESIAN_POINT ( 'NONE',  ( 17.70481770901024632, 11.96970539787597509, -0.6999999999999785283 ) ) ;
#16839 = AXIS2_PLACEMENT_3D ( 'NONE', #2130, #244, #9827 ) ;
#16841 = DIRECTION ( 'NONE',  ( 0.000000000000000000, 0.000000000000000000, 1.000000000000000000 ) ) ;
#16842 = DIRECTION ( 'NONE',  ( -1.595945597898660305E-12, 0.7071067811865475727, 0.7071067811865475727 ) ) ;
#16843 = CARTESIAN_POINT ( 'NONE',  ( 0.2815792077273640004, 4.370109598415317542, -35.69999999999998863 ) ) ;
#16844 = DIRECTION ( 'NONE',  ( -1.000000000000000000, 5.687697913153403713E-16, -6.771501495041734442E-12 ) ) ;
#16845 = CARTESIAN_POINT ( 'NONE',  ( 9.499999999739312528, -17.84826627069900340, -36.91653688543832601 ) ) ;
#16846 = CARTESIAN_POINT ( 'NONE',  ( -5.732982782746885775, -7.779120688648472282, -33.68503850088168150 ) ) ;
#16847 = CARTESIAN_POINT ( 'NONE',  ( 17.18658402241074867, -10.09981795543446736, -1.000005633855494125E-09 ) ) ;
#16848 = EDGE_CURVE ( 'NONE', #28074, #27949, #12591, .T. ) ;
#16849 = CARTESIAN_POINT ( 'NONE',  ( -6.277996069133942925, 1.777976852108807737, -7.910827254899999161 ) ) ;
#16850 = CARTESIAN_POINT ( 'NONE',  ( 4.170003719754086013, -2.319039617606510006, -25.99287294500000201 ) ) ;
#16851 = CARTESIAN_POINT ( 'NONE',  ( 3.448453739143401808, -0.7497105383105261422, 0.000000000000000000 ) ) ;
#16852 = AXIS2_PLACEMENT_3D ( 'NONE', #15921, #11052, #23327 ) ;
#16853 =( GEOMETRIC_REPRESENTATION_CONTEXT ( 3 ) GLOBAL_UNCERTAINTY_ASSIGNED_CONTEXT ( ( #24164 ) ) GLOBAL_UNIT_ASSIGNED_CONTEXT ( ( #22994, #3796, #13543 ) ) REPRESENTATION_CONTEXT ( 'NONE', 'WORKASPACE' ) );
#16854 = CARTESIAN_POINT ( 'NONE',  ( 24.29138541237941240, -13.52003710528471281, 6.098655051000018368 ) ) ;
#16855 = CARTESIAN_POINT ( 'NONE',  ( 19.79257030269742756, 19.51192911135138175, 0.8505974720000031297 ) ) ;
#16856 = CARTESIAN_POINT ( 'NONE',  ( -2.345194346458620682, -4.011532291445383258, -15.68182079290000175 ) ) ;
#16857 = CARTESIAN_POINT ( 'NONE',  ( 16.76556712906763735, 9.965626860143510513, -1.400000000000002132 ) ) ;
#16858 = CARTESIAN_POINT ( 'NONE',  ( -24.47278419579111386, -14.60601539740217092, 3.904031772999999816 ) ) ;
#16859 = CARTESIAN_POINT ( 'NONE',  ( -17.49999999969999820, -24.60885018109999933, -24.02302961593000319 ) ) ;
#16860 = ORIENTED_EDGE ( 'NONE', *, *, #6098, .F. ) ;
#16861 = B_SPLINE_CURVE_WITH_KNOTS ( 'NONE', 5,
 ( #13653, #30172, #1698, #2015, #23258, #25627, #8602, #21053, #6258 ),
 .UNSPECIFIED., .F., .F.,
 ( 6, 3, 6 ),
 ( 8.011061266649999624, 8.831591450809998634, 9.652121634960000307 ),
 .UNSPECIFIED. ) ;
#16862 = CARTESIAN_POINT ( 'NONE',  ( 10.32522729140000095, -25.00000000000000000, -1.399999999999998579 ) ) ;
#16863 = CARTESIAN_POINT ( 'NONE',  ( 10.69999999999910933, -23.99999999999999645, -28.00730091825414902 ) ) ;
#16864 = ORIENTED_EDGE ( 'NONE', *, *, #27071, .F. ) ;
#16865 = LINE ( 'NONE', #21285, #25389 ) ;
#16866 = CARTESIAN_POINT ( 'NONE',  ( 22.97596238400000246, 15.65128114700000239, 222.0000000000000000 ) ) ;
#16867 = ORIENTED_EDGE ( 'NONE', *, *, #7961, .F. ) ;
#16868 = VERTEX_POINT ( 'NONE', #24246 ) ;
#16869 = ORIENTED_EDGE ( 'NONE', *, *, #20772, .F. ) ;
#16870 = VERTEX_POINT ( 'NONE', #7410 ) ;
#16871 = DIRECTION ( 'NONE',  ( 1.000000000000000000, 0.000000000000000000, 0.000000000000000000 ) ) ;
#16872 = DIRECTION ( 'NONE',  ( 0.000000000000000000, 0.000000000000000000, 1.000000000000000000 ) ) ;
#16873 = EDGE_CURVE ( 'NONE', #14390, #5681, #26761, .T. ) ;
#16874 = CARTESIAN_POINT ( 'NONE',  ( 17.93011078765611543, -8.208160914697428368, 0.000000000000000000 ) ) ;
#16875 = ORIENTED_EDGE ( 'NONE', *, *, #10020, .F. ) ;
#16876 = DIRECTION ( 'NONE',  ( 2.257144471330000330E-12, -0.000000000000000000, -1.000000000000000000 ) ) ;
#16877 = B_SPLINE_CURVE_WITH_KNOTS ( 'NONE', 3,
 ( #4895, #19369, #12277, #14955, #29260, #19677, #31014, #16845, #341, #14347 ),
 .UNSPECIFIED., .F., .F.,
 ( 4, 2, 2, 2, 4 ),
 ( 0.000000000000000000, 0.2500000000000000000, 0.5000000000000000000, 0.7500000000000000000, 1.000000000000000000 ),
 .UNSPECIFIED. ) ;
#16878 = CARTESIAN_POINT ( 'NONE',  ( 27.92857142820000149, 7.105427357599999217E-15, 142.0603150149999863 ) ) ;
#16879 = CARTESIAN_POINT ( 'NONE',  ( 19.68707593455170368, 19.53815609463533320, 0.6304112420000007599 ) ) ;
#16880 = FACE_OUTER_BOUND ( 'NONE', #21446, .T. ) ;
#16881 = CARTESIAN_POINT ( 'NONE',  ( 3.843630909669756957, -2.553018000905745044, -0.6999999999999992895 ) ) ;
#16882 = VERTEX_POINT ( 'NONE', #22198 ) ;
#16883 = ADVANCED_FACE ( 'NONE', ( #2688 ), #7615, .F. ) ;
#16884 = CARTESIAN_POINT ( 'NONE',  ( -18.31680438778779418, 19.99999316982339437, -0.6696325988070516155 ) ) ;
#16885 = CARTESIAN_POINT ( 'NONE',  ( 1.403799475828179766, 5.569137675590418723, -16.45080441500000745 ) ) ;
#16886 = CARTESIAN_POINT ( 'NONE',  ( -7.999999999650137639, -15.20668219507512653, -37.92535107952787854 ) ) ;
#16887 = CARTESIAN_POINT ( 'NONE',  ( 1.087565150579584028, -27.47889317205707727, 5.217914068007818429 ) ) ;
#16888 = ORIENTED_EDGE ( 'NONE', *, *, #22187, .T. ) ;
#16889 = CARTESIAN_POINT ( 'NONE',  ( 23.55447120710000064, 16.04539730700000177, 222.0000000000000000 ) ) ;
#16890 = CARTESIAN_POINT ( 'NONE',  ( 25.09775673860000467, 13.55753231799999980, 222.0000000000000000 ) ) ;
#16891 = CARTESIAN_POINT ( 'NONE',  ( 22.95800505923639534, -13.82601854777970729, 5.993195172372761448 ) ) ;
#16892 = DIRECTION ( 'NONE',  ( 0.000000000000000000, 0.000000000000000000, -1.000000000000000000 ) ) ;
#16893 = DIRECTION ( 'NONE',  ( 1.000000000000000000, 0.000000000000000000, 0.000000000000000000 ) ) ;
#16894 = CARTESIAN_POINT ( 'NONE',  ( 27.77512470410000134, 4.690278755559999624, 229.2930777930000090 ) ) ;
#16895 = FACE_OUTER_BOUND ( 'NONE', #21915, .T. ) ;
#16896 = VERTEX_POINT ( 'NONE', #17009 ) ;
#16897 = DIRECTION ( 'NONE',  ( 0.000000000000000000, 0.000000000000000000, -1.000000000000000000 ) ) ;
#16898 = CARTESIAN_POINT ( 'NONE',  ( 9.000000000000000000, -55.00000000000001421, -42.39999999999999858 ) ) ;
#16899 = CARTESIAN_POINT ( 'NONE',  ( 2.260959825389143862, -4.263672264598562300, -68.10000000002500542 ) ) ;
#16900 = CARTESIAN_POINT ( 'NONE',  ( 27.92857142860000152, 3.552713678799999608E-15, 92.06031501460000754 ) ) ;
#16901 = EDGE_CURVE ( 'NONE', #9520, #20613, #9617, .T. ) ;
#16902 = ORIENTED_EDGE ( 'NONE', *, *, #4405, .T. ) ;
#16903 = CARTESIAN_POINT ( 'NONE',  ( 17.83931934289999788, 20.00000000000000000, 230.6999999999999886 ) ) ;
#16904 = FILL_AREA_STYLE_COLOUR ( '', #18804 ) ;
#16905 = ORIENTED_EDGE ( 'NONE', *, *, #20250, .F. ) ;
#16906 = CARTESIAN_POINT ( 'NONE',  ( -11.69999999989999928, 19.99999999999999645, -1.399999999999998579 ) ) ;
#16907 = CARTESIAN_POINT ( 'NONE',  ( 0.7459188900473354700, -27.79046661982714639, 3.920206710000012862 ) ) ;
#16908 = ORIENTED_EDGE ( 'NONE', *, *, #19887, .T. ) ;
#16909 = CARTESIAN_POINT ( 'NONE',  ( 5.307277461537168506, -2.951504967840870464, -27.53037294499999277 ) ) ;
#16910 = CARTESIAN_POINT ( 'NONE',  ( -0.7556487780321572423, 4.453147011089724217, -51.25792092402500089 ) ) ;
#16911 = DIRECTION ( 'NONE',  ( 1.000000000000000000, 0.000000000000000000, -0.000000000000000000 ) ) ;
#16912 = B_SPLINE_CURVE_WITH_KNOTS ( 'NONE', 1,
 ( #10136, #12339 ),
 .UNSPECIFIED., .F., .F.,
 ( 2, 2 ),
 ( -3.500000000000000000, 3.500000000000000000 ),
 .UNSPECIFIED. ) ;
#16913 = B_SPLINE_CURVE_WITH_KNOTS ( 'NONE', 4,
 ( #14324, #9735, #16818, #9898, #23924 ),
 .UNSPECIFIED., .F., .F.,
 ( 5, 5 ),
 ( -0.9817477042479999527, 0.9817477042479999527 ),
 .UNSPECIFIED. ) ;
#16914 = CARTESIAN_POINT ( 'NONE',  ( -23.80092421045090489, -14.36517094966148633, 3.899998581000013509 ) ) ;
#16915 = CARTESIAN_POINT ( 'NONE',  ( 23.74337837439999888, -14.46065164910000078, 224.0987030360000176 ) ) ;
#16916 = EDGE_CURVE ( 'NONE', #31008, #15988, #26459, .T. ) ;
#16917 = FACE_OUTER_BOUND ( 'NONE', #9742, .T. ) ;
#16918 = UNCERTAINTY_MEASURE_WITH_UNIT (LENGTH_MEASURE( 1.000000000000000082E-05 ), #29643, 'distance_accuracy_value', 'NONE');
#16919 = DIRECTION ( 'NONE',  ( -0.2815395311429196301, -0.9595496299847262600, 0.000000000000000000 ) ) ;
#16920 = CARTESIAN_POINT ( 'NONE',  ( -17.35614611409699393, -22.00027648907067501, -26.84046950015551047 ) ) ;
#16921 = VERTEX_POINT ( 'NONE', #12128 ) ;
#16922 = DIRECTION ( 'NONE',  ( 1.000000000000000000, -1.224606353819998843E-16, 0.000000000000000000 ) ) ;
#16923 = CARTESIAN_POINT ( 'NONE',  ( 23.45048833493306972, -12.97319122329745156, 224.0048062712651813 ) ) ;
#16924 = CARTESIAN_POINT ( 'NONE',  ( -23.82471740849593544, -15.64077206322649083, 5.208368890000008911 ) ) ;
#16925 = CARTESIAN_POINT ( 'NONE',  ( 1.110223024630000146E-16, 0.000000000000000000, -44.10000000000000142 ) ) ;
#16926 = DIRECTION ( 'NONE',  ( 0.000000000000000000, 0.000000000000000000, 1.000000000000000000 ) ) ;
#16927 = CARTESIAN_POINT ( 'NONE',  ( -8.699999999723049271, -24.33803193940951104, -26.96176843113012112 ) ) ;
#16928 = CARTESIAN_POINT ( 'NONE',  ( -9.999999999979998222, -27.00000000000000000, -31.39999999999999858 ) ) ;
#16929 = CARTESIAN_POINT ( 'NONE',  ( -9.007237961434523044, -15.62744792279970696, -74.56625543040802029 ) ) ;
#16930 = EDGE_CURVE ( 'NONE', #30015, #20876, #187, .T. ) ;
#16931 = DIRECTION ( 'NONE',  ( 3.133604487004501912E-12, 0.3568421334038983650, -0.9341647027306021478 ) ) ;
#16932 = DIRECTION ( 'NONE',  ( 0.000000000000000000, -1.000000000000000000, 2.257145581549999994E-12 ) ) ;
#16933 = VECTOR ( 'NONE', #25083, 1000.000000000000000 ) ;
#16934 = ADVANCED_FACE ( 'NONE', ( #13050 ), #13173, .T. ) ;
#16935 = DIRECTION ( 'NONE',  ( -5.551115123049999208E-18, 0.000000000000000000, -1.000000000000000000 ) ) ;
#16936 = CARTESIAN_POINT ( 'NONE',  ( 7.638687372290042354, 3.773810209576400343, -39.31977939339549266 ) ) ;
#16937 = DIRECTION ( 'NONE',  ( 0.000000000000000000, 0.000000000000000000, -1.000000000000000000 ) ) ;
#16938 = AXIS2_PLACEMENT_3D ( 'NONE', #3363, #3058, #5879 ) ;
#16939 = ORIENTED_EDGE ( 'NONE', *, *, #27674, .F. ) ;
#16940 = CARTESIAN_POINT ( 'NONE',  ( -12.47331730070000155, 21.70000000000000284, -55.90289625529999995 ) ) ;
#16941 = ADVANCED_FACE ( 'NONE', ( #15888 ), #8477, .F. ) ;
#16942 = ORIENTED_EDGE ( 'NONE', *, *, #12325, .T. ) ;
#16943 = CARTESIAN_POINT ( 'NONE',  ( 0.000000000000000000, 0.000000000000000000, 210.0000000000000284 ) ) ;
#16944 = CARTESIAN_POINT ( 'NONE',  ( 3.312932182603874232, 3.356011527877053702, -57.70805965152499795 ) ) ;
#16945 = EDGE_LOOP ( 'NONE', ( #29710, #19602, #4722, #29021 ) ) ;
#16946 = CONTEXT_DEPENDENT_SHAPE_REPRESENTATION ( #13618, #28566 ) ;
#16947 = VERTEX_POINT ( 'NONE', #10694 ) ;
#16949 = EDGE_CURVE ( 'NONE', #4684, #17295, #14227, .T. ) ;
#16948 = LINE ( 'NONE', #2943, #28737 ) ;
#16950 = ORIENTED_EDGE ( 'NONE', *, *, #22021, .F. ) ;
#16951 = ORIENTED_EDGE ( 'NONE', *, *, #23155, .T. ) ;
#16952 = CYLINDRICAL_SURFACE ( 'NONE', #30260, 27.50000000000000000 ) ;
#16953 = DIRECTION ( 'NONE',  ( 1.000000000000000000, 0.000000000000000000, 0.000000000000000000 ) ) ;
#16954 = CARTESIAN_POINT ( 'NONE',  ( 9.572761946760001806, 19.99999999999999645, -43.22291707689799978 ) ) ;
#16955 = CIRCLE ( 'NONE', #4406, 1.999999999999999112 ) ;
#16956 = VECTOR ( 'NONE', #30404, 1000.000000000000000 ) ;
#16957 = CARTESIAN_POINT ( 'NONE',  ( 12.29168530480000143, 0.2506124891389999720, 232.6627648150000027 ) ) ;
#16958 = CARTESIAN_POINT ( 'NONE',  ( 27.76135143639999825, -3.399672735949999729E-15, 87.66141409839998744 ) ) ;
#16959 = CARTESIAN_POINT ( 'NONE',  ( -4.598206294437411579, -3.044638162784917945, -5.889929326000000742 ) ) ;
#16960 = CARTESIAN_POINT ( 'NONE',  ( -20.26572724632349320, -21.15151735177849091, 8.000000000000007105 ) ) ;
#16961 = EDGE_LOOP ( 'NONE', ( #9241, #11383, #18686, #20266, #4909 ) ) ;
#16962 = CARTESIAN_POINT ( 'NONE',  ( -10.00000000070000183, -130.0000000000000000, -41.82335799894999440 ) ) ;
#16963 = ADVANCED_FACE ( 'NONE', ( #17613 ), #28745, .F. ) ;
#16964 = CARTESIAN_POINT ( 'NONE',  ( 3.800013225884302237, -1.579422177728474708, -17.87122516810000405 ) ) ;
#16965 = CARTESIAN_POINT ( 'NONE',  ( -2.020725942109999895, 3.500000000090000007, 230.5235986622430175 ) ) ;
#16966 = CARTESIAN_POINT ( 'NONE',  ( -8.903108651239966420, -22.82508830966961000, 40.00000000000000000 ) ) ;
#16967 = CARTESIAN_POINT ( 'NONE',  ( -6.072586508529999705, -10.48251654620000117, 230.6412452697800006 ) ) ;
#16968 = FACE_BOUND ( 'NONE', #4600, .T. ) ;
#16969 = CARTESIAN_POINT ( 'NONE',  ( -18.41897712746086668, 20.00000741691685846, -0.6632653549999978360 ) ) ;
#16970 = B_SPLINE_SURFACE_WITH_KNOTS ( 'NONE', 5, 5, ( 
 ( #23573, #23877, #14585, #24172, #23719, #7029 ),
 ( #2611, #16618, #4518, #26388, #18827, #7181 ),
 ( #28430, #2007, #4829, #14273, #2319, #31103 ),
 ( #21504, #21815, #19142, #16465, #270, #16769 ),
 ( #14427, #24025, #26079, #21354, #21663, #2467 ),
 ( #9851, #19450, #12059, #7488, #25925, #22858 ) ),
 .UNSPECIFIED., .F., .F., .F.,
 ( 6, 6 ),
 ( 6, 6 ),
 ( 66.71447726240000975, 88.61406016669999985 ),
 ( -3.500000000000000000, 3.500000000000000000 ),
 .UNSPECIFIED. ) ;
#16971 = AXIS2_PLACEMENT_3D ( 'NONE', #21071, #1718, #6429 ) ;
#16972 = CARTESIAN_POINT ( 'NONE',  ( -10.69999999999999929, -120.6167089059000119, -31.26531288160000344 ) ) ;
#16973 = LINE ( 'NONE', #7379, #22302 ) ;
#16974 = AXIS2_PLACEMENT_3D ( 'NONE', #12495, #12815, #24618 ) ;
#16975 = FACE_OUTER_BOUND ( 'NONE', #15786, .T. ) ;
#16976 = CARTESIAN_POINT ( 'NONE',  ( -0.9307262390600369306, -1.887507901406886957, 226.6412452697800006 ) ) ;
#16977 = AXIS2_PLACEMENT_3D ( 'NONE', #12926, #10418, #3167 ) ;
#16978 = CARTESIAN_POINT ( 'NONE',  ( 2.373469614669200922, -26.70001233586149780, 19.99999999999999645 ) ) ;
#16979 = VERTEX_POINT ( 'NONE', #3299 ) ;
#16980 = CARTESIAN_POINT ( 'NONE',  ( 6.487627055914963137, 0.6495842397260740420, -30.23116556699999435 ) ) ;
#16981 = AXIS2_PLACEMENT_3D ( 'NONE', #19262, #81, #7453 ) ;
#16982 = DIRECTION ( 'NONE',  ( 0.000000000000000000, 0.000000000000000000, 1.000000000000000000 ) ) ;
#16983 = ORIENTED_EDGE ( 'NONE', *, *, #24644, .F. ) ;
#16984 = CARTESIAN_POINT ( 'NONE',  ( 24.44014313072642963, -13.24968496497942105, 3.920132093000017193 ) ) ;
#16985 = CARTESIAN_POINT ( 'NONE',  ( 5.643028086411650435, 2.011589847869324377, -45.92627377572500080 ) ) ;
#16986 = ORIENTED_EDGE ( 'NONE', *, *, #30739, .T. ) ;
#16987 = ORIENTED_EDGE ( 'NONE', *, *, #2303, .T. ) ;
#16988 = FILL_AREA_STYLE ('',( #21885 ) ) ;
#16989 = ORIENTED_EDGE ( 'NONE', *, *, #28092, .F. ) ;
#16990 = CARTESIAN_POINT ( 'NONE',  ( -0.3738033647229999645, -27.79799560440000050, 223.9576764909999724 ) ) ;
#16991 = ADVANCED_FACE ( 'NONE', ( #19985 ), #15717, .F. ) ;
#16992 = ORIENTED_EDGE ( 'NONE', *, *, #14258, .F. ) ;
#16993 = LINE ( 'NONE', #26288, #3494 ) ;
#16994 = PRESENTATION_STYLE_ASSIGNMENT (( #1760 ) ) ;
#16995 = CARTESIAN_POINT ( 'NONE',  ( 27.07818553041514065, 6.807801137122736712, 1.000000000000000888 ) ) ;
#16996 = CARTESIAN_POINT ( 'NONE',  ( 0.7245117006341926791, 4.718262249271010234, -35.69999999999999574 ) ) ;
#16997 = AXIS2_PLACEMENT_3D ( 'NONE', #18692, #18854, #25946 ) ;
#16998 = EDGE_CURVE ( 'NONE', #22920, #5024, #10862, .T. ) ;
#16999 = EDGE_CURVE ( 'NONE', #18765, #11066, #20715, .T. ) ;
#17000 = CARTESIAN_POINT ( 'NONE',  ( 8.700000000280658341, -13.90765988010977239, -34.05269868223890484 ) ) ;
#17001 = CARTESIAN_POINT ( 'NONE',  ( -24.39135169139800041, 14.74223402946396000, 5.310643621000004977 ) ) ;
#17002 = CARTESIAN_POINT ( 'NONE',  ( -10.06596365874885812, -25.80632433378972124, 90.00000000000000000 ) ) ;
#17003 = CARTESIAN_POINT ( 'NONE',  ( -8.699999998930268319, -15.05691612485074948, -37.86814428179198444 ) ) ;
#17004 = VERTEX_POINT ( 'NONE', #18228 ) ;
#17005 = CARTESIAN_POINT ( 'NONE',  ( 3.486358836775539594, -2.566383416802844319, -8.972776792899997744 ) ) ;
#17006 = CARTESIAN_POINT ( 'NONE',  ( -4.346598770676703083, -0.007247149673123010061, -28.16856466009999593 ) ) ;
#17007 = CARTESIAN_POINT ( 'NONE',  ( 8.999999999770000869, 20.99999999999999645, -45.10000000000000142 ) ) ;
#17008 = VECTOR ( 'NONE', #22350, 1000.000000000000227 ) ;
#17009 = CARTESIAN_POINT ( 'NONE',  ( -27.50000000000000000, 3.367667473009999970E-15, 136.3944487260000074 ) ) ;
#17010 = CARTESIAN_POINT ( 'NONE',  ( 23.87170004953230773, 14.24726900334573187, 6.095965388000001539 ) ) ;
#17011 = CARTESIAN_POINT ( 'NONE',  ( -17.62526668104891314, 11.76353838341477953, -0.6999999999999784173 ) ) ;
#17012 = CARTESIAN_POINT ( 'NONE',  ( 10.00000000000000000, 22.06507305262541863, -61.91147751336289673 ) ) ;
#17013 = CARTESIAN_POINT ( 'NONE',  ( -0.6370991518874352666, 4.292107257743940529, -10.86772091660000150 ) ) ;
#17014 = FACE_OUTER_BOUND ( 'NONE', #17297, .T. ) ;
#17015 = APPLICATION_CONTEXT ( 'automotive_design' ) ;
#17016 = CARTESIAN_POINT ( 'NONE',  ( 10.99999999979999998, 21.34999999950001026, -70.09999999999999432 ) ) ;
#17017 = FACE_OUTER_BOUND ( 'NONE', #16804, .T. ) ;
#17018 = ORIENTED_EDGE ( 'NONE', *, *, #22849, .F. ) ;
#17019 = VECTOR ( 'NONE', #27217, 1000.000000000000000 ) ;
#17020 = DIRECTION ( 'NONE',  ( 1.000000000000000000, 0.000000000000000000, 0.000000000000000000 ) ) ;
#17021 = DIRECTION ( 'NONE',  ( -4.428977494234582379E-12, -0.8987940462991651502, 0.4383711467890810676 ) ) ;
#17022 = ORIENTED_EDGE ( 'NONE', *, *, #19640, .F. ) ;
#17023 = CARTESIAN_POINT ( 'NONE',  ( 23.67167941903707273, -13.99714051993749919, 6.071909320481077010 ) ) ;
#17024 = CARTESIAN_POINT ( 'NONE',  ( 20.50716141039999840, 18.79636021840000026, 225.9999999149999894 ) ) ;
#17025 = ORIENTED_EDGE ( 'NONE', *, *, #8132, .F. ) ;
#17026 = ORIENTED_EDGE ( 'NONE', *, *, #28444, .F. ) ;
#17027 = ORIENTED_EDGE ( 'NONE', *, *, #28054, .T. ) ;
#17028 = ORIENTED_EDGE ( 'NONE', *, *, #27509, .F. ) ;
#17029 = DIRECTION ( 'NONE',  ( 0.000000000000000000, 0.000000000000000000, 1.000000000000000000 ) ) ;
#17030 = AXIS2_PLACEMENT_3D ( 'NONE', #30331, #20569, #10824 ) ;
#17031 = CARTESIAN_POINT ( 'NONE',  ( -26.05511412830000140, 14.93229958979999950, 229.0000000000000000 ) ) ;
#17032 = CARTESIAN_POINT ( 'NONE',  ( -5.945069363104310334, -15.39359683734633677, -109.1271631200178689 ) ) ;
#17033 = VERTEX_POINT ( 'NONE', #8318 ) ;
#17034 = CARTESIAN_POINT ( 'NONE',  ( -25.46368746804859740, 12.80129684245613575, 5.104216618000034345 ) ) ;
#17035 = B_SPLINE_CURVE_WITH_KNOTS ( 'NONE', 3,
 ( #23864, #29458, #14576, #24593, #28724, #31093 ),
 .UNSPECIFIED., .F., .F.,
 ( 4, 2, 4 ),
 ( 0.000000000000000000, 0.5000000000000000000, 1.000000000000000000 ),
 .UNSPECIFIED. ) ;
#17036 = DIRECTION ( 'NONE',  ( 0.000000000000000000, 0.000000000000000000, 1.000000000000000000 ) ) ;
#17037 = ADVANCED_FACE ( 'NONE', ( #17913 ), #27522, .T. ) ;
#17038 = CARTESIAN_POINT ( 'NONE',  ( -17.39358994610300257, -31.99978466862134141, -27.07701006545490330 ) ) ;
#17039 = CARTESIAN_POINT ( 'NONE',  ( 7.418657832813924990, -7.750849174212353532, -37.03663326122587307 ) ) ;
#17040 = VERTEX_POINT ( 'NONE', #15562 ) ;
#17041 = LINE ( 'NONE', #2572, #9458 ) ;
#17042 = CARTESIAN_POINT ( 'NONE',  ( 3.791027721911684800, -3.577548591872723449, -17.03565261000001385 ) ) ;
#17043 = DIRECTION ( 'NONE',  ( 0.2815395311429195746, 0.9595496299847261490, 0.000000000000000000 ) ) ;
#17044 = ADVANCED_BREP_SHAPE_REPRESENTATION ( '', ( #438, #17722 ), #9278 ) ;
#17045 = FACE_OUTER_BOUND ( 'NONE', #23272, .T. ) ;
#17046 = CARTESIAN_POINT ( 'NONE',  ( -12.30800288698999978, -29.39779533043000015, -32.78913491261000246 ) ) ;
#17047 = CARTESIAN_POINT ( 'NONE',  ( 24.10374060750000069, 15.23914466740000151, 222.0000000000000000 ) ) ;
#17048 = CARTESIAN_POINT ( 'NONE',  ( 26.84464183080000055, -3.287411895189999871E-15, 92.56249624490000372 ) ) ;
#17049 = AXIS2_PLACEMENT_3D ( 'NONE', #11889, #4507, #19128 ) ;
#17050 = B_SPLINE_CURVE_WITH_KNOTS ( 'NONE', 3,
 ( #7034, #31108, #7187, #14120, #4670, #280, #21200, #26689, #30798, #26541, #14739, #26233 ),
 .UNSPECIFIED., .F., .F.,
 ( 4, 2, 2, 2, 2, 4 ),
 ( 0.000000000000000000, 0.2500000000000126565, 0.5000000000000253131, 0.6250000000000296430, 0.7500000000000339728, 1.000000000000000000 ),
 .UNSPECIFIED. ) ;
#17051 = CARTESIAN_POINT ( 'NONE',  ( 8.000000000278095769, -14.92844969908619035, -33.25053330389217621 ) ) ;
#17052 = CARTESIAN_POINT ( 'NONE',  ( 8.699999999555858565, -13.61360970152257721, -34.64062719131236179 ) ) ;
#17053 = CARTESIAN_POINT ( 'NONE',  ( 24.19803665890000133, 13.43835505600000069, 229.9751240860000223 ) ) ;
#17054 = CARTESIAN_POINT ( 'NONE',  ( -7.999999999719110022, -29.98791861939423598, -27.92402217208466197 ) ) ;
#17055 = ORIENTED_EDGE ( 'NONE', *, *, #7133, .F. ) ;
#17056 = CARTESIAN_POINT ( 'NONE',  ( -12.39529267487105102, -23.42185988122897555, -24.69233746907211469 ) ) ;
#17057 = CARTESIAN_POINT ( 'NONE',  ( -27.52676963214367944, -0.5008603480904468830, 0.2686740700000300741 ) ) ;
#17058 = CARTESIAN_POINT ( 'NONE',  ( 9.999999999933628203, -25.95491900963585152, -13.51082902187790857 ) ) ;
#17059 = ORIENTED_EDGE ( 'NONE', *, *, #7016, .F. ) ;
#17060 = EDGE_CURVE ( 'NONE', #6349, #13182, #3603, .T. ) ;
#17061 = CARTESIAN_POINT ( 'NONE',  ( 17.16657240410000185, -9.000000001100003644, -0.6999999999999992895 ) ) ;
#17062 = SURFACE_STYLE_USAGE ( .BOTH. , #7008 ) ;
#17063 = ORIENTED_EDGE ( 'NONE', *, *, #26599, .F. ) ;
#17064 = CARTESIAN_POINT ( 'NONE',  ( -11.43935997342166822, 19.99999999999998934, -1.425491584528367772 ) ) ;
#17065 = CARTESIAN_POINT ( 'NONE',  ( -3.200877993934835075, 3.183711413074212349, -68.94322600112499799 ) ) ;
#17066 = ORIENTED_EDGE ( 'NONE', *, *, #25344, .F. ) ;
#17067 = CARTESIAN_POINT ( 'NONE',  ( -3.253989917302557267, -2.899813084402114161, -25.34101932449999595 ) ) ;
#17068 = DIRECTION ( 'NONE',  ( 0.9316362575375356503, 0.3633921898465274913, 0.000000000000000000 ) ) ;
#17069 = VECTOR ( 'NONE', #18257, 1000.000000000000000 ) ;
#17070 = B_SPLINE_SURFACE_WITH_KNOTS ( 'NONE', 5, 1, ( 
 ( #9159, #16866 ),
 ( #9478, #21603 ),
 ( #6966, #14520 ),
 ( #18921, #18762 ),
 ( #19081, #17024 ),
 ( #23968, #28363 ) ),
 .UNSPECIFIED., .F., .F., .F.,
 ( 6, 6 ),
 ( 2, 2 ),
 ( 0.000000000000000000, 7.118285296629999870 ),
 ( -0.7000000117410000167, 0.0003775348956340000232 ),
 .UNSPECIFIED. ) ;
#17071 = CARTESIAN_POINT ( 'NONE',  ( -0.9606962270921406422, -4.447130805931738706, -55.93033560642499680 ) ) ;
#17072 = CARTESIAN_POINT ( 'NONE',  ( 8.000000000252409649, -24.26136093482662304, -29.62468611105709471 ) ) ;
#17073 = CARTESIAN_POINT ( 'NONE',  ( -10.00000000000000000, 21.72305290929948640, -60.97178489257708378 ) ) ;
#17074 = CARTESIAN_POINT ( 'NONE',  ( -15.81846178510917156, 11.44785871239032105, -1.400000000000001910 ) ) ;
#17075 = LINE ( 'NONE', #21657, #15828 ) ;
#17076 = CARTESIAN_POINT ( 'NONE',  ( -17.31586207617448636, -22.00035168746386560, -30.24399382304843797 ) ) ;
#17077 = EDGE_CURVE ( 'NONE', #2594, #27396, #27221, .T. ) ;
#17078 = EDGE_LOOP ( 'NONE', ( #25392, #18449, #19235, #16794 ) ) ;
#17079 = CARTESIAN_POINT ( 'NONE',  ( -15.73360964030186970, 11.02001161816959396, -1.000005633855494125E-09 ) ) ;
#17080 = CARTESIAN_POINT ( 'NONE',  ( 23.64633388422165083, -12.61377020549707417, 224.3610176357263128 ) ) ;
#17081 = CARTESIAN_POINT ( 'NONE',  ( 0.1347871022389999784, -12.22452263659999971, 232.6627643349999914 ) ) ;
#17082 = CARTESIAN_POINT ( 'NONE',  ( 3.052989692426276491, -2.544715063274864519, -96.33992724129673491 ) ) ;
#17083 = DIRECTION ( 'NONE',  ( 1.000000000000000000, 0.000000000000000000, 0.000000000000000000 ) ) ;
#17084 = CARTESIAN_POINT ( 'NONE',  ( -5.987315253674642790, -30.20684655539371732, -79.87272256617823984 ) ) ;
#17085 = CARTESIAN_POINT ( 'NONE',  ( 24.47668464858733373, -13.18089138023650975, 224.2673115778495685 ) ) ;
#17086 = CARTESIAN_POINT ( 'NONE',  ( -25.77914833258148164, -15.40383343755785361, 1.000000000000000888 ) ) ;
#17087 = LINE ( 'NONE', #7641, #24319 ) ;
#17088 = CARTESIAN_POINT ( 'NONE',  ( -25.35851007062240114, 13.00862288638852959, 4.319165764000016061 ) ) ;
#17089 = DIRECTION ( 'NONE',  ( 0.000000000000000000, -0.9396926207858125046, -0.3420201433259318358 ) ) ;
#17090 = EDGE_CURVE ( 'NONE', #2594, #21789, #23987, .T. ) ;
#17091 = B_SPLINE_CURVE_WITH_KNOTS ( 'NONE', 3,
 ( #13353, #1090, #15403, #13509, #20277, #22800 ),
 .UNSPECIFIED., .F., .F.,
 ( 4, 2, 4 ),
 ( 0.000000000000000000, 0.5000000000000000000, 1.000000000000000000 ),
 .UNSPECIFIED. ) ;
#17092 = CARTESIAN_POINT ( 'NONE',  ( -24.24391315718250084, -12.98049462764927853, 5.674968348892686976 ) ) ;
#17093 = CARTESIAN_POINT ( 'NONE',  ( 13.99999999979999821, 20.99999999999999645, -58.51619795559999915 ) ) ;
#17094 = FACE_OUTER_BOUND ( 'NONE', #20130, .T. ) ;
#17095 = VERTEX_POINT ( 'NONE', #3773 ) ;
#17096 = EDGE_CURVE ( 'NONE', #21014, #5533, #17218, .T. ) ;
#17097 = PLANE ( 'NONE',  #12254 ) ;
#17098 = ORIENTED_EDGE ( 'NONE', *, *, #3028, .F. ) ;
#17099 = CARTESIAN_POINT ( 'NONE',  ( 24.60666973300000038, -12.93650480179999995, 225.0000014190000002 ) ) ;
#17100 = CARTESIAN_POINT ( 'NONE',  ( -4.385510522249749243, 2.177216032696348780, -57.54877225282500319 ) ) ;
#17101 = ORIENTED_EDGE ( 'NONE', *, *, #7485, .F. ) ;
#17102 = VERTEX_POINT ( 'NONE', #31106 ) ;
#17103 = DIRECTION ( 'NONE',  ( 0.000000000000000000, 0.000000000000000000, 1.000000000000000000 ) ) ;
#17104 = VERTEX_POINT ( 'NONE', #27995 ) ;
#17105 = VERTEX_POINT ( 'NONE', #16928 ) ;
#17106 = EDGE_CURVE ( 'NONE', #565, #10669, #649, .T. ) ;
#17107 = CARTESIAN_POINT ( 'NONE',  ( 8.000000000251251464, -25.56183060493181358, -31.06205794070631043 ) ) ;
#17108 = CARTESIAN_POINT ( 'NONE',  ( -4.861312627776433359, -11.03139726553092892, -35.43660304873223765 ) ) ;
#17109 = EDGE_CURVE ( 'NONE', #26791, #17104, #274, .T. ) ;
#17110 = CARTESIAN_POINT ( 'NONE',  ( -11.83960380747999963, -33.00000000000000000, -28.40000000000771863 ) ) ;
#17111 = CYLINDRICAL_SURFACE ( 'NONE', #10432, 3.000000000000002220 ) ;
#17112 = CARTESIAN_POINT ( 'NONE',  ( 3.904508939291361003, -1.994718106397497914, -11.91474735220000092 ) ) ;
#17113 = DIRECTION ( 'NONE',  ( 1.000000000000000000, 0.000000000000000000, 0.000000000000000000 ) ) ;
#17114 = EDGE_LOOP ( 'NONE', ( #11859, #9470, #16213, #1401 ) ) ;
#17115 = CARTESIAN_POINT ( 'NONE',  ( 2.828562571734781095, -3.451486673425649077, -44.10000000002499831 ) ) ;
#17116 = LINE ( 'NONE', #2647, #26359 ) ;
#17117 = EDGE_CURVE ( 'NONE', #145, #9481, #7032, .T. ) ;
#17118 = CARTESIAN_POINT ( 'NONE',  ( -0.8316310374238428116, 4.718996048841939128, -20.77333244400000822 ) ) ;
#17119 = CARTESIAN_POINT ( 'NONE',  ( -1.238178402492337682, 3.499999999999999112, 230.7147300523246543 ) ) ;
#17120 = DIRECTION ( 'NONE',  ( -0.000000000000000000, 1.000000000000000000, 0.000000000000000000 ) ) ;
#17121 = CARTESIAN_POINT ( 'NONE',  ( -1.630907768819999992, -5.558498092260000689, 226.6412452697800006 ) ) ;
#17122 = DIRECTION ( 'NONE',  ( 0.3633921898465273803, -0.9316362575375355393, 1.734723475976806306E-15 ) ) ;
#17123 = CARTESIAN_POINT ( 'NONE',  ( -18.03078366343508421, 19.99999999996890665, -0.6999999999999784173 ) ) ;
#17124 = CARTESIAN_POINT ( 'NONE',  ( -7.999999999945442752, -112.0649859495781300, 5.802913492026387843 ) ) ;
#17125 = CARTESIAN_POINT ( 'NONE',  ( 1.100000000000000089, -26.77741585740000119, 225.0000000000000000 ) ) ;
#17126 = PLANE ( 'NONE',  #19837 ) ;
#17127 = EDGE_CURVE ( 'NONE', #9871, #4371, #16621, .T. ) ;
#17128 = CARTESIAN_POINT ( 'NONE',  ( -24.83650131330000121, 13.77747940689999950, 229.1414214410000056 ) ) ;
#17129 = DIRECTION ( 'NONE',  ( 1.000000000000000000, 0.000000000000000000, 0.000000000000000000 ) ) ;
#17130 = ORIENTED_EDGE ( 'NONE', *, *, #14934, .T. ) ;
#17131 = CARTESIAN_POINT ( 'NONE',  ( -3.231711866632715147, -5.662799918003592836, -30.67642233980000199 ) ) ;
#17132 = ORIENTED_EDGE ( 'NONE', *, *, #1351, .T. ) ;
#17133 = CARTESIAN_POINT ( 'NONE',  ( 24.98823331316959440, -13.70626928515100573, 3.904029301000005781 ) ) ;
#17134 = CARTESIAN_POINT ( 'NONE',  ( 5.925978784015399903, -0.8792241758803844842, -46.61818262062499940 ) ) ;
#17135 = VERTEX_POINT ( 'NONE', #16773 ) ;
#17136 = ADVANCED_FACE ( 'NONE', ( #6440 ), #30953, .F. ) ;
#17137 = EDGE_LOOP ( 'NONE', ( #17492, #4876, #8237, #26238 ) ) ;
#17138 = ORIENTED_EDGE ( 'NONE', *, *, #21269, .T. ) ;
#17139 = FACE_OUTER_BOUND ( 'NONE', #27877, .T. ) ;
#17140 = ORIENTED_EDGE ( 'NONE', *, *, #981, .T. ) ;
#17141 = CARTESIAN_POINT ( 'NONE',  ( 23.50666810109999716, -14.84174128299999929, 225.0000014190000002 ) ) ;
#17142 =( LENGTH_UNIT ( ) NAMED_UNIT ( * ) SI_UNIT ( .MILLI., .METRE. ) );
#17143 = DIRECTION ( 'NONE',  ( 4.428977494234582379E-12, 0.8987940462991651502, -0.4383711467890810676 ) ) ;
#17144 = CARTESIAN_POINT ( 'NONE',  ( 0.3318591986118693549, 4.627280206481456659, -35.69999999999999574 ) ) ;
#17145 = CARTESIAN_POINT ( 'NONE',  ( -12.30733375691920628, -29.69486568737967502, -24.18213133546005977 ) ) ;
#17146 = EDGE_CURVE ( 'NONE', #902, #26900, #22246, .T. ) ;
#17147 = CARTESIAN_POINT ( 'NONE',  ( -2.017871889752692383, -3.161030873707806332, -0.6999999999999992895 ) ) ;
#17148 = CARTESIAN_POINT ( 'NONE',  ( 0.000000000000000000, 0.000000000000000000, 140.0000000000000000 ) ) ;
#17149 = CARTESIAN_POINT ( 'NONE',  ( -23.56894429787650935, -14.74331334052646980, 224.5038504355401017 ) ) ;
#17150 = EDGE_LOOP ( 'NONE', ( #26314, #13064, #23587, #16497 ) ) ;
#17151 = CARTESIAN_POINT ( 'NONE',  ( 0.4590887144193210312, -5.884162454197269909, -10.39338421180000438 ) ) ;
#17152 = CARTESIAN_POINT ( 'NONE',  ( -4.273414424137721213, 4.913340199448848367, -27.98728588870000422 ) ) ;
#17153 = CARTESIAN_POINT ( 'NONE',  ( -2.858922298043036214, -2.052062286655957024, 0.000000000000000000 ) ) ;
#17154 = DIRECTION ( 'NONE',  ( -1.000000000000000000, 5.687697999151106851E-16, -6.771501495036750356E-12 ) ) ;
#17155 = DIRECTION ( 'NONE',  ( -1.000000000000000000, 0.000000000000000000, 0.000000000000000000 ) ) ;
#17156 = CARTESIAN_POINT ( 'NONE',  ( -17.52370713000112090, 11.86883708413922811, -0.6999999999999784173 ) ) ;
#17157 = CARTESIAN_POINT ( 'NONE',  ( 3.283040606112535897, -20.07229108452098032, -27.68925868202152074 ) ) ;
#17158 = CARTESIAN_POINT ( 'NONE',  ( 0.5300456733980246637, -4.293941145674104121, -18.37054674910000429 ) ) ;
#17159 = B_SPLINE_SURFACE_WITH_KNOTS ( 'NONE', 5, 1, ( 
 ( #2988, #176 ),
 ( #14495, #7849 ),
 ( #7698, #26447 ),
 ( #5185, #26910 ),
 ( #19831, #21724 ),
 ( #16995, #26600 ),
 ( #5347, #14952 ),
 ( #12578, #5039 ),
 ( #22342, #24090 ) ),
 .UNSPECIFIED., .F., .F., .F.,
 ( 6, 3, 6 ),
 ( 2, 2 ),
 ( 67.22752578339999729, 77.81866039000000512, 88.40979499649999696 ),
 ( -3.500000000000000000, 3.500000000000000000 ),
 .UNSPECIFIED. ) ;
#17160 = AXIS2_PLACEMENT_3D ( 'NONE', #22011, #12866, #22313 ) ;
#17161 = B_SPLINE_CURVE_WITH_KNOTS ( 'NONE', 3,
 ( #6953, #16547, #26155, #14197, #14362, #23960, #42, #7268, #16857, #2547, #14971, #19540, #12441, #19690, #26614, #17163, #12752, #12134 ),
 .UNSPECIFIED., .F., .F.,
 ( 4, 2, 2, 2, 2, 2, 2, 2, 4 ),
 ( 0.000000000000000000, 0.1250000000000000000, 0.2500000000000000000, 0.3750000000000000000, 0.5000000000000000000, 0.6250000000000000000, 0.7500000000000000000, 0.8750000000000000000, 1.000000000000000000 ),
 .UNSPECIFIED. ) ;
#17163 = CARTESIAN_POINT ( 'NONE',  ( 16.08831934135733022, 11.26096619629935702, -1.400000000000001910 ) ) ;
#17162 = B_SPLINE_CURVE_WITH_KNOTS ( 'NONE', 3,
 ( #1932, #28197, #18283, #25853, #21276, #4292, #13887, #15931, #11525, #25539 ),
 .UNSPECIFIED., .F., .F.,
 ( 4, 2, 2, 2, 4 ),
 ( 0.000000000000000000, 0.2500000000000000000, 0.5000000000000000000, 0.7500000000000000000, 1.000000000000000000 ),
 .UNSPECIFIED. ) ;
#17164 = CARTESIAN_POINT ( 'NONE',  ( 7.105427357599999217E-15, 8.881784197000000993E-16, 224.6412452697800290 ) ) ;
#17165 = DIRECTION ( 'NONE',  ( -5.962915006522622422E-16, -0.4383711467890810676, -0.8987940462991651502 ) ) ;
#17166 = EDGE_CURVE ( 'NONE', #23803, #15341, #11207, .T. ) ;
#17167 = ORIENTED_EDGE ( 'NONE', *, *, #21334, .T. ) ;
#17168 = AXIS2_PLACEMENT_3D ( 'NONE', #14842, #26946, #12315 ) ;
#17169 = EDGE_CURVE ( 'NONE', #17596, #61, #7491, .T. ) ;
#17170 = CARTESIAN_POINT ( 'NONE',  ( 8.000000000858760174, -25.41682687355206482, -25.82167197184731577 ) ) ;
#17171 = CARTESIAN_POINT ( 'NONE',  ( 13.99999999979999821, 20.99999999999999645, -67.09999999999999432 ) ) ;
#17172 = ORIENTED_EDGE ( 'NONE', *, *, #16426, .F. ) ;
#17173 = LINE ( 'NONE', #3158, #7303 ) ;
#17174 = CARTESIAN_POINT ( 'NONE',  ( -11.69999999989999928, 19.99999999999999645, -0.6999999999999992895 ) ) ;
#17175 = ORIENTED_EDGE ( 'NONE', *, *, #1535, .F. ) ;
#17176 = FACE_OUTER_BOUND ( 'NONE', #27816, .T. ) ;
#17177 = ORIENTED_EDGE ( 'NONE', *, *, #7194, .F. ) ;
#17178 = VERTEX_POINT ( 'NONE', #12062 ) ;
#17179 = VERTEX_POINT ( 'NONE', #8797 ) ;
#17180 = CARTESIAN_POINT ( 'NONE',  ( -17.49999999970000175, -28.51480899498708510, -31.01896946163343216 ) ) ;
#17181 = CARTESIAN_POINT ( 'NONE',  ( -26.80000000000000071, 9.769962616700000205E-15, 36.78285841159999592 ) ) ;
#17182 = CARTESIAN_POINT ( 'NONE',  ( 17.04261818930491401, 9.897562529765991712, -0.6999999999999783062 ) ) ;
#17183 = ORIENTED_EDGE ( 'NONE', *, *, #27917, .T. ) ;
#17184 = CARTESIAN_POINT ( 'NONE',  ( 0.000000000000000000, 0.000000000000000000, 40.00000000000000000 ) ) ;
#17185 = AXIS2_PLACEMENT_3D ( 'NONE', #5160, #22015, #471 ) ;
#17186 = FACE_OUTER_BOUND ( 'NONE', #23305, .T. ) ;
#17187 = DIRECTION ( 'NONE',  ( 1.000000000000000000, -0.000000000000000000, 0.000000000000000000 ) ) ;
#17188 = CARTESIAN_POINT ( 'NONE',  ( 10.69999999993478568, -25.95326775694153199, -13.50807451238996570 ) ) ;
#17189 = ORIENTED_EDGE ( 'NONE', *, *, #13852, .F. ) ;
#17190 = CARTESIAN_POINT ( 'NONE',  ( -12.41421356240000051, 25.87105682045942245, -59.46203493729375822 ) ) ;
#17191 = CARTESIAN_POINT ( 'NONE',  ( 3.800013225884302237, -1.579422177728474708, -17.87122516810000405 ) ) ;
#17192 = CARTESIAN_POINT ( 'NONE',  ( 0.6731456008920000400, -3.434453875705480108, -72.25672407562892374 ) ) ;
#17193 = CARTESIAN_POINT ( 'NONE',  ( 10.82908725742652223, -27.76276047461856678, 186.7828584120000244 ) ) ;
#17194 = CARTESIAN_POINT ( 'NONE',  ( 7.453090060300407771, -2.907137518772283435, 210.0000000000000284 ) ) ;
#17195 = CARTESIAN_POINT ( 'NONE',  ( 0.5057536231481193356, -27.79562098839016571, 3.899998581000013509 ) ) ;
#17196 = CARTESIAN_POINT ( 'NONE',  ( 22.74641636092161434, -14.17229404674536042, 5.633487048338723824 ) ) ;
#17197 = CYLINDRICAL_SURFACE ( 'NONE', #15480, 3.000000000000002220 ) ;
#17198 = CARTESIAN_POINT ( 'NONE',  ( -10.00000000001209344, -15.94902145808038618, -35.53273252466679111 ) ) ;
#17199 = CARTESIAN_POINT ( 'NONE',  ( 18.50497803200000035, 20.74625852820000205, 229.1414212620000228 ) ) ;
#17200 = CARTESIAN_POINT ( 'NONE',  ( 1.854620136230000105, 18.18682247289999765, 230.6999999999999886 ) ) ;
#17201 = ADVANCED_FACE ( 'NONE', ( #9547 ), #16043, .T. ) ;
#17202 = ORIENTED_EDGE ( 'NONE', *, *, #1809, .T. ) ;
#17203 = CARTESIAN_POINT ( 'NONE',  ( -1.192105394233154314, -5.728767129463715690, -52.12706695232498788 ) ) ;
#17204 = AXIS2_PLACEMENT_3D ( 'NONE', #12626, #26647, #17353 ) ;
#17205 = CARTESIAN_POINT ( 'NONE',  ( 6.000000000000000000, -16.80434454291883029, -74.99461076894029077 ) ) ;
#17206 = ADVANCED_FACE ( 'NONE', ( #26537 ), #2322, .T. ) ;
#17207 = CARTESIAN_POINT ( 'NONE',  ( -1.756770791141829546, 0.9559060557399279290, 231.1412452697749984 ) ) ;
#17208 = CARTESIAN_POINT ( 'NONE',  ( -4.117519161151379059, -0.1404918132599033975, -68.10000000002499121 ) ) ;
#17209 = EDGE_CURVE ( 'NONE', #7653, #24157, #21666, .T. ) ;
#17210 = ORIENTED_EDGE ( 'NONE', *, *, #15941, .F. ) ;
#17211 = CARTESIAN_POINT ( 'NONE',  ( 1.041264040880410136, -0.4587700011719486604, -98.09067668424567898 ) ) ;
#17212 = EDGE_LOOP ( 'NONE', ( #24955, #15291, #14600, #29011 ) ) ;
#17213 = CYLINDRICAL_SURFACE ( 'NONE', #7439, 3.000000000000003997 ) ;
#17214 = CARTESIAN_POINT ( 'NONE',  ( -9.500000000000000000, 21.70000000000000284, -60.10000000019999788 ) ) ;
#17215 = ORIENTED_EDGE ( 'NONE', *, *, #10597, .T. ) ;
#17216 = CARTESIAN_POINT ( 'NONE',  ( -5.367600138795724618, 3.713494282866228069, -25.46779765530001072 ) ) ;
#17217 = FACE_OUTER_BOUND ( 'NONE', #5837, .T. ) ;
#17218 = B_SPLINE_CURVE_WITH_KNOTS ( 'NONE', 5,
 ( #30043, #22811, #1263, #27677, #27837, #13364, #10550, #22974, #6123, #1419, #11013, #30201, #28893, #18398, #4085 ),
 .UNSPECIFIED., .F., .F.,
 ( 6, 3, 3, 3, 6 ),
 ( 0.000000000000000000, 6.476076814690000738, 12.95215362940000325, 19.42823044409999866, 25.90430725880000651 ),
 .UNSPECIFIED. ) ;
#17219 = CARTESIAN_POINT ( 'NONE',  ( 2.637655088286928962, -3.673227524439524050, -61.52197827312500067 ) ) ;
#17220 = DIRECTION ( 'NONE',  ( -1.000000000000000000, 0.000000000000000000, 0.000000000000000000 ) ) ;
#17221 = AXIS2_PLACEMENT_3D ( 'NONE', #23335, #20964, #26002 ) ;
#17222 = FILL_AREA_STYLE ('',( #3519 ) ) ;
#17223 = B_SPLINE_SURFACE_WITH_KNOTS ( 'NONE', 5, 1, ( 
 ( #13685, #8799 ),
 ( #23288, #13366 ),
 ( #16196, #18709 ),
 ( #28466, #18557 ),
 ( #11168, #6597 ),
 ( #11015, #23454 ),
 ( #18401, #3933 ),
 ( #27839, #8635 ),
 ( #11329, #28308 ),
 ( #20763, #1732 ),
 ( #6903, #25493 ),
 ( #4396, #6291 ),
 ( #30370, #15890 ),
 ( #1884, #20926 ),
 ( #11483, #8958 ) ),
 .UNSPECIFIED., .F., .F., .F.,
 ( 6, 3, 3, 3, 6 ),
 ( 2, 2 ),
 ( 0.000000000000000000, 0.5239017170190000128, 1.047803434039999981, 1.571705151059999972, 1.746339056730000117 ),
 ( -0.7000000000009999335, 2.556331278550000249E-06 ),
 .UNSPECIFIED. ) ;
#17224 = PLANE ( 'NONE',  #19776 ) ;
#17225 = UNCERTAINTY_MEASURE_WITH_UNIT (LENGTH_MEASURE( 1.000000000000000082E-05 ), #15586, 'distance_accuracy_value', 'NONE');
#17226 = CARTESIAN_POINT ( 'NONE',  ( -7.999999999683915952, -16.84112630284391443, -33.19732204833458411 ) ) ;
#17227 = DIRECTION ( 'NONE',  ( 1.000000000000000000, 0.000000000000000000, 0.000000000000000000 ) ) ;
#17228 = ORIENTED_EDGE ( 'NONE', *, *, #3291, .F. ) ;
#17229 = CARTESIAN_POINT ( 'NONE',  ( 14.54659216920905962, -31.99974211811322533, -26.04155240325682641 ) ) ;
#17230 = DIRECTION ( 'NONE',  ( -0.8923935798119907448, -1.018860921557044162E-12, -0.4512579070889951582 ) ) ;
#17231 = EDGE_CURVE ( 'NONE', #6392, #8755, #16836, .T. ) ;
#17232 = CARTESIAN_POINT ( 'NONE',  ( -8.981701821569998856, 8.059682504060001307, 231.9999989789999972 ) ) ;
#17233 = CARTESIAN_POINT ( 'NONE',  ( 17.18658402238548533, 9.900182044515950963, -0.6999999999999784173 ) ) ;
#17234 = LINE ( 'NONE', #5742, #23720 ) ;
#17235 = CARTESIAN_POINT ( 'NONE',  ( -5.414213562369999622, -31.28896728272270877, -80.26658230080884948 ) ) ;
#17236 = CARTESIAN_POINT ( 'NONE',  ( -11.69999999989999928, -2.500000000000002220, -2.399999999999999467 ) ) ;
#17237 = CARTESIAN_POINT ( 'NONE',  ( -28.49528339128749366, -0.5184828350247816520, 0.7595836940000044724 ) ) ;
#17238 = CARTESIAN_POINT ( 'NONE',  ( 23.81866167241657806, 14.33570040768432996, 6.099998581000020792 ) ) ;
#17239 = CARTESIAN_POINT ( 'NONE',  ( 24.37165445055180157, -14.77472140295711434, 4.999998581000003384 ) ) ;
#17240 = CARTESIAN_POINT ( 'NONE',  ( 17.14656078599760392, 12.09981795542235439, -1.000005633855494125E-09 ) ) ;
#17241 = AXIS2_PLACEMENT_3D ( 'NONE', #12745, #20145, #22975 ) ;
#17242 = FACE_OUTER_BOUND ( 'NONE', #27126, .T. ) ;
#17243 = CYLINDRICAL_SURFACE ( 'NONE', #7778, 1.099999999999999867 ) ;
#17244 = VECTOR ( 'NONE', #11675, 1000.000000000000114 ) ;
#17245 = VERTEX_POINT ( 'NONE', #26685 ) ;
#17246 = CARTESIAN_POINT ( 'NONE',  ( 20.30396079662882158, 20.00000000004802203, 2.600000000000019185 ) ) ;
#17247 = CARTESIAN_POINT ( 'NONE',  ( 24.33395417675687611, -14.83647238286172509, 224.1112557440231114 ) ) ;
#17248 = CARTESIAN_POINT ( 'NONE',  ( -0.05440858064702409902, 4.649678238646714590, -58.06818518972500698 ) ) ;
#17249 = ORIENTED_EDGE ( 'NONE', *, *, #28551, .F. ) ;
#17250 = B_SPLINE_CURVE_WITH_KNOTS ( 'NONE', 5,
 ( #15799, #15957, #25563, #16111, #18776, #18934, #14070, #16421, #21460 ),
 .UNSPECIFIED., .F., .F.,
 ( 6, 3, 6 ),
 ( 0.000000000000000000, 3.075806851740000347, 4.017655677589999641 ),
 .UNSPECIFIED. ) ;
#17251 = EDGE_LOOP ( 'NONE', ( #13350, #4069, #14061, #16297 ) ) ;
#17252 = LINE ( 'NONE', #5306, #7134 ) ;
#17253 = ORIENTED_EDGE ( 'NONE', *, *, #29773, .F. ) ;
#17254 = EDGE_CURVE ( 'NONE', #29606, #18476, #9701, .T. ) ;
#17255 = AXIS2_PLACEMENT_3D ( 'NONE', #10024, #16784, #11913 ) ;
#17256 = DIRECTION ( 'NONE',  ( 0.000000000000000000, -0.9396926207858125046, -0.3420201433259318358 ) ) ;
#17257 = VECTOR ( 'NONE', #18714, 1000.000000000000000 ) ;
#17258 = CARTESIAN_POINT ( 'NONE',  ( -24.70074544867652122, 14.21822122508601716, 3.997190861000005313 ) ) ;
#17259 = DIRECTION ( 'NONE',  ( -1.000000000000000000, -2.587524353642439916E-24, -2.257144471329210308E-12 ) ) ;
#17260 = ADVANCED_FACE ( 'NONE', ( #3228 ), #20075, .F. ) ;
#17261 = B_SPLINE_CURVE_WITH_KNOTS ( 'NONE', 3,
 ( #25367, #6154, #17497, #8192, #6000, #10426, #27102, #23004, #20018, #10888, #17796, #15599, #24743, #20478, #3175, #27406, #25201, #3805, #15448, #25050, #1131, #1453, #20324, #10722 ),
 .UNSPECIFIED., .F., .F.,
 ( 4, 2, 2, 2, 2, 2, 2, 2, 2, 2, 2, 4 ),
 ( 0.000000000000000000, 0.001576261392767915439, 0.002364392089151865026, 0.003152522785535814397, 0.004728784178303712706, 0.005516914874687660342, 0.006305045571071608845, 0.007881306963839505852, 0.009457568356607402860, 0.01024569905299135136, 0.01103382974937529813, 0.01261009114214319514 ),
 .UNSPECIFIED. ) ;
#17262 = AXIS2_PLACEMENT_3D ( 'NONE', #29977, #12992, #24650 ) ;
#17263 = CARTESIAN_POINT ( 'NONE',  ( 16.99504414847917744, 12.09604337533561669, -1.400000000000001910 ) ) ;
#17264 = CARTESIAN_POINT ( 'NONE',  ( 8.700000000275174727, -18.43913150047637828, -35.13595876467604739 ) ) ;
#17265 = CARTESIAN_POINT ( 'NONE',  ( 4.262818619062177738, -0.7545854518158033875, -8.271482634700015879 ) ) ;
#17266 = PLANE ( 'NONE',  #20543 ) ;
#17267 = ORIENTED_EDGE ( 'NONE', *, *, #2366, .F. ) ;
#17268 = CARTESIAN_POINT ( 'NONE',  ( 0.5885947091413640253, -3.963556596990289727, -44.10000000002499831 ) ) ;
#17269 = CARTESIAN_POINT ( 'NONE',  ( 27.50000000000000000, -3.367667472999999580E-15, 93.60555127639999284 ) ) ;
#17270 = EDGE_CURVE ( 'NONE', #17343, #11027, #24694, .T. ) ;
#17271 = CARTESIAN_POINT ( 'NONE',  ( -2.820898088245517688, -4.403288343584588205, -19.70544088820000184 ) ) ;
#17272 = CARTESIAN_POINT ( 'NONE',  ( 28.43005475791858672, 2.264356203195492689, 8.000000000000007105 ) ) ;
#17273 = CARTESIAN_POINT ( 'NONE',  ( -16.81341597756113515, 9.900182044522454206, -1.000005633855494125E-09 ) ) ;
#17274 = CARTESIAN_POINT ( 'NONE',  ( -7.877322421349998827, 9.296057209389999798, 230.6412452697800006 ) ) ;
#17275 = LINE ( 'NONE', #22474, #21211 ) ;
#17276 = CARTESIAN_POINT ( 'NONE',  ( -3.501023913647623331, -3.402888588040827500, -46.45083066912499703 ) ) ;
#17277 = CARTESIAN_POINT ( 'NONE',  ( -7.999999999984332533, -116.7459945346252113, 11.01907316483054622 ) ) ;
#17278 = CARTESIAN_POINT ( 'NONE',  ( 0.8466629623219488199, -26.78674366391425110, 224.2963572738258904 ) ) ;
#17279 = LINE ( 'NONE', #2362, #746 ) ;
#17280 = CARTESIAN_POINT ( 'NONE',  ( -26.81201737230000148, 9.375055877170000329, 229.1414213529999984 ) ) ;
#17281 = AXIS2_PLACEMENT_3D ( 'NONE', #12667, #11056, #428 ) ;
#17282 = ADVANCED_FACE ( 'NONE', ( #13446 ), #20532, .F. ) ;
#17283 = AXIS2_PLACEMENT_3D ( 'NONE', #10169, #5440, #22281 ) ;
#17284 = VECTOR ( 'NONE', #1787, 1000.000000000000000 ) ;
#17285 = DIRECTION ( 'NONE',  ( 0.000000000000000000, 0.000000000000000000, -1.000000000000000000 ) ) ;
#17286 = ORIENTED_EDGE ( 'NONE', *, *, #22747, .T. ) ;
#17287 = AXIS2_PLACEMENT_3D ( 'NONE', #9070, #1845, #7178 ) ;
#17288 = CARTESIAN_POINT ( 'NONE',  ( -5.505691776210679400, -0.009179722898969058451, -29.16856466010000304 ) ) ;
#17289 = B_SPLINE_CURVE_WITH_KNOTS ( 'NONE', 5,
 ( #23919, #2199, #28464, #19179, #6900, #16503, #9582, #6257, #7063 ),
 .UNSPECIFIED., .F., .F.,
 ( 6, 3, 6 ),
 ( 0.000000000000000000, 1.211913930199999934, 1.514808573670000102 ),
 .UNSPECIFIED. ) ;
#17290 = VERTEX_POINT ( 'NONE', #30291 ) ;
#17291 = CARTESIAN_POINT ( 'NONE',  ( -9.999999999969999109, -43.95328087550000618, -27.24755286569999768 ) ) ;
#17292 = CARTESIAN_POINT ( 'NONE',  ( 4.880217822150678231, -0.7240669684095875080, -46.88818262062500963 ) ) ;
#17293 = ORIENTED_EDGE ( 'NONE', *, *, #2701, .T. ) ;
#17294 = VERTEX_POINT ( 'NONE', #25577 ) ;
#17295 = VERTEX_POINT ( 'NONE', #10938 ) ;
#17296 = CARTESIAN_POINT ( 'NONE',  ( 20.25970996295725968, 20.00000589292579534, 229.3324148076499114 ) ) ;
#17297 = EDGE_LOOP ( 'NONE', ( #12885, #10067, #30963, #6671 ) ) ;
#17298 = MECHANICAL_DESIGN_GEOMETRIC_PRESENTATION_REPRESENTATION (  '', ( #17802 ), #26874 ) ;
#17299 = CARTESIAN_POINT ( 'NONE',  ( 8.000000000658319621, -14.18526619378945774, -37.39743501090877942 ) ) ;
#17300 = CARTESIAN_POINT ( 'NONE',  ( -4.861312627776433359, -11.03139726553092892, -35.43660304873223765 ) ) ;
#17301 = CARTESIAN_POINT ( 'NONE',  ( -8.699999999715885224, -26.99999999997790923, -28.40000000002690683 ) ) ;
#17302 = CARTESIAN_POINT ( 'NONE',  ( 1.629408644310613052, 4.659406692139858919, -35.70000000000000284 ) ) ;
#17303 = DIRECTION ( 'NONE',  ( 0.000000000000000000, 0.000000000000000000, 1.000000000000000000 ) ) ;
#17304 = CARTESIAN_POINT ( 'NONE',  ( -3.679671488369449683, -1.085031249664836439, -0.6999999999999991784 ) ) ;
#17305 = CARTESIAN_POINT ( 'NONE',  ( 5.114250173790000353, 17.43050733020000109, 230.6999999999999886 ) ) ;
#17306 = TOROIDAL_SURFACE ( 'NONE', #1234, 24.50000000000000000, 3.200000000000000178 ) ;
#17307 = CARTESIAN_POINT ( 'NONE',  ( -10.69999999996291251, -37.77860098318037529, -25.96937563633603574 ) ) ;
#17308 = AXIS2_PLACEMENT_3D ( 'NONE', #21515, #21674, #19308 ) ;
#17309 = EDGE_CURVE ( 'NONE', #3457, #29133, #9517, .T. ) ;
#17310 = VECTOR ( 'NONE', #22052, 1000.000000000000000 ) ;
#17311 = CARTESIAN_POINT ( 'NONE',  ( -4.345037505360560992, 2.733239894040710105, -11.38297590280000016 ) ) ;
#17312 = CARTESIAN_POINT ( 'NONE',  ( -2.705882613314523955, 5.963358562559473164, -31.72635571290000200 ) ) ;
#17313 = VECTOR ( 'NONE', #20027, 1000.000000000000114 ) ;
#17314 = CARTESIAN_POINT ( 'NONE',  ( 3.771189585364855379, -0.9962994085146968937, -69.24095287807548971 ) ) ;
#17315 = DIRECTION ( 'NONE',  ( 0.000000000000000000, 0.000000000000000000, -1.000000000000000000 ) ) ;
#17316 = CARTESIAN_POINT ( 'NONE',  ( 20.30396079662882158, 20.00000000004802203, 1.000000000000000888 ) ) ;
#17317 = CARTESIAN_POINT ( 'NONE',  ( -3.072394438959999974, -1.678456730820000020, 227.6468472915199754 ) ) ;
#17318 = CARTESIAN_POINT ( 'NONE',  ( 1.089891362629999971, -28.47934442809999922, 225.3101849020000031 ) ) ;
#17319 = CARTESIAN_POINT ( 'NONE',  ( 8.903108651239925564, -22.82508830966962421, 40.00000000000000000 ) ) ;
#17320 = CARTESIAN_POINT ( 'NONE',  ( -1.598721155459999804E-14, 0.000000000000000000, -0.6999999999999992895 ) ) ;
#17321 = CARTESIAN_POINT ( 'NONE',  ( -24.05769994060051786, -13.93129956160059102, 3.997248602000014195 ) ) ;
#17322 = LINE ( 'NONE', #9785, #26374 ) ;
#17323 = CIRCLE ( 'NONE', #6274, 2.999999999999999556 ) ;
#17324 = ORIENTED_EDGE ( 'NONE', *, *, #7436, .F. ) ;
#17325 = EDGE_CURVE ( 'NONE', #12226, #18212, #27759, .T. ) ;
#17326 = EDGE_CURVE ( 'NONE', #6137, #6530, #24759, .T. ) ;
#17327 = FACE_OUTER_BOUND ( 'NONE', #20400, .T. ) ;
#17328 = CARTESIAN_POINT ( 'NONE',  ( -12.30769945475714344, -32.00000000000001421, -28.17921486638179829 ) ) ;
#17329 = ORIENTED_EDGE ( 'NONE', *, *, #25683, .T. ) ;
#17330 = EDGE_CURVE ( 'NONE', #25188, #4001, #16730, .T. ) ;
#17331 = CARTESIAN_POINT ( 'NONE',  ( 0.2762902770302890221, 2.100000000240000109, 226.6412452697799438 ) ) ;
#17332 = CARTESIAN_POINT ( 'NONE',  ( -8.699999999692932917, -26.69041892758821888, -31.40984194557997000 ) ) ;
#17333 = ORIENTED_EDGE ( 'NONE', *, *, #28604, .F. ) ;
#17334 = CARTESIAN_POINT ( 'NONE',  ( -4.865310089958662765, -0.9828511995358047981, -44.10000000002499121 ) ) ;
#17335 = VECTOR ( 'NONE', #22374, 1000.000000000000000 ) ;
#17336 = ORIENTED_EDGE ( 'NONE', *, *, #8713, .F. ) ;
#17337 = ORIENTED_EDGE ( 'NONE', *, *, #5548, .T. ) ;
#17338 = EDGE_CURVE ( 'NONE', #1526, #8364, #11714, .T. ) ;
#17339 = EDGE_LOOP ( 'NONE', ( #25153, #325, #20872, #19784 ) ) ;
#17340 = CARTESIAN_POINT ( 'NONE',  ( 26.80000000000000071, 3.019806626980000436E-14, 230.6999999999999886 ) ) ;
#17341 = DIRECTION ( 'NONE',  ( -0.9316362575375349842, 0.3633921898465292122, -0.000000000000000000 ) ) ;
#17342 = DIRECTION ( 'NONE',  ( 1.000000000000000000, -1.843431230204166689E-12, 2.650498504954120002E-12 ) ) ;
#17343 = VERTEX_POINT ( 'NONE', #7148 ) ;
#17344 = DIRECTION ( 'NONE',  ( 2.965499939100700266E-25, -1.000000000000000000, 2.257145581549900232E-12 ) ) ;
#17345 = CARTESIAN_POINT ( 'NONE',  ( 4.785280386532176244, 31.71089591181006639, 8.000000000000007105 ) ) ;
#17346 = EDGE_CURVE ( 'NONE', #24268, #8147, #18788, .T. ) ;
#17347 = CARTESIAN_POINT ( 'NONE',  ( -17.49266624248391722, -32.00021425718040291, -28.17511218750900071 ) ) ;
#17348 = AXIS2_PLACEMENT_3D ( 'NONE', #25995, #15762, #30239 ) ;
#17349 = CARTESIAN_POINT ( 'NONE',  ( 11.39269908143662491, 20.99999999989801225, -70.09999999997381792 ) ) ;
#17350 = CARTESIAN_POINT ( 'NONE',  ( -2.183849900456023896, 3.899926742306373928, -16.67761783620000315 ) ) ;
#17351 = CARTESIAN_POINT ( 'NONE',  ( -18.95046173579999760, -18.95046173579999760, 193.2171415880000040 ) ) ;
#17352 = CARTESIAN_POINT ( 'NONE',  ( 24.29878022517171132, 13.50606022452295996, 5.558728318588544326 ) ) ;
#17353 = DIRECTION ( 'NONE',  ( 1.000000000000000000, -1.224606353820000075E-16, 0.000000000000000000 ) ) ;
#17354 = CARTESIAN_POINT ( 'NONE',  ( 9.500000000000000000, 20.99999999999999645, -64.10000000019999788 ) ) ;
#17355 = CARTESIAN_POINT ( 'NONE',  ( -24.58829991325495001, 12.97289974774663790, 4.038486474265504000 ) ) ;
#17356 = ADVANCED_FACE ( 'NONE', ( #16436 ), #29285, .T. ) ;
#17357 = CARTESIAN_POINT ( 'NONE',  ( -10.69999999999999929, -25.07023973440000120, -30.70263567090000123 ) ) ;
#17358 = CARTESIAN_POINT ( 'NONE',  ( 21.43444001219999961, 17.18614031629999772, 229.9751245449999999 ) ) ;
#17359 = DIRECTION ( 'NONE',  ( 1.000000000000000000, -1.224606353820000075E-16, 0.000000000000000000 ) ) ;
#17360 = VERTEX_POINT ( 'NONE', #16584 ) ;
#17361 = CARTESIAN_POINT ( 'NONE',  ( -5.473210459063365896, -0.1384095708982860384, -52.75673954922498865 ) ) ;
#17362 = CARTESIAN_POINT ( 'NONE',  ( -8.699999999662093586, -15.94902145834643115, -35.53273252493492862 ) ) ;
#17363 = CARTESIAN_POINT ( 'NONE',  ( -21.50791824780870698, 17.12055895076685630, 0.02487541500001411165 ) ) ;
#17364 = CARTESIAN_POINT ( 'NONE',  ( -4.747698592653731176, 0.5343720360068521247, -68.10000000002500542 ) ) ;
#17365 = PRODUCT_DEFINITION_FORMATION_WITH_SPECIFIED_SOURCE ( 'ANY', '', #1288, .NOT_KNOWN. ) ;
#17366 = ORIENTED_EDGE ( 'NONE', *, *, #26679, .F. ) ;
#17367 = SURFACE_STYLE_USAGE ( .BOTH. , #10451 ) ;
#17368 = VERTEX_POINT ( 'NONE', #2434 ) ;
#17369 = DIRECTION ( 'NONE',  ( 0.7071067811865475727, -0.7071067811865475727, 0.000000000000000000 ) ) ;
#17370 = DIRECTION ( 'NONE',  ( 0.000000000000000000, 0.000000000000000000, 1.000000000000000000 ) ) ;
#17371 = VERTEX_POINT ( 'NONE', #23839 ) ;
#17372 = CARTESIAN_POINT ( 'NONE',  ( 2.450607853129171954, -3.579122932049592976, -27.63292313650000054 ) ) ;
#17373 = CARTESIAN_POINT ( 'NONE',  ( -9.738910687886855655, -24.96785170200598714, 115.0000000000000000 ) ) ;
#17374 = B_SPLINE_CURVE_WITH_KNOTS ( 'NONE', 3,
 ( #25484, #18545, #13189, #20752, #30359, #13673 ),
 .UNSPECIFIED., .F., .F.,
 ( 4, 2, 4 ),
 ( 0.000000000000000000, 0.5000000000000000000, 1.000000000000000000 ),
 .UNSPECIFIED. ) ;
#17375 = B_SPLINE_CURVE_WITH_KNOTS ( 'NONE', 3,
 ( #10753, #23038, #3665, #9434, #23192, #19037, #1484, #26279, #15944, #7080 ),
 .UNSPECIFIED., .F., .F.,
 ( 4, 2, 2, 2, 4 ),
 ( 0.000000000000000000, 0.2500000000000000555, 0.5000000000000001110, 0.7500000000000002220, 1.000000000000000000 ),
 .UNSPECIFIED. ) ;
#17376 = CARTESIAN_POINT ( 'NONE',  ( -25.57973247310144771, 13.96556750272910641, 0.7595836940000044724 ) ) ;
#17377 = EDGE_CURVE ( 'NONE', #30573, #19165, #19233, .T. ) ;
#17378 = CARTESIAN_POINT ( 'NONE',  ( 11.20000000009999930, -22.00000000000000000, -25.51324865394999719 ) ) ;
#17379 = CARTESIAN_POINT ( 'NONE',  ( -27.63177371730000331, 3.383804566159999695E-15, 192.6394760439999914 ) ) ;
#17380 = CARTESIAN_POINT ( 'NONE',  ( 26.80000000000000071, -3.552713678799999608E-15, 193.2171415880000040 ) ) ;
#17381 = VERTEX_POINT ( 'NONE', #2584 ) ;
#17382 = EDGE_CURVE ( 'NONE', #27477, #7336, #5657, .T. ) ;
#17383 = CARTESIAN_POINT ( 'NONE',  ( 24.81746042554890863, -14.01353061607344053, 3.920132063000014710 ) ) ;
#17384 = EDGE_CURVE ( 'NONE', #6179, #10144, #16275, .T. ) ;
#17385 = EDGE_CURVE ( 'NONE', #15899, #16404, #15203, .T. ) ;
#17386 = DIRECTION ( 'NONE',  ( -1.000000000000000000, 0.000000000000000000, 0.000000000000000000 ) ) ;
#17387 = ORIENTED_EDGE ( 'NONE', *, *, #17755, .F. ) ;
#17388 = CARTESIAN_POINT ( 'NONE',  ( 14.80403571754988512, -31.99970031113917557, -29.28999737812765147 ) ) ;
#17389 = CARTESIAN_POINT ( 'NONE',  ( -24.34942396232675321, -13.41447636113284680, 5.310538869999992251 ) ) ;
#17390 = CARTESIAN_POINT ( 'NONE',  ( -8.999999999559999964, 21.70000000000000284, -64.10000000000000853 ) ) ;
#17391 = LINE ( 'NONE', #22122, #9737 ) ;
#17392 = CARTESIAN_POINT ( 'NONE',  ( -9.777910867663793582, -7.131609927916758629, 232.0000000000046612 ) ) ;
#17393 = DIRECTION ( 'NONE',  ( 0.8090169943751909232, 0.5877852522921378498, 0.000000000000000000 ) ) ;
#17394 = CARTESIAN_POINT ( 'NONE',  ( 2.129400989689198997, -3.370417416381545905, -0.6999999999999992895 ) ) ;
#17395 = CARTESIAN_POINT ( 'NONE',  ( -25.74089749696337037, -15.38097739005167419, 0.5017677510000262409 ) ) ;
#17396 = DIRECTION ( 'NONE',  ( 5.962915006522622422E-16, 0.4383711467890810676, 0.8987940462991651502 ) ) ;
#17397 = DIRECTION ( 'NONE',  ( 0.000000000000000000, 1.000000000000000000, 0.000000000000000000 ) ) ;
#17398 = CARTESIAN_POINT ( 'NONE',  ( -9.689803781819808393, -24.98716455116955970, 26.94264034010273434 ) ) ;
#17399 = CARTESIAN_POINT ( 'NONE',  ( -0.4846640835383786983, -27.79604706135651782, 5.506468674000009500 ) ) ;
#17400 = ORIENTED_EDGE ( 'NONE', *, *, #27403, .T. ) ;
#17401 = CARTESIAN_POINT ( 'NONE',  ( -8.999999999699999975, 21.69999999929999390, -51.10000000000999876 ) ) ;
#17402 =( NAMED_UNIT ( * ) PLANE_ANGLE_UNIT ( ) SI_UNIT ( $, .RADIAN. ) );
#17403 = SHAPE_REPRESENTATION ( 'Plunger Rod', ( #17722 ), #27910 ) ;
#17404 = CARTESIAN_POINT ( 'NONE',  ( 24.69936741169999905, -14.21947533890000059, 226.1000014189999945 ) ) ;
#17405 = CARTESIAN_POINT ( 'NONE',  ( -4.069925668896384963, 4.914984763948436530, -62.99933298482500277 ) ) ;
#17406 = ORIENTED_EDGE ( 'NONE', *, *, #21512, .T. ) ;
#17407 = VERTEX_POINT ( 'NONE', #9659 ) ;
#17408 = CARTESIAN_POINT ( 'NONE',  ( -4.622623965551615477, -30.63307358560974336, 0.2686722299999888541 ) ) ;
#17409 = VERTEX_POINT ( 'NONE', #19263 ) ;
#17410 = EDGE_LOOP ( 'NONE', ( #13348, #13784, #22546, #11310 ) ) ;
#17411 = CARTESIAN_POINT ( 'NONE',  ( 17.14656078599760392, 12.09981795542235439, -0.6999999999999784173 ) ) ;
#17412 = CARTESIAN_POINT ( 'NONE',  ( -24.93720648713954446, 13.79881813474513486, 3.899998581000013509 ) ) ;
#17413 = CARTESIAN_POINT ( 'NONE',  ( -18.95046173579999760, -18.95046173579999760, 143.2171415880000040 ) ) ;
#17414 = B_SPLINE_CURVE_WITH_KNOTS ( 'NONE', 3,
 ( #7704, #17609, #7855, #19979, #17307, #181, #7558, #14957, #2994, #24703 ),
 .UNSPECIFIED., .F., .F.,
 ( 4, 2, 2, 2, 4 ),
 ( 0.000000000000000000, 0.2500000000000000000, 0.5000000000000000000, 0.7500000000000000000, 1.000000000000000000 ),
 .UNSPECIFIED. ) ;
#17415 = CARTESIAN_POINT ( 'NONE',  ( 3.378474288950000126, 11.51459527090000101, 231.9999991140000191 ) ) ;
#17416 =( REPRESENTATION_RELATIONSHIP ('NONE','NONE', #2712, #527 ) REPRESENTATION_RELATIONSHIP_WITH_TRANSFORMATION ( #22141 )SHAPE_REPRESENTATION_RELATIONSHIP( ) );
#17417 = CARTESIAN_POINT ( 'NONE',  ( 24.95427444975690889, -13.76797447160702070, 6.099998581000020792 ) ) ;
#17418 = CARTESIAN_POINT ( 'NONE',  ( -3.409041349409528632, -3.412796932024714014, -8.876491631000003935 ) ) ;
#17419 = ADVANCED_FACE ( 'NONE', ( #30759 ), #26498, .F. ) ;
#17420 = DIRECTION ( 'NONE',  ( 0.000000000000000000, 1.000000000000000000, 0.000000000000000000 ) ) ;
#17421 = VERTEX_POINT ( 'NONE', #24452 ) ;
#17422 = CARTESIAN_POINT ( 'NONE',  ( 2.578787959589605716, -3.990362813461365121, -44.10000000002499121 ) ) ;
#17423 = CARTESIAN_POINT ( 'NONE',  ( 28.49528339128749366, 0.5184828350247212558, 1.000000000000000888 ) ) ;
#17424 = AXIS2_PLACEMENT_3D ( 'NONE', #31051, #28992, #19561 ) ;
#17425 = CARTESIAN_POINT ( 'NONE',  ( 0.2309929099465271585, 4.358477053493584386, -22.94418644579999977 ) ) ;
#17426 = CARTESIAN_POINT ( 'NONE',  ( -12.75378086759999796, -22.00000000000000000, -31.28675134614999820 ) ) ;
#17427 = CARTESIAN_POINT ( 'NONE',  ( -8.699999999691694796, -25.92947359974585098, -31.20249410827203107 ) ) ;
#17428 = ADVANCED_BREP_SHAPE_REPRESENTATION ( '', ( #10658, #17722 ), #14824 ) ;
#17429 = CARTESIAN_POINT ( 'NONE',  ( 9.999999999966100006, -30.00000000000020606, -28.79269908146310186 ) ) ;
#17430 = LINE ( 'NONE', #19803, #2128 ) ;
#17431 = CARTESIAN_POINT ( 'NONE',  ( 5.643028086411650435, 2.011589847869324377, -45.92627377572500080 ) ) ;
#17432 = CARTESIAN_POINT ( 'NONE',  ( -10.69999999999999929, -124.6960077043000013, -32.36679061319999562 ) ) ;
#17433 = DIRECTION ( 'NONE',  ( 0.000000000000000000, 0.000000000000000000, 1.000000000000000000 ) ) ;
#17434 = CARTESIAN_POINT ( 'NONE',  ( 10.69999999999999929, -130.0000000000000000, -42.39999999999999858 ) ) ;
#17435 = CARTESIAN_POINT ( 'NONE',  ( -22.29514036694590118, -14.89751301532326444, 43.21714158846668141 ) ) ;
#17436 = EDGE_CURVE ( 'NONE', #15429, #1748, #27115, .T. ) ;
#17437 = CARTESIAN_POINT ( 'NONE',  ( -1.484924240490000047, 1.484924240490000047, 226.6412452697800006 ) ) ;
#17438 = ORIENTED_EDGE ( 'NONE', *, *, #16254, .F. ) ;
#17439 = CARTESIAN_POINT ( 'NONE',  ( 4.634019325638258024, 0.4639887426745141208, -30.13116556700000714 ) ) ;
#17440 = ORIENTED_EDGE ( 'NONE', *, *, #13819, .T. ) ;
#17441 = CARTESIAN_POINT ( 'NONE',  ( 24.70448873180906446, -12.74983733560190302, 4.239730452999995514 ) ) ;
#17442 = CARTESIAN_POINT ( 'NONE',  ( 2.990129296507525680, -3.859048371143013245, -53.25430438132500655 ) ) ;
#17443 = ORIENTED_EDGE ( 'NONE', *, *, #24537, .F. ) ;
#17444 = EDGE_CURVE ( 'NONE', #18378, #28697, #1802, .T. ) ;
#17445 = ORIENTED_EDGE ( 'NONE', *, *, #26724, .T. ) ;
#17446 = AXIS2_PLACEMENT_3D ( 'NONE', #30859, #23162, #23315 ) ;
#17447 = PRODUCT_CONTEXT ( 'NONE', #943, 'mechanical' ) ;
#17448 = VERTEX_POINT ( 'NONE', #9976 ) ;
#17449 = AXIS2_PLACEMENT_3D ( 'NONE', #7970, #758, #19942 ) ;
#17450 = ORIENTED_EDGE ( 'NONE', *, *, #10034, .T. ) ;
#17451 = CARTESIAN_POINT ( 'NONE',  ( 24.43762869010000216, -14.66515636309999948, 226.0027499809999938 ) ) ;
#17452 = CARTESIAN_POINT ( 'NONE',  ( -17.93324555120827668, 10.97998838178171432, -0.6999999999999784173 ) ) ;
#17453 = DIRECTION ( 'NONE',  ( 1.000000000000000000, -1.843431230198065424E-12, 2.650498504953516580E-12 ) ) ;
#17454 = PLANE ( 'NONE',  #10944 ) ;
#17455 = CARTESIAN_POINT ( 'NONE',  ( -12.34115088265029669, -30.17434508811917127, -24.45955028003077913 ) ) ;
#17456 = CARTESIAN_POINT ( 'NONE',  ( -5.082955080895779965, -0.02874842474374714185, -0.6999999999999992895 ) ) ;
#17457 = DIRECTION ( 'NONE',  ( 0.000000000000000000, 2.257145581549999994E-12, 1.000000000000000000 ) ) ;
#17458 = CARTESIAN_POINT ( 'NONE',  ( -9.738910687886855655, -24.96785170200598714, 115.0000000000000000 ) ) ;
#17459 = B_SPLINE_CURVE_WITH_KNOTS ( 'NONE', 3,
 ( #15457, #17507, #17651, #22553 ),
 .UNSPECIFIED., .F., .F.,
 ( 4, 4 ),
 ( 0.000000000000000000, 1.000000000000000000 ),
 .UNSPECIFIED. ) ;
#17460 = CARTESIAN_POINT ( 'NONE',  ( 2.789765316938662476, -3.934254546267435426, -13.06138893670000023 ) ) ;
#17461 = CARTESIAN_POINT ( 'NONE',  ( 3.999349870826697018, -3.799712354642017509, -29.05126389020000133 ) ) ;
#17462 = CARTESIAN_POINT ( 'NONE',  ( 0.8746022926037627654, -27.78660248490213291, 225.6820510556075590 ) ) ;
#17463 = EDGE_CURVE ( 'NONE', #26986, #26129, #14860, .T. ) ;
#17464 = CARTESIAN_POINT ( 'NONE',  ( 23.77307140678977504, -14.41181874416537134, 4.999998581000003384 ) ) ;
#17465 = CARTESIAN_POINT ( 'NONE',  ( 17.83931306984926835, 20.00000000000176570, -0.6999999999999784173 ) ) ;
#17466 = CARTESIAN_POINT ( 'NONE',  ( -2.595403069806114793, -2.504630016969688011, 227.7079405341370091 ) ) ;
#17467 = CARTESIAN_POINT ( 'NONE',  ( 28.49530731802708416, 0.5184832703811660393, 8.000000000000007105 ) ) ;
#17468 = CARTESIAN_POINT ( 'NONE',  ( -4.215937884789293655, -1.105999120962562809, -25.04656121680000425 ) ) ;
#17469 = VECTOR ( 'NONE', #3993, 1000.000000000000000 ) ;
#17470 = VECTOR ( 'NONE', #11267, 1000.000000000000000 ) ;
#17471 = CYLINDRICAL_SURFACE ( 'NONE', #26287, 26.80000000000000071 ) ;
#17472 = CARTESIAN_POINT ( 'NONE',  ( 14.73745037969879590, -25.71390008926000448, -23.36904195206612656 ) ) ;
#17473 = DIRECTION ( 'NONE',  ( 5.962915006522622422E-16, 0.4383711467890810676, 0.8987940462991651502 ) ) ;
#17474 = CIRCLE ( 'NONE', #913, 1.700000000000000178 ) ;
#17475 = ORIENTED_EDGE ( 'NONE', *, *, #20348, .T. ) ;
#17476 = LINE ( 'NONE', #22064, #18298 ) ;
#17477 = CARTESIAN_POINT ( 'NONE',  ( 13.92191802967587577, 20.99999999989822186, -67.88524365365343272 ) ) ;
#17478 = VERTEX_POINT ( 'NONE', #26652 ) ;
#17479 = CARTESIAN_POINT ( 'NONE',  ( 27.89542231038745257, 7.122393016134455301, 8.000000000000007105 ) ) ;
#17480 = CARTESIAN_POINT ( 'NONE',  ( 7.963158867438391297, -115.4064749715892617, 21.31606477568482916 ) ) ;
#17481 = ORIENTED_EDGE ( 'NONE', *, *, #4787, .T. ) ;
#17482 = CARTESIAN_POINT ( 'NONE',  ( -4.602032322722164892, 0.8949949322525938555, -44.10000000002499831 ) ) ;
#17483 = ORIENTED_EDGE ( 'NONE', *, *, #2753, .T. ) ;
#17484 = EDGE_CURVE ( 'NONE', #8183, #26174, #21752, .T. ) ;
#17485 = EDGE_LOOP ( 'NONE', ( #8692, #6029, #14481, #28286 ) ) ;
#17486 = AXIS2_PLACEMENT_3D ( 'NONE', #10847, #20433, #22647 ) ;
#17487 =( NAMED_UNIT ( * ) PLANE_ANGLE_UNIT ( ) SI_UNIT ( $, .RADIAN. ) );
#17488 = ORIENTED_EDGE ( 'NONE', *, *, #14073, .F. ) ;
#17489 = CARTESIAN_POINT ( 'NONE',  ( 27.34838611700000044, 9.577833257040001769, 229.7625741969999922 ) ) ;
#17490 = CYLINDRICAL_SURFACE ( 'NONE', #17168, 1.100000000000000089 ) ;
#17491 = CARTESIAN_POINT ( 'NONE',  ( -10.69999999999999929, -24.97510340920000260, -26.18620021100000272 ) ) ;
#17492 = ORIENTED_EDGE ( 'NONE', *, *, #5330, .T. ) ;
#17493 = CARTESIAN_POINT ( 'NONE',  ( -24.35797963555383205, 13.39969403207715892, 6.098655031999994591 ) ) ;
#17494 = AXIS2_PLACEMENT_3D ( 'NONE', #6850, #1832, #25910 ) ;
#17495 = CARTESIAN_POINT ( 'NONE',  ( 10.82908725742651512, -27.76276047461856322, 143.2171415880000040 ) ) ;
#17496 = AXIS2_PLACEMENT_3D ( 'NONE', #28425, #4515, #21349 ) ;
#17497 = CARTESIAN_POINT ( 'NONE',  ( 3.160606383828830968, -27.32265456628853784, 209.9517185872548453 ) ) ;
#17498 = CARTESIAN_POINT ( 'NONE',  ( 24.15870318760000046, -15.11998207899999969, 224.4930104139999969 ) ) ;
#17499 = EDGE_CURVE ( 'NONE', #19704, #30881, #29008, .T. ) ;
#17500 = EDGE_CURVE ( 'NONE', #23358, #2527, #8660, .T. ) ;
#17501 = FACE_OUTER_BOUND ( 'NONE', #25921, .T. ) ;
#17502 = CARTESIAN_POINT ( 'NONE',  ( -3.331422745097512017, -2.438398348906446689, -18.87254627010000263 ) ) ;
#17503 = CARTESIAN_POINT ( 'NONE',  ( -0.5615373373075090990, -28.49504780676721438, 224.0344865918038977 ) ) ;
#17504 = DIRECTION ( 'NONE',  ( -3.924189347185961537E-12, 0.4082287037029530552, 0.9128796883888952163 ) ) ;
#17505 = CARTESIAN_POINT ( 'NONE',  ( -12.75378086759999796, -27.00000000000000355, -34.17350269210000135 ) ) ;
#17506 = CYLINDRICAL_SURFACE ( 'NONE', #18240, 3.000000000000002220 ) ;
#17507 = CARTESIAN_POINT ( 'NONE',  ( -12.24453640261407905, 20.99999999997362821, -55.78347656086990725 ) ) ;
#17508 = EDGE_CURVE ( 'NONE', #30054, #22831, #4164, .T. ) ;
#17509 = CARTESIAN_POINT ( 'NONE',  ( -11.08346179031913437, -28.41490585489480480, 43.60555127550000520 ) ) ;
#17510 = CARTESIAN_POINT ( 'NONE',  ( 24.82944511390000031, 13.78896019219999936, 229.0000000000000000 ) ) ;
#17511 = CARTESIAN_POINT ( 'NONE',  ( 4.638687372223567529, -9.716283825201511348, -32.74022090981630839 ) ) ;
#17512 = ORIENTED_EDGE ( 'NONE', *, *, #29311, .F. ) ;
#17513 = CARTESIAN_POINT ( 'NONE',  ( -5.325262776966551037, 2.643762325382846612, -56.79877225282499609 ) ) ;
#17514 = AXIS2_PLACEMENT_3D ( 'NONE', #15740, #20161, #22674 ) ;
#17515 = CARTESIAN_POINT ( 'NONE',  ( 21.13530760622424864, 17.06006193249097436, 0.000000000000000000 ) ) ;
#17516 = CARTESIAN_POINT ( 'NONE',  ( -21.27524652179786457, 16.93536700441368126, 0.000000000000000000 ) ) ;
#17518 = ADVANCED_FACE ( 'NONE', ( #26805 ), #14701, .F. ) ;
#17517 = VECTOR ( 'NONE', #17578, 1000.000000000000000 ) ;
#17519 = CARTESIAN_POINT ( 'NONE',  ( -4.207018160331792878, 0.5698972141343202624, -68.10000000002500542 ) ) ;
#17520 = ORIENTED_EDGE ( 'NONE', *, *, #4072, .F. ) ;
#17521 = CARTESIAN_POINT ( 'NONE',  ( -2.657516869754243061, -0.4832168877570500176, -97.49610867634444844 ) ) ;
#17522 = ORIENTED_EDGE ( 'NONE', *, *, #29847, .T. ) ;
#17523 = CYLINDRICAL_SURFACE ( 'NONE', #19000, 1.100000000000002309 ) ;
#17524 = DIRECTION ( 'NONE',  ( 2.257150022439999944E-12, 0.000000000000000000, 1.000000000000000000 ) ) ;
#17525 = VERTEX_POINT ( 'NONE', #12630 ) ;
#17526 = CARTESIAN_POINT ( 'NONE',  ( -3.112296099710467168, 3.758517760630106785, -62.59933298492499887 ) ) ;
#17527 = EDGE_CURVE ( 'NONE', #27200, #6537, #5514, .T. ) ;
#17528 = CARTESIAN_POINT ( 'NONE',  ( -13.25572673970000004, -26.61578565920000017, 230.0000000000000000 ) ) ;
#17529 = AXIS2_PLACEMENT_3D ( 'NONE', #15677, #20243, #5617 ) ;
#17530 = CARTESIAN_POINT ( 'NONE',  ( 4.117846205589234643, 1.989599136607407504, -66.85315453642499506 ) ) ;
#17531 = CARTESIAN_POINT ( 'NONE',  ( 11.00000000000000000, 25.22617105830878614, -61.82510970417090590 ) ) ;
#17532 = CARTESIAN_POINT ( 'NONE',  ( -4.861312627816332999, -17.81361358224843627, -28.79088930694037884 ) ) ;
#17533 = VERTEX_POINT ( 'NONE', #12792 ) ;
#17534 = CARTESIAN_POINT ( 'NONE',  ( 4.041451884329999800, 2.220446049249999755E-16, 230.5235986622430175 ) ) ;
#17535 = AXIS2_PLACEMENT_3D ( 'NONE', #20377, #29968, #1505 ) ;
#17536 = CARTESIAN_POINT ( 'NONE',  ( 19.79266700209999996, 19.51190850369999907, 229.1494847489999813 ) ) ;
#17537 = ORIENTED_EDGE ( 'NONE', *, *, #4535, .F. ) ;
#17538 = DIRECTION ( 'NONE',  ( 1.666951178525963134E-12, -0.4082287037029531107, -0.9128796883888953273 ) ) ;
#17539 = CARTESIAN_POINT ( 'NONE',  ( -24.96253706803760153, -13.75225324404262572, 5.310538869999992251 ) ) ;
#17540 = CARTESIAN_POINT ( 'NONE',  ( 23.24663841809999809, -14.69162354060000020, 225.0000000000000000 ) ) ;
#17541 = CARTESIAN_POINT ( 'NONE',  ( 9.999999999962829733, -25.28360478509039311, -25.93233155165111370 ) ) ;
#17542 = CARTESIAN_POINT ( 'NONE',  ( -7.297190580108165570, -25.78810378223603195, 207.8834700269517270 ) ) ;
#17543 = CARTESIAN_POINT ( 'NONE',  ( -0.3657832974528221759, -3.774695518882208667, -0.6999999999999992895 ) ) ;
#17544 = CARTESIAN_POINT ( 'NONE',  ( -4.761646371388416732, -31.55428150781402508, 0.2374258030000131470 ) ) ;
#17545 = DIRECTION ( 'NONE',  ( -1.000000000000000000, 9.219999999999999084E-13, -4.710999999999999616E-12 ) ) ;
#17546 = PRESENTATION_STYLE_ASSIGNMENT (( #738 ) ) ;
#17547 = CARTESIAN_POINT ( 'NONE',  ( 0.000000000000000000, 0.000000000000000000, 115.0000000000000000 ) ) ;
#17548 = CARTESIAN_POINT ( 'NONE',  ( -8.966526567020544292, -25.25634759429105003, 24.42360803256879720 ) ) ;
#17549 = DIRECTION ( 'NONE',  ( 0.000000000000000000, 0.000000000000000000, -1.000000000000000000 ) ) ;
#17550 = EDGE_CURVE ( 'NONE', #18290, #23153, #27310, .T. ) ;
#17551 = ORIENTED_EDGE ( 'NONE', *, *, #19531, .F. ) ;
#17552 = CARTESIAN_POINT ( 'NONE',  ( 3.040504021322313122, 1.733590290792417887, -0.6999999999999784173 ) ) ;
#17553 = AXIS2_PLACEMENT_3D ( 'NONE', #30315, #16143, #30636 ) ;
#17554 = ADVANCED_FACE ( 'NONE', ( #19418 ), #15612, .F. ) ;
#17555 =( NAMED_UNIT ( * ) SI_UNIT ( $, .STERADIAN. ) SOLID_ANGLE_UNIT ( ) );
#17556 = CARTESIAN_POINT ( 'NONE',  ( 9.999999999977427834, -126.3827248121017419, -33.44530783663593354 ) ) ;
#17557 = EDGE_CURVE ( 'NONE', #30855, #24241, #16054, .T. ) ;
#17558 = CARTESIAN_POINT ( 'NONE',  ( -10.92933975387415302, -24.70409753101286654, -1.761594195916170946 ) ) ;
#17559 = CARTESIAN_POINT ( 'NONE',  ( 4.508719565894404369, 1.847421675581905953, -61.29141554682499304 ) ) ;
#17560 = EDGE_LOOP ( 'NONE', ( #13419, #12657, #7216, #23940 ) ) ;
#17561 = ORIENTED_EDGE ( 'NONE', *, *, #4678, .T. ) ;
#17562 = CLOSED_SHELL ( 'NONE', ( #28933, #27939, #1452, #13691, #5662, #20227, #18589, #16991, #220, #11174, #20060, #3527, #14529, #13512, #7532, #3865, #8077, #30711, #20144, #13620, #8421, #10726, #2413, #10348, #22657, #7754, #15035, #2491, #9459, #20049, #10671, #13614, #15516, #26425, #16152, #8870, #28857, #9673, #9221, #10405, #21298, #29316, #8196, #22019, #16031, #30512, #15401, #10921, #12761, #26984, #16193, #13143, #22284, #17037, #5687, #4056, #14670, #7547, #7198, #1706, #25711, #27975, #1332, #11642, #14264, #14077, #4745, #2200, #17719, #24450, #19805, #19585, #30290, #30974, #30945, #8171, #27016, #14880, #8022, #15368, #29421, #9568, #504, #21452, #15407, #30854, #8403, #16810, #19625, #2355, #22584, #11811, #5270, #6862, #5795, #15250, #14658, #5208, #15742, #3318, #27230, #1326, #5338, #25792, #10390, #9679, #3174, #21966, #21770, #28899, #24951, #5002, #8349, #30615, #3670, #2541, #10176, #9860, #3898, #2582 ) ) ;
#17563 = CARTESIAN_POINT ( 'NONE',  ( 26.97469346668950152, -9.357175201752722771, 0.000000000000000000 ) ) ;
#17564 = ORIENTED_EDGE ( 'NONE', *, *, #22922, .T. ) ;
#17565 = VERTEX_POINT ( 'NONE', #13723 ) ;
#17566 = CARTESIAN_POINT ( 'NONE',  ( -1.871191271462957495, 2.657633465977181420, -42.11318944236838036 ) ) ;
#17567 = CARTESIAN_POINT ( 'NONE',  ( 24.97129468909112404, -13.73710443560444183, 3.901342130000013064 ) ) ;
#17568 = CARTESIAN_POINT ( 'NONE',  ( -25.15375632540583695, -13.40010330548238926, 224.4391897960165068 ) ) ;
#17569 = UNCERTAINTY_MEASURE_WITH_UNIT (LENGTH_MEASURE( 1.000000000000000082E-05 ), #7363, 'distance_accuracy_value', 'NONE');
#17570 = CARTESIAN_POINT ( 'NONE',  ( 18.20094554413687504, 10.59899472509098040, -1.400000000000001910 ) ) ;
#17571 = CARTESIAN_POINT ( 'NONE',  ( 25.45799949673341800, -12.81261086040661645, 5.208434320000010942 ) ) ;
#17572 = CARTESIAN_POINT ( 'NONE',  ( 17.16657240419154462, 10.99999999996915179, -0.6999999999999784173 ) ) ;
#17573 = ORIENTED_EDGE ( 'NONE', *, *, #13910, .F. ) ;
#17574 = CARTESIAN_POINT ( 'NONE',  ( 2.781799176224414971, -3.750297231070458537, -44.10000000002499121 ) ) ;
#17575 = LINE ( 'NONE', #19946, #11769 ) ;
#17576 = CARTESIAN_POINT ( 'NONE',  ( 0.2925910193319765096, 5.520737601085913937, -23.94418644580000688 ) ) ;
#17577 = CARTESIAN_POINT ( 'NONE',  ( -12.30733375692050302, -24.30513431261573842, -32.61786866493986992 ) ) ;
#17578 = DIRECTION ( 'NONE',  ( 0.000000000000000000, -1.000000000000000000, 0.000000000000000000 ) ) ;
#17579 = CARTESIAN_POINT ( 'NONE',  ( 8.999999999770000869, 21.35000000010000321, -45.09999999954499827 ) ) ;
#17580 = CARTESIAN_POINT ( 'NONE',  ( -23.73488293864406629, -14.47501376178995258, 225.8859541126125237 ) ) ;
#17581 = CARTESIAN_POINT ( 'NONE',  ( 5.925978784015399903, -0.8792241758803844842, -46.13818262062499542 ) ) ;
#17582 = LINE ( 'NONE', #5788, #11728 ) ;
#17583 = CARTESIAN_POINT ( 'NONE',  ( 8.310304230308181772, -25.47941657935494675, 206.6944841980503043 ) ) ;
#17584 = CARTESIAN_POINT ( 'NONE',  ( -18.21696450012034063, 20.00000023631326229, 230.6811166311184422 ) ) ;
#17585 = CARTESIAN_POINT ( 'NONE',  ( -25.90058877277586902, -6.940365930346065859, 43.21714158835417408 ) ) ;
#17586 = EDGE_CURVE ( 'NONE', #14673, #23569, #23201, .T. ) ;
#17587 = CARTESIAN_POINT ( 'NONE',  ( 5.851800771450333727, -26.15706768910720470, 21.02145656915469019 ) ) ;
#17588 = VERTEX_POINT ( 'NONE', #18280 ) ;
#17589 = AXIS2_PLACEMENT_3D ( 'NONE', #2532, #16844, #6936 ) ;
#17590 = CARTESIAN_POINT ( 'NONE',  ( 3.503437880490057665, 2.636891074952370850, -32.86032172560000220 ) ) ;
#17591 = EDGE_CURVE ( 'NONE', #26756, #15714, #20738, .T. ) ;
#17592 = ORIENTED_EDGE ( 'NONE', *, *, #30970, .F. ) ;
#17593 = LINE ( 'NONE', #20267, #15268 ) ;
#17594 = CARTESIAN_POINT ( 'NONE',  ( 1.592968524163114852, 5.205024221813498109, -52.26125421252498882 ) ) ;
#17595 = EDGE_LOOP ( 'NONE', ( #22226, #16832, #16279, #11804 ) ) ;
#17596 = VERTEX_POINT ( 'NONE', #8679 ) ;
#17597 = CARTESIAN_POINT ( 'NONE',  ( 14.64818567264223326, -31.16543602876212304, 10.33864357293908931 ) ) ;
#17598 = ORIENTED_EDGE ( 'NONE', *, *, #22747, .F. ) ;
#17599 = ORIENTED_EDGE ( 'NONE', *, *, #11896, .F. ) ;
#17600 = CIRCLE ( 'NONE', #22136, 1.700000000000000178 ) ;
#17601 = CARTESIAN_POINT ( 'NONE',  ( 8.000000000284819279, -13.66682223737133128, -36.55330428412179344 ) ) ;
#17602 = CARTESIAN_POINT ( 'NONE',  ( -17.59696554489119080, -9.791838634853515799, 0.000000000000000000 ) ) ;
#17603 = DIRECTION ( 'NONE',  ( 0.000000000000000000, 1.000000000000000000, 0.000000000000000000 ) ) ;
#17604 = CARTESIAN_POINT ( 'NONE',  ( 5.245096043587340162, -0.2338077457563897399, -35.69999999999999574 ) ) ;
#17605 = CARTESIAN_POINT ( 'NONE',  ( 3.746497173757565413, -0.1670055334890632737, -35.69999999999999574 ) ) ;
#17606 = CARTESIAN_POINT ( 'NONE',  ( -19.80526803269999903, 19.50877411230000291, 227.0000000000000000 ) ) ;
#17607 = CARTESIAN_POINT ( 'NONE',  ( -4.088025854205739940, 2.308258268490227305, -0.6999999999999991784 ) ) ;
#17608 = DIRECTION ( 'NONE',  ( -0.000000000000000000, 1.000000000000000000, -2.255973188440000244E-12 ) ) ;
#17609 = CARTESIAN_POINT ( 'NONE',  ( -10.69999999996564632, -42.68530818349433531, -27.18110123272096601 ) ) ;
#17610 = DIRECTION ( 'NONE',  ( -0.000000000000000000, -0.000000000000000000, -1.000000000000000000 ) ) ;
#17611 = CARTESIAN_POINT ( 'NONE',  ( 3.316815470610420924, 4.395877990916175371, -15.22796858840000311 ) ) ;
#17612 = CARTESIAN_POINT ( 'NONE',  ( 1.456545767631101107, -4.104408573385627257, -30.25632401680000783 ) ) ;
#17613 = FACE_OUTER_BOUND ( 'NONE', #26768, .T. ) ;
#17614 = DIRECTION ( 'NONE',  ( 0.000000000000000000, -1.000000000000000000, 0.000000000000000000 ) ) ;
#17615 = PRESENTATION_STYLE_ASSIGNMENT (( #13201 ) ) ;
#17616 = DIRECTION ( 'NONE',  ( 2.966427579999808118E-12, 0.8902635789278698919, -0.4554456718803465143 ) ) ;
#17617 = CARTESIAN_POINT ( 'NONE',  ( -8.699999999732469291, -28.77621036647359887, -25.95065533197870167 ) ) ;
#17618 = ADVANCED_FACE ( 'NONE', ( #10589, #6332, #23021, #18121 ), #14916, .T. ) ;
#17619 = CARTESIAN_POINT ( 'NONE',  ( -28.50000000000000000, 3.490128108389999698E-15, 140.0000000000000000 ) ) ;
#17620 = CARTESIAN_POINT ( 'NONE',  ( 16.20123158649999695, -8.472631907100000248, -0.6999999999999992895 ) ) ;
#17621 = CYLINDRICAL_SURFACE ( 'NONE', #27865, 2.100000000000000977 ) ;
#17622 = ORIENTED_EDGE ( 'NONE', *, *, #24825, .F. ) ;
#17623 = CARTESIAN_POINT ( 'NONE',  ( 24.40022624086872938, 14.72688605419589614, 6.099998581000020792 ) ) ;
#17624 = CARTESIAN_POINT ( 'NONE',  ( -7.453090060300352704, -2.907137518772246132, 210.0000000000000284 ) ) ;
#17625 = VERTEX_POINT ( 'NONE', #23177 ) ;
#17626 = CARTESIAN_POINT ( 'NONE',  ( 28.49528339128749366, 0.5184828350247753237, 8.000000000000007105 ) ) ;
#17627 = CARTESIAN_POINT ( 'NONE',  ( 0.000000000000000000, 0.000000000000000000, 0.000000000000000000 ) ) ;
#17628 = EDGE_LOOP ( 'NONE', ( #23228, #26501 ) ) ;
#17629 = CARTESIAN_POINT ( 'NONE',  ( -6.112033042629958501, -26.81582465834875251, 21.02319148660755133 ) ) ;
#17630 = ORIENTED_EDGE ( 'NONE', *, *, #7365, .T. ) ;
#17631 = ORIENTED_EDGE ( 'NONE', *, *, #16565, .F. ) ;
#17632 =( LENGTH_UNIT ( ) NAMED_UNIT ( * ) SI_UNIT ( .MILLI., .METRE. ) );
#17633 = ORIENTED_EDGE ( 'NONE', *, *, #16638, .F. ) ;
#17634 = CARTESIAN_POINT ( 'NONE',  ( 28.04325408110000240, 2.413353885199999816E-14, 230.2432540810000319 ) ) ;
#17635 = CARTESIAN_POINT ( 'NONE',  ( -8.699999999693440955, -7.565603753652677455, -31.48340496202640892 ) ) ;
#17636 = CARTESIAN_POINT ( 'NONE',  ( -7.999999999660042604, -18.28443193496838504, -36.42483736938474692 ) ) ;
#17637 = VERTEX_POINT ( 'NONE', #6168 ) ;
#17638 = LINE ( 'NONE', #15445, #8383 ) ;
#17639 = B_SPLINE_CURVE_WITH_KNOTS ( 'NONE', 3,
 ( #9198, #14982, #670, #2708, #11575, #9947 ),
 .UNSPECIFIED., .F., .F.,
 ( 4, 2, 4 ),
 ( 0.000000000000000000, 0.5000000000000000000, 1.000000000000000000 ),
 .UNSPECIFIED. ) ;
#17640 = CARTESIAN_POINT ( 'NONE',  ( -24.09790742087466597, -13.86182010774420625, 5.963951780225244192 ) ) ;
#17641 = CARTESIAN_POINT ( 'NONE',  ( -7.620434517381760919, -5.659705516265826297, -27.22144157413186250 ) ) ;
#17642 = CARTESIAN_POINT ( 'NONE',  ( 24.11883219139999923, -15.18335225210000061, 224.6894478949999723 ) ) ;
#17643 = EDGE_CURVE ( 'NONE', #12999, #19402, #3648, .T. ) ;
#17644 = VECTOR ( 'NONE', #14927, 1000.000000000000114 ) ;
#17645 = CARTESIAN_POINT ( 'NONE',  ( 3.950106903291092930, 1.853988655799142959, -2.979170051700004151 ) ) ;
#17646 = CARTESIAN_POINT ( 'NONE',  ( -4.893571841047932303, 0.6806285466545627383, -18.31409460729999950 ) ) ;
#17647 = CARTESIAN_POINT ( 'NONE',  ( 27.79999999999999716, 2.355804440410000085E-11, 229.0000000000000000 ) ) ;
#17648 = CARTESIAN_POINT ( 'NONE',  ( -28.50000000000000000, 3.490128108389999698E-15, 40.00000000000000000 ) ) ;
#17649 = CARTESIAN_POINT ( 'NONE',  ( -27.92857142820000149, 5.329070518200000398E-15, 137.9396849850000137 ) ) ;
#17650 = CARTESIAN_POINT ( 'NONE',  ( -18.34692058799999970, 20.56908522310000009, 230.5592437530000041 ) ) ;
#17651 = CARTESIAN_POINT ( 'NONE',  ( -12.36063638108074692, 20.99999999997349676, -55.83941130196991054 ) ) ;
#17652 = EDGE_CURVE ( 'NONE', #13180, #23040, #1617, .T. ) ;
#17653 = CARTESIAN_POINT ( 'NONE',  ( 0.4822370985009165056, 3.496762477156720728, -0.6999999999999784173 ) ) ;
#17654 = CARTESIAN_POINT ( 'NONE',  ( -21.27753346980000160, -16.59085281950000379, 230.6999999999999886 ) ) ;
#17655 = DIRECTION ( 'NONE',  ( 1.224606353819999829E-16, 1.000000000000000000, 0.000000000000000000 ) ) ;
#17656 = ORIENTED_EDGE ( 'NONE', *, *, #28811, .F. ) ;
#17657 = CARTESIAN_POINT ( 'NONE',  ( 0.9634065801723908917, -5.189854773623245876, -57.99125695792501034 ) ) ;
#17658 = FACE_OUTER_BOUND ( 'NONE', #14750, .T. ) ;
#17659 = CARTESIAN_POINT ( 'NONE',  ( -5.530047734074942767, 3.478668956039820959, -10.44547590279999660 ) ) ;
#17660 = CARTESIAN_POINT ( 'NONE',  ( 13.73773747404255552, -26.37022765825810922, -0.6999999999999784173 ) ) ;
#17661 = CARTESIAN_POINT ( 'NONE',  ( -4.439243896310288484, 1.104759232538872205, -68.10000000002500542 ) ) ;
#17662 = EDGE_CURVE ( 'NONE', #24922, #22997, #9180, .T. ) ;
#17663 = VERTEX_POINT ( 'NONE', #28039 ) ;
#17664 = VERTEX_POINT ( 'NONE', #6483 ) ;
#17665 = CARTESIAN_POINT ( 'NONE',  ( 1.623446460547932624, 3.271163362686331233, -92.12187520236776095 ) ) ;
#17666 = AXIS2_PLACEMENT_3D ( 'NONE', #19343, #14622, #28932 ) ;
#17667 = VERTEX_POINT ( 'NONE', #10736 ) ;
#17668 = CARTESIAN_POINT ( 'NONE',  ( 7.999999999945623941, -115.1185614904247814, 21.95989595802063121 ) ) ;
#17669 = CARTESIAN_POINT ( 'NONE',  ( 23.23277120357798964, 15.26692725135965745, 4.999998581000003384 ) ) ;
#17670 = CARTESIAN_POINT ( 'NONE',  ( -5.505147662677075004, -0.2930537998028365232, -64.76421022022501006 ) ) ;
#17671 = CARTESIAN_POINT ( 'NONE',  ( -10.69999999999999929, -29.06671945329999929, -26.22544931050000017 ) ) ;
#17672 = CARTESIAN_POINT ( 'NONE',  ( -25.16978723329435397, 13.74175290767721691, -0.2432540810000105580 ) ) ;
#17673 = DIRECTION ( 'NONE',  ( 0.000000000000000000, 0.000000000000000000, 1.000000000000000000 ) ) ;
#17674 = ORIENTED_EDGE ( 'NONE', *, *, #19640, .T. ) ;
#17675 = CARTESIAN_POINT ( 'NONE',  ( 1.071233844162623683, -26.77863813579940455, 5.288095982889605473 ) ) ;
#17676 = EDGE_CURVE ( 'NONE', #25227, #30352, #20568, .T. ) ;
#17677 = CARTESIAN_POINT ( 'NONE',  ( -9.414213562409999625, -15.31419272936388687, -74.45223986426802298 ) ) ;
#17678 = VECTOR ( 'NONE', #24562, 1000.000000000000000 ) ;
#17679 = ORIENTED_EDGE ( 'NONE', *, *, #8467, .F. ) ;
#17680 = CARTESIAN_POINT ( 'NONE',  ( 3.511528848221511012, 0.9178490656560075456, 227.7210190899548365 ) ) ;
#17681 = CARTESIAN_POINT ( 'NONE',  ( -23.20948082139999968, -13.40000000000000036, 3.900000000369999942 ) ) ;
#17682 = FACE_BOUND ( 'NONE', #18741, .T. ) ;
#17683 = EDGE_CURVE ( 'NONE', #12643, #24389, #28280, .T. ) ;
#17684 = CARTESIAN_POINT ( 'NONE',  ( 23.74337837439999888, -14.46065164910000078, 224.0987030360000176 ) ) ;
#17685 = CARTESIAN_POINT ( 'NONE',  ( 17.16657240420000008, 10.97998838177520931, 0.5194763363741546902 ) ) ;
#17686 = PRODUCT_DEFINITION_SHAPE ( 'NONE', 'NONE',  #31120 ) ;
#17687 = CARTESIAN_POINT ( 'NONE',  ( 3.258358799905588299, -2.671990297561158467, -0.6999999999999992895 ) ) ;
#17688 = CARTESIAN_POINT ( 'NONE',  ( 14.60916111673911288, -28.04296597555454085, 0.7595836940000044724 ) ) ;
#17689 = CARTESIAN_POINT ( 'NONE',  ( 1.100000000000000089, -27.47799119300000115, 225.0000000000000000 ) ) ;
#17690 = ORIENTED_EDGE ( 'NONE', *, *, #23193, .F. ) ;
#17691 = DIRECTION ( 'NONE',  ( -0.7071067811865475727, -0.6644630243886071597, -0.2418447626481610435 ) ) ;
#17692 = CARTESIAN_POINT ( 'NONE',  ( 14.09657531829999932, 28.30410039250000054, 222.0000000000000000 ) ) ;
#17693 = CARTESIAN_POINT ( 'NONE',  ( -24.79654435811119484, -10.16723671460308154, 93.21714158839822062 ) ) ;
#17694 = CARTESIAN_POINT ( 'NONE',  ( 0.03549436706548679543, -27.80040766162893817, 6.002517553000020101 ) ) ;
#17695 = VECTOR ( 'NONE', #30143, 1000.000000000000000 ) ;
#17696 = VERTEX_POINT ( 'NONE', #7110 ) ;
#17697 = EDGE_CURVE ( 'NONE', #12916, #8976, #28352, .T. ) ;
#17698 = DIRECTION ( 'NONE',  ( 1.000000000000000000, -1.224606353820000075E-16, 0.000000000000000000 ) ) ;
#17699 = SURFACE_SIDE_STYLE ('',( #8260 ) ) ;
#17700 = LINE ( 'NONE', #6384, #4157 ) ;
#17701 = CARTESIAN_POINT ( 'NONE',  ( -8.699999999703425857, -29.80249410822303346, -29.47052640025896508 ) ) ;
#17702 = ADVANCED_FACE ( 'NONE', ( #11368, #2395 ), #6797, .F. ) ;
#17703 = AXIS2_PLACEMENT_3D ( 'NONE', #15970, #17997, #23216 ) ;
#17704 = CARTESIAN_POINT ( 'NONE',  ( 5.896017893897736784, 2.415859114112482775, -61.37141554682499134 ) ) ;
#17705 = ORIENTED_EDGE ( 'NONE', *, *, #25745, .T. ) ;
#17706 = ORIENTED_EDGE ( 'NONE', *, *, #10254, .F. ) ;
#17707 = CARTESIAN_POINT ( 'NONE',  ( 27.79539923781684507, 0.5057481689249165857, 0.8585786439999909536 ) ) ;
#17708 = ORIENTED_EDGE ( 'NONE', *, *, #14486, .T. ) ;
#17709 = PLANE ( 'NONE',  #19208 ) ;
#17710 = CARTESIAN_POINT ( 'NONE',  ( -12.29999999971541591, -30.00000000000000000, -28.79269908189872851 ) ) ;
#17711 = CARTESIAN_POINT ( 'NONE',  ( -25.22658730140000216, -13.26242337740000110, 225.0000014190000002 ) ) ;
#17712 = CARTESIAN_POINT ( 'NONE',  ( 8.700000000287717583, -16.96959321760160222, -37.81493174583334849 ) ) ;
#17713 = ADVANCED_FACE ( 'NONE', ( #21435 ), #30805, .T. ) ;
#17714 = CARTESIAN_POINT ( 'NONE',  ( 25.41286869299526074, -12.90211872965451079, 5.507123706999989210 ) ) ;
#17715 = DIRECTION ( 'NONE',  ( 0.000000000000000000, 0.000000000000000000, -1.000000000000000000 ) ) ;
#17716 = ORIENTED_EDGE ( 'NONE', *, *, #15827, .F. ) ;
#17717 = CARTESIAN_POINT ( 'NONE',  ( 1.728339646750869818, -3.757809983586919866, -44.10000000002499121 ) ) ;
#17718 = DIRECTION ( 'NONE',  ( 0.8660254037843289066, -0.5000000000001899592, 0.000000000000000000 ) ) ;
#17719 = ADVANCED_FACE ( 'NONE', ( #28195 ), #22753, .T. ) ;
#17720 = CARTESIAN_POINT ( 'NONE',  ( 5.195105410215491659, 3.969764343816663210, -23.36727430110000014 ) ) ;
#17721 = DIRECTION ( 'NONE',  ( 1.000000000000000000, -1.841917067661885521E-12, 2.653884470265303553E-12 ) ) ;
#17722 = AXIS2_PLACEMENT_3D ( 'NONE', #2627, #14015, #29203 ) ;
#17723 = FACE_OUTER_BOUND ( 'NONE', #13816, .T. ) ;
#17724 = CONICAL_SURFACE ( 'NONE', #25298, 4.987531172069999741, 1.047197551199999799 ) ;
#17725 = SURFACE_STYLE_USAGE ( .BOTH. , #8127 ) ;
#17726 = CARTESIAN_POINT ( 'NONE',  ( -24.93720648713954446, 13.79881813474513486, 6.099998581000020792 ) ) ;
#17727 = CARTESIAN_POINT ( 'NONE',  ( -3.917812474729757799, -3.807994372373406211, -46.40083066912499277 ) ) ;
#17728 = EDGE_CURVE ( 'NONE', #24389, #27584, #31029, .T. ) ;
#17729 = DIRECTION ( 'NONE',  ( 6.901835126637476841E-14, -5.775494631892377345E-13, 1.000000000000000000 ) ) ;
#17730 = CARTESIAN_POINT ( 'NONE',  ( 2.898287520843013443, -26.64792758275491380, 209.9518913731128009 ) ) ;
#17731 = CARTESIAN_POINT ( 'NONE',  ( -17.92761595767789728, 19.99992249444004244, 230.6995778483687616 ) ) ;
#17732 = DIRECTION ( 'NONE',  ( 0.6087614290090099800, 0.7933533402910131205, 4.134802762626407668E-12 ) ) ;
#17733 = CARTESIAN_POINT ( 'NONE',  ( 8.727399452413365566, -25.34090985533206108, 23.95427889024438173 ) ) ;
#17734 = VERTEX_POINT ( 'NONE', #23800 ) ;
#17735 = CARTESIAN_POINT ( 'NONE',  ( 4.556810990865948874, -1.030009251744163468, -33.28377053309998956 ) ) ;
#17736 = VERTEX_POINT ( 'NONE', #8998 ) ;
#17737 = DIRECTION ( 'NONE',  ( 4.250489863290715314E-14, 6.005940811918195789E-13, 1.000000000000000000 ) ) ;
#17738 = CARTESIAN_POINT ( 'NONE',  ( -3.745704904464692842, -4.048335345151853559, -50.99612412472499301 ) ) ;
#17739 = ORIENTED_EDGE ( 'NONE', *, *, #6910, .F. ) ;
#17740 = AXIS2_PLACEMENT_3D ( 'NONE', #29898, #8169, #3455 ) ;
#17741 = ORIENTED_EDGE ( 'NONE', *, *, #28936, .F. ) ;
#17742 = AXIS2_PLACEMENT_3D ( 'NONE', #20159, #15432, #10563 ) ;
#17743 = ORIENTED_EDGE ( 'NONE', *, *, #11278, .T. ) ;
#17744 = ORIENTED_EDGE ( 'NONE', *, *, #17338, .F. ) ;
#17745 = DIRECTION ( 'NONE',  ( -0.000000000000000000, 0.000000000000000000, -1.000000000000000000 ) ) ;
#17746 = FACE_OUTER_BOUND ( 'NONE', #1338, .T. ) ;
#17747 = CARTESIAN_POINT ( 'NONE',  ( 3.609060361128767713, 3.656617855560637231, -35.69999999999999574 ) ) ;
#17748 = CARTESIAN_POINT ( 'NONE',  ( 8.000000000289732682, -15.05691661385925961, -37.86814300156539304 ) ) ;
#17749 = DIRECTION ( 'NONE',  ( 0.000000000000000000, 0.3420201433259318358, -0.9396926207858125046 ) ) ;
#17750 = EDGE_CURVE ( 'NONE', #11379, #6771, #22797, .T. ) ;
#17751 = CARTESIAN_POINT ( 'NONE',  ( -3.935256165287342789, 0.8486244890569863975, -0.6999999999999994005 ) ) ;
#17752 = CARTESIAN_POINT ( 'NONE',  ( 3.956700543085260424, -2.628121156294163541, 1.041245269799995876 ) ) ;
#17753 = CARTESIAN_POINT ( 'NONE',  ( -3.221703195397895403, -1.419518900327898736, 227.6563758784881202 ) ) ;
#17754 = CARTESIAN_POINT ( 'NONE',  ( 8.699999999548097662, -14.92844969910509079, -33.25053330388070805 ) ) ;
#17755 = EDGE_CURVE ( 'NONE', #11678, #28642, #28806, .T. ) ;
#17756 = CARTESIAN_POINT ( 'NONE',  ( -1.184025259985572953, -4.532227402022651397, -12.55022317840000312 ) ) ;
#17757 = CARTESIAN_POINT ( 'NONE',  ( 2.070912548172440637, 4.356181786950492629, -31.21363063600000487 ) ) ;
#17758 = EDGE_CURVE ( 'NONE', #28953, #19872, #6174, .T. ) ;
#17759 = EDGE_CURVE ( 'NONE', #8329, #13375, #21593, .T. ) ;
#17760 = VECTOR ( 'NONE', #17396, 1000.000000000000114 ) ;
#17761 = CARTESIAN_POINT ( 'NONE',  ( -13.67718144140000014, 21.70000000000000284, -57.16242377749999548 ) ) ;
#17762 = CARTESIAN_POINT ( 'NONE',  ( -24.53666176017020462, -13.06964705028265072, 225.5585889358212626 ) ) ;
#17763 = CARTESIAN_POINT ( 'NONE',  ( 24.06826093652101051, -20.50742065841456707, 1.000000000000000888 ) ) ;
#17764 = VECTOR ( 'NONE', #24038, 1000.000000000000000 ) ;
#17765 = CARTESIAN_POINT ( 'NONE',  ( -27.04041630560000087, -6.115355784250000757E-14, 230.6999999999999886 ) ) ;
#17766 = CARTESIAN_POINT ( 'NONE',  ( -8.699999999733913469, -28.43737202012412624, -25.73763746937040864 ) ) ;
#17767 = VECTOR ( 'NONE', #2399, 1000.000000000000000 ) ;
#17768 = AXIS2_PLACEMENT_3D ( 'NONE', #25904, #6382, #15980 ) ;
#17769 =( GEOMETRIC_REPRESENTATION_CONTEXT ( 3 ) GLOBAL_UNCERTAINTY_ASSIGNED_CONTEXT ( ( #6240 ) ) GLOBAL_UNIT_ASSIGNED_CONTEXT ( ( #17142, #336, #5038 ) ) REPRESENTATION_CONTEXT ( 'NONE', 'WORKASPACE' ) );
#17770 = CARTESIAN_POINT ( 'NONE',  ( 17.16657240421717390, -9.000000000001264766, -0.6999999999999784173 ) ) ;
#17771 = CARTESIAN_POINT ( 'NONE',  ( 0.000000000000000000, 0.000000000000000000, 231.6412452697749984 ) ) ;
#17772 = CARTESIAN_POINT ( 'NONE',  ( 27.07818553041514065, 6.807801137122736712, 1.000000000000000888 ) ) ;
#17773 = ORIENTED_EDGE ( 'NONE', *, *, #28126, .F. ) ;
#17774 = DIRECTION ( 'NONE',  ( 0.000000000000000000, 0.000000000000000000, -1.000000000000000000 ) ) ;
#17775 = CARTESIAN_POINT ( 'NONE',  ( 10.24010329470000080, 19.99999999999999645, -1.477379946600000604 ) ) ;
#17776 = ORIENTED_EDGE ( 'NONE', *, *, #7485, .T. ) ;
#17777 = CARTESIAN_POINT ( 'NONE',  ( -16.04158851046123502, 10.23646161653652875, -0.6999999989999727834 ) ) ;
#17778 = CARTESIAN_POINT ( 'NONE',  ( 7.989499821578848859, -115.4538843872006453, 21.21004799597932688 ) ) ;
#17779 = ORIENTED_EDGE ( 'NONE', *, *, #21062, .F. ) ;
#17780 = CARTESIAN_POINT ( 'NONE',  ( -1.100000000000000089, -26.77741585740000119, 5.000000000000000000 ) ) ;
#17781 = VERTEX_POINT ( 'NONE', #18908 ) ;
#17782 = EDGE_LOOP ( 'NONE', ( #906, #13579, #1149, #25551 ) ) ;
#17783 =( LENGTH_UNIT ( ) NAMED_UNIT ( * ) SI_UNIT ( .MILLI., .METRE. ) );
#17784 = ORIENTED_EDGE ( 'NONE', *, *, #26739, .F. ) ;
#17785 = CARTESIAN_POINT ( 'NONE',  ( 27.56257419730000180, 4.654386182180000553, 230.5592437530000041 ) ) ;
#17786 = AXIS2_PLACEMENT_3D ( 'NONE', #26465, #358, #2699 ) ;
#17787 = EDGE_CURVE ( 'NONE', #2571, #17102, #17161, .T. ) ;
#17788 = CARTESIAN_POINT ( 'NONE',  ( -17.93324555128263142, -9.020011618190519442, -0.6999999999999784173 ) ) ;
#17790 = PLANE ( 'NONE',  #8518 ) ;
#17789 = CIRCLE ( 'NONE', #7735, 1.120011618224791450 ) ;
#17791 = CIRCLE ( 'NONE', #6757, 2.000000000000000000 ) ;
#17792 = EDGE_LOOP ( 'NONE', ( #12997, #1831, #26621, #12482 ) ) ;
#17793 = SURFACE_STYLE_USAGE ( .BOTH. , #30077 ) ;
#17794 = VECTOR ( 'NONE', #15814, 999.9999999999998863 ) ;
#17795 = CARTESIAN_POINT ( 'NONE',  ( -0.4969045691271392617, -28.49594262166942116, 5.506468674000009500 ) ) ;
#17796 = CARTESIAN_POINT ( 'NONE',  ( 6.965151789112639769, -26.60412671351617320, 208.3894876551769926 ) ) ;
#17797 = CARTESIAN_POINT ( 'NONE',  ( -19.29999999990000248, -28.92682926916000241, -28.39999999989999679 ) ) ;
#17798 = CARTESIAN_POINT ( 'NONE',  ( -6.055223678858003389, -2.441925613954294860, -1.597197434499999957 ) ) ;
#17799 = CARTESIAN_POINT ( 'NONE',  ( -2.618143654921853969, 3.481518582925489991, -19.13064294430000345 ) ) ;
#17800 = LINE ( 'NONE', #8052, #15848 ) ;
#17801 = CARTESIAN_POINT ( 'NONE',  ( -1.071537510008835126, -27.47917025540911951, 5.286989672262158102 ) ) ;
#17802 = STYLED_ITEM ( 'NONE', ( #12960 ), #26089 ) ;
#17803 = CARTESIAN_POINT ( 'NONE',  ( 24.68173674080000168, -14.25001227039999918, 223.9000014189999774 ) ) ;
#17804 = FACE_OUTER_BOUND ( 'NONE', #26075, .T. ) ;
#17805 = CARTESIAN_POINT ( 'NONE',  ( 8.000000000252409649, -24.26136093482662304, -29.62468611105709471 ) ) ;
#17806 = CARTESIAN_POINT ( 'NONE',  ( 0.5057536231481327693, -27.79562098839016571, 3.899998581000013509 ) ) ;
#17807 = CARTESIAN_POINT ( 'NONE',  ( -19.80526803560000104, 19.50877411510000314, 227.8000000000000114 ) ) ;
#17808 = CARTESIAN_POINT ( 'NONE',  ( -9.999999999909999104, 19.99999999999999645, -2.399999999999999467 ) ) ;
#17809 = VECTOR ( 'NONE', #28813, 1000.000000000000000 ) ;
#17810 = ORIENTED_EDGE ( 'NONE', *, *, #14607, .T. ) ;
#17811 = CARTESIAN_POINT ( 'NONE',  ( 4.332295931058598448, 4.388630459628991787, -57.22805965152500107 ) ) ;
#17812 = CARTESIAN_POINT ( 'NONE',  ( -8.000000000000000000, -15.18061163548115466, -76.53197586718597734 ) ) ;
#17813 = AXIS2_PLACEMENT_3D ( 'NONE', #6093, #13172, #19958 ) ;
#17814 = CARTESIAN_POINT ( 'NONE',  ( 4.315341029122434335, -4.279276102762477940, -15.06112212870000455 ) ) ;
#17815 = EDGE_LOOP ( 'NONE', ( #14958, #27240, #16329, #26476 ) ) ;
#17816 = B_SPLINE_CURVE_WITH_KNOTS ( 'NONE', 3,
 ( #5635, #10835, #24842, #10212, #19959, #20421, #930, #29554, #30014, #8449 ),
 .UNSPECIFIED., .F., .F.,
 ( 4, 2, 2, 2, 4 ),
 ( 0.000000000000000000, 0.2500000000000000000, 0.5000000000000000000, 0.7500000000000000000, 1.000000000000000000 ),
 .UNSPECIFIED. ) ;
#17817 = CARTESIAN_POINT ( 'NONE',  ( -26.67548192793729456, 9.015773298006253711, 0.2686740810000365354 ) ) ;
#17818 = CARTESIAN_POINT ( 'NONE',  ( -4.225732272487059404, 0.7470832582109949715, -68.10000000002500542 ) ) ;
#17819 = EDGE_CURVE ( 'NONE', #24853, #1904, #9308, .T. ) ;
#17820 = ORIENTED_EDGE ( 'NONE', *, *, #25640, .F. ) ;
#17821 = ORIENTED_EDGE ( 'NONE', *, *, #1863, .F. ) ;
#17822 = CARTESIAN_POINT ( 'NONE',  ( 2.383853413490760964, -1.270093451928029582, -97.49610867634444844 ) ) ;
#17823 =( NAMED_UNIT ( * ) PLANE_ANGLE_UNIT ( ) SI_UNIT ( $, .RADIAN. ) );
#17824 = ORIENTED_EDGE ( 'NONE', *, *, #15730, .F. ) ;
#17825 = CARTESIAN_POINT ( 'NONE',  ( -24.90302310912370132, 13.86047864606265279, 3.901342110999989288 ) ) ;
#17826 = VECTOR ( 'NONE', #14419, 1000.000000000000000 ) ;
#17827 = PRESENTATION_LAYER_ASSIGNMENT (  '', '', ( #278 ) ) ;
#17828 = CARTESIAN_POINT ( 'NONE',  ( 0.000000000000000000, -31.83942647549183746, -80.46693306215520636 ) ) ;
#17829 = CARTESIAN_POINT ( 'NONE',  ( 0.8372177269581373427, 4.490875019823951320, -63.02744533512500169 ) ) ;
#17830 = EDGE_CURVE ( 'NONE', #6392, #13541, #10823, .T. ) ;
#17831 = LINE ( 'NONE', #1166, #16933 ) ;
#17832 = CARTESIAN_POINT ( 'NONE',  ( 16.06941601963802668, 10.83371123183088436, 0.000000000000000000 ) ) ;
#17833 = CARTESIAN_POINT ( 'NONE',  ( -10.00000000000000000, -130.0000000000000000, -42.39999999999999858 ) ) ;
#17834 = CARTESIAN_POINT ( 'NONE',  ( -10.00000000070000183, -82.23832021890000021, -29.25398675769999812 ) ) ;
#17835 = ORIENTED_EDGE ( 'NONE', *, *, #10504, .F. ) ;
#17836 = PRODUCT_DEFINITION_CONTEXT ( 'detailed design', #24645, 'design' ) ;
#17837 = DIRECTION ( 'NONE',  ( -1.000000000000000000, 0.000000000000000000, 0.000000000000000000 ) ) ;
#17838 = CARTESIAN_POINT ( 'NONE',  ( -27.23548387100000312, 1.421085471519999843E-14, 91.66046017469999185 ) ) ;
#17839 = ORIENTED_EDGE ( 'NONE', *, *, #1764, .F. ) ;
#17840 = CARTESIAN_POINT ( 'NONE',  ( 24.55535052759999814, -13.03386662210000146, 224.4930265309999982 ) ) ;
#17841 = CARTESIAN_POINT ( 'NONE',  ( -24.00926694310947695, -14.01467022312833421, 6.042472825000033687 ) ) ;
#17842 = CARTESIAN_POINT ( 'NONE',  ( -23.62421573606080827, -14.65442406347138338, 6.042470790000031400 ) ) ;
#17843 = CARTESIAN_POINT ( 'NONE',  ( 26.00441062110688506, 9.413902731553067227, 0.02487529700001545052 ) ) ;
#17844 = CARTESIAN_POINT ( 'NONE',  ( 1.030019577584204020E-10, -102.7755780389355778, 17.20706796825876239 ) ) ;
#17845 = CARTESIAN_POINT ( 'NONE',  ( 3.233307954802753237, -2.689733879864655286, -0.6999999999999992895 ) ) ;
#17846 = CARTESIAN_POINT ( 'NONE',  ( -15.73360964098195147, -8.979988381493612337, 0.000000000000000000 ) ) ;
#17847 = CARTESIAN_POINT ( 'NONE',  ( 27.92857142820000149, 7.105427357599999217E-15, 142.0603150149999863 ) ) ;
#17848 = AXIS2_PLACEMENT_3D ( 'NONE', #2982, #29718, #9912 ) ;
#17849 = ORIENTED_EDGE ( 'NONE', *, *, #6964, .T. ) ;
#17850 = ADVANCED_FACE ( 'NONE', ( #22364 ), #3676, .T. ) ;
#17851 = DIRECTION ( 'NONE',  ( 0.000000000000000000, 0.000000000000000000, -1.000000000000000000 ) ) ;
#17852 = CARTESIAN_POINT ( 'NONE',  ( -25.15951549259923326, -9.235088186050580461, 93.21714158838125286 ) ) ;
#17853 = CARTESIAN_POINT ( 'NONE',  ( 18.82264457159015691, 10.97998838177520931, -1.452769935612311825 ) ) ;
#17854 = CARTESIAN_POINT ( 'NONE',  ( -9.631980347289379907, 21.69999999997851603, -53.61980015864676119 ) ) ;
#17855 = SURFACE_STYLE_USAGE ( .BOTH. , #17699 ) ;
#17856 = CARTESIAN_POINT ( 'NONE',  ( 14.74203063448154793, -25.68810651402014500, -33.41580572993174059 ) ) ;
#17857 = CARTESIAN_POINT ( 'NONE',  ( -26.85555875125346859, -1.316834860305418076, -0.6999999999999992895 ) ) ;
#17858 = CARTESIAN_POINT ( 'NONE',  ( -0.8249440165340113928, 4.504533947698903695, -60.25324387862499975 ) ) ;
#17859 = ORIENTED_EDGE ( 'NONE', *, *, #4208, .F. ) ;
#17860 = ADVANCED_FACE ( 'NONE', ( #17014 ), #17471, .T. ) ;
#17861 = CARTESIAN_POINT ( 'NONE',  ( 18.66381637565261542, 19.99999441337020656, 230.6065604230005874 ) ) ;
#17862 = VERTEX_POINT ( 'NONE', #17619 ) ;
#17863 = CARTESIAN_POINT ( 'NONE',  ( 8.699999999531884853, -22.83323352251082738, -39.84673050073825351 ) ) ;
#17864 = VERTEX_POINT ( 'NONE', #26929 ) ;
#17865 = DIRECTION ( 'NONE',  ( 1.000000000000000000, 0.000000000000000000, 0.000000000000000000 ) ) ;
#17866 = DIRECTION ( 'NONE',  ( -1.000000000000000000, 0.000000000000000000, 0.000000000000000000 ) ) ;
#17867 = DIRECTION ( 'NONE',  ( 1.553791817432425509E-12, 0.7253743710120286181, -0.6883545756940269156 ) ) ;
#17868 = B_SPLINE_CURVE_WITH_KNOTS ( 'NONE', 3,
 ( #22319, #154, #12560, #28935, #14625, #9896 ),
 .UNSPECIFIED., .F., .F.,
 ( 4, 2, 4 ),
 ( 0.000000000000000000, 0.5000000000000000000, 1.000000000000000000 ),
 .UNSPECIFIED. ) ;
#17869 = CARTESIAN_POINT ( 'NONE',  ( -17.49227491161553871, -24.88129198361984606, -32.95026604850808383 ) ) ;
#17870 = CARTESIAN_POINT ( 'NONE',  ( 25.25401215828319579, -13.21081861402798374, 5.901400366999986602 ) ) ;
#17871 = CARTESIAN_POINT ( 'NONE',  ( -1.100001419170000050, -27.77850706310000106, 224.8959436220000043 ) ) ;
#17872 = EDGE_LOOP ( 'NONE', ( #9393, #20270 ) ) ;
#17873 = CARTESIAN_POINT ( 'NONE',  ( -2.098672137722010334, -3.287437779826620776, -44.10000000002499121 ) ) ;
#17874 = EDGE_CURVE ( 'NONE', #19357, #30733, #3004, .T. ) ;
#17875 = CARTESIAN_POINT ( 'NONE',  ( 26.80000000000000071, -6.394884621839999216E-14, 230.6999999999999886 ) ) ;
#17876 = EDGE_CURVE ( 'NONE', #28481, #24422, #12596, .T. ) ;
#17877 = CARTESIAN_POINT ( 'NONE',  ( 4.275653884846098762, -3.504702130532165505, -24.99674734060000603 ) ) ;
#17878 = CARTESIAN_POINT ( 'NONE',  ( 27.79539923611798358, 0.5057481688468927761, 8.000000000000007105 ) ) ;
#17879 = CARTESIAN_POINT ( 'NONE',  ( 19.80538173989999962, 19.50875420239999869, 227.3999999149999951 ) ) ;
#17880 = CARTESIAN_POINT ( 'NONE',  ( -10.00000000001209344, -15.94902145808038618, -35.53273252466679111 ) ) ;
#17881 = DIRECTION ( 'NONE',  ( 0.000000000000000000, 0.000000000000000000, 1.000000000000000000 ) ) ;
#17882 = CARTESIAN_POINT ( 'NONE',  ( -5.843148694310191793, 0.5835664591014033675, -46.82737393802500492 ) ) ;
#17883 = EDGE_CURVE ( 'NONE', #26472, #11411, #2898, .T. ) ;
#17884 = CARTESIAN_POINT ( 'NONE',  ( 10.88909890409999903, 20.99999999999999645, -56.10000000020000499 ) ) ;
#17885 = CARTESIAN_POINT ( 'NONE',  ( 5.852082250035302913, -26.15431190117149285, 208.9630145448510916 ) ) ;
#17886 = CARTESIAN_POINT ( 'NONE',  ( -19.83759560044297388, 20.00030161953416297, 230.0085100852693358 ) ) ;
#17887 = CARTESIAN_POINT ( 'NONE',  ( -25.51870711004139380, -8.199261060474283269, 43.21714158836665831 ) ) ;
#17888 = CARTESIAN_POINT ( 'NONE',  ( 4.671347416477003023, -26.39088508839783032, 20.48731328533980545 ) ) ;
#17889 = ORIENTED_EDGE ( 'NONE', *, *, #5663, .F. ) ;
#17890 = CARTESIAN_POINT ( 'NONE',  ( -4.339197174995634398, 0.6278332542688190854, -34.75783976330000513 ) ) ;
#17891 = EDGE_CURVE ( 'NONE', #12916, #2248, #15225, .T. ) ;
#17892 = ORIENTED_EDGE ( 'NONE', *, *, #2380, .T. ) ;
#17893 = CARTESIAN_POINT ( 'NONE',  ( 0.000000000000000000, 0.000000000000000000, 115.0000000000000000 ) ) ;
#17894 = CARTESIAN_POINT ( 'NONE',  ( 4.762123832160154890, 2.112064333128992555, -52.62998794302499306 ) ) ;
#17895 = ORIENTED_EDGE ( 'NONE', *, *, #3075, .T. ) ;
#17896 = VERTEX_POINT ( 'NONE', #24716 ) ;
#17897 = SHAPE_DEFINITION_REPRESENTATION ( #27648, #28252 ) ;
#17898 = B_SPLINE_CURVE_WITH_KNOTS ( 'NONE', 3,
 ( #12786, #27108, #10124, #10730, #10431, #29620, #29303, #19879, #15147, #17351 ),
 .UNSPECIFIED., .F., .F.,
 ( 4, 2, 2, 2, 4 ),
 ( 0.000000000000000000, 0.2500000000000000000, 0.5000000000000000000, 0.7500000000000000000, 1.000000000000000000 ),
 .UNSPECIFIED. ) ;
#17899 = EDGE_LOOP ( 'NONE', ( #9795, #25897, #10222, #2029, #14484, #15, #25443, #14019, #31114, #16989, #19292, #11500, #7886, #10564, #1238, #28326, #247 ) ) ;
#17900 = VERTEX_POINT ( 'NONE', #14666 ) ;
#17901 = CARTESIAN_POINT ( 'NONE',  ( 24.61381495443087175, 14.36755986787189521, 3.957524335000017768 ) ) ;
#17902 = EDGE_CURVE ( 'NONE', #25445, #10257, #9201, .T. ) ;
#17903 = CARTESIAN_POINT ( 'NONE',  ( 26.80000000069999899, -3.214342854470000215E-14, 230.0000000000000000 ) ) ;
#17904 = CARTESIAN_POINT ( 'NONE',  ( -10.69999999999999929, -27.00000000000000000, -28.40000000000000213 ) ) ;
#17905 = CARTESIAN_POINT ( 'NONE',  ( 9.000000000029999114, 20.99999999999999645, -45.10000000000000142 ) ) ;
#17906 = DIRECTION ( 'NONE',  ( 0.7071067811865476838, -1.595945597898661315E-12, -0.7071067811865473507 ) ) ;
#17907 = CARTESIAN_POINT ( 'NONE',  ( -3.928330961999677573, 0.9358211253549650888, -0.6999999999999992895 ) ) ;
#17908 = CARTESIAN_POINT ( 'NONE',  ( 1.213582369797461258, 4.521795443253901148, -2.053410702900000828 ) ) ;
#17909 = CARTESIAN_POINT ( 'NONE',  ( 10.69999999997517115, -27.39379052061039843, -31.39999999999999858 ) ) ;
#17910 = CARTESIAN_POINT ( 'NONE',  ( 8.000000000287716517, -16.96959321760095563, -37.81493174583665251 ) ) ;
#17911 = CARTESIAN_POINT ( 'NONE',  ( 1.708629737455300335, 5.223905898740939691, -12.07047964829999920 ) ) ;
#17912 = CARTESIAN_POINT ( 'NONE',  ( 0.07512830594656044747, -4.346272141329931671, -33.41110030499999795 ) ) ;
#17913 = FACE_OUTER_BOUND ( 'NONE', #11961, .T. ) ;
#17914 = FACE_OUTER_BOUND ( 'NONE', #16707, .T. ) ;
#17915 = CARTESIAN_POINT ( 'NONE',  ( -28.35945636591989683, -7.983396444576476902, 1.000000000000000888 ) ) ;
#17916 = CARTESIAN_POINT ( 'NONE',  ( 14.85000000009999788, -27.00000000000000000, -28.39999999989999679 ) ) ;
#17917 = CARTESIAN_POINT ( 'NONE',  ( 4.370697773661016861, 1.580342671372844787, -26.51249766020000109 ) ) ;
#17918 = CARTESIAN_POINT ( 'NONE',  ( 18.34691755833856064, 20.56908522341882417, -0.5592437529999827461 ) ) ;
#17919 = PLANE ( 'NONE',  #24300 ) ;
#17920 = CARTESIAN_POINT ( 'NONE',  ( -6.661312627754256255, -8.560122214784900763, -36.64192442629084212 ) ) ;
#17921 = ORIENTED_EDGE ( 'NONE', *, *, #17330, .F. ) ;
#17922 = CARTESIAN_POINT ( 'NONE',  ( -7.999999999720831312, -24.33763747047824566, -26.96262797785872678 ) ) ;
#17923 = CARTESIAN_POINT ( 'NONE',  ( 10.00000000020000002, 19.99999999999999645, -2.208382156699995047 ) ) ;
#17924 = ORIENTED_EDGE ( 'NONE', *, *, #5994, .F. ) ;
#17925 = CIRCLE ( 'NONE', #8384, 4.987531172950001590 ) ;
#17926 = CARTESIAN_POINT ( 'NONE',  ( -1.022169856860690729, -3.500000000000000444, 227.7302799852759279 ) ) ;
#17927 = DIRECTION ( 'NONE',  ( -0.000000000000000000, 0.000000000000000000, -1.000000000000000000 ) ) ;
#17928 = EDGE_CURVE ( 'NONE', #18728, #17781, #693, .T. ) ;
#17929 = ORIENTED_EDGE ( 'NONE', *, *, #30863, .F. ) ;
#17930 = CARTESIAN_POINT ( 'NONE',  ( -1.099927927653325810, -26.77741881808574220, 4.854121423575340266 ) ) ;
#17931 = ORIENTED_EDGE ( 'NONE', *, *, #18352, .T. ) ;
#17932 = VERTEX_POINT ( 'NONE', #24107 ) ;
#17933 = ADVANCED_FACE ( 'NONE', ( #24250 ), #2697, .F. ) ;
#17934 =( NAMED_UNIT ( * ) SI_UNIT ( $, .STERADIAN. ) SOLID_ANGLE_UNIT ( ) );
#17935 = ORIENTED_EDGE ( 'NONE', *, *, #22699, .F. ) ;
#17936 = CARTESIAN_POINT ( 'NONE',  ( -17.36983091266188950, 10.02891580965362017, -0.6999999999999784173 ) ) ;
#17937 = ADVANCED_FACE ( 'NONE', ( #8167 ), #2849, .F. ) ;
#17938 = DIRECTION ( 'NONE',  ( -1.000000000000000000, -1.433034374054745923E-13, -1.199006074477166028E-12 ) ) ;
#17939 = DIRECTION ( 'NONE',  ( -0.000000000000000000, 0.000000000000000000, -1.000000000000000000 ) ) ;
#17940 = ORIENTED_EDGE ( 'NONE', *, *, #29494, .T. ) ;
#17941 = CARTESIAN_POINT ( 'NONE',  ( -17.62526668112344908, -8.236461616547455122, -0.6999999989999727834 ) ) ;
#17942 = CARTESIAN_POINT ( 'NONE',  ( -0.6094664100040195764, -28.49364619262437870, 5.104049977999985721 ) ) ;
#17943 = CONICAL_SURFACE ( 'NONE', #28526, 0.9999999999991042721, 0.7853981633970000820 ) ;
#17944 = CARTESIAN_POINT ( 'NONE',  ( -6.999999999262594308, -5.572998883415898774, -27.02754848611273530 ) ) ;
#17945 = CARTESIAN_POINT ( 'NONE',  ( -11.26179938759879740, 26.42151601322855115, -59.26168417594740845 ) ) ;
#17946 = TOROIDAL_SURFACE ( 'NONE', #30536, 29.80000000000000071, 3.000000000000000000 ) ;
#17947 = CARTESIAN_POINT ( 'NONE',  ( 0.5877407897813119453, -4.297347728519514298, -0.8731240480000050930 ) ) ;
#17948 = CARTESIAN_POINT ( 'NONE',  ( -3.679974273075529823, -2.251605409995534490, -21.90799200640000777 ) ) ;
#17949 = CARTESIAN_POINT ( 'NONE',  ( -0.6817539855342577004, -28.49230123151905758, 224.1111716133609093 ) ) ;
#17950 = AXIS2_PLACEMENT_3D ( 'NONE', #8414, #10337, #27620 ) ;
#17951 = CARTESIAN_POINT ( 'NONE',  ( 4.638687372303287759, 5.146895567816208938, -43.32728369091725540 ) ) ;
#17952 = CARTESIAN_POINT ( 'NONE',  ( 24.87112161019999945, -13.91739822849999975, 223.9575271749999672 ) ) ;
#17953 = CARTESIAN_POINT ( 'NONE',  ( -21.81164872309999936, 17.47864169270000190, 230.5592437530000041 ) ) ;
#17954 = CARTESIAN_POINT ( 'NONE',  ( -1.243449787579999883E-14, 0.000000000000000000, -0.6999999999999992895 ) ) ;
#17955 = CARTESIAN_POINT ( 'NONE',  ( -8.000000000474178918, -29.73863906514523947, -27.17531388891475075 ) ) ;
#17956 = DIRECTION ( 'NONE',  ( 0.000000000000000000, 0.000000000000000000, 1.000000000000000000 ) ) ;
#17957 = CARTESIAN_POINT ( 'NONE',  ( 10.87630772340000185, -14.78838862870000170, 230.6999999999999886 ) ) ;
#17958 = CARTESIAN_POINT ( 'NONE',  ( 23.25354871338156570, -14.68148953523539468, 224.7820750499900839 ) ) ;
#17959 = ORIENTED_EDGE ( 'NONE', *, *, #11422, .T. ) ;
#17960 = CARTESIAN_POINT ( 'NONE',  ( 4.332295931058598448, 4.388630459628991787, -57.70805965152499795 ) ) ;
#17961 = DIRECTION ( 'NONE',  ( 1.000000000000000000, -3.980999999999999294E-12, 1.940999999999999504E-12 ) ) ;
#17962 = ORIENTED_EDGE ( 'NONE', *, *, #25713, .F. ) ;
#17963 = CIRCLE ( 'NONE', #16997, 3.500000000000000888 ) ;
#17964 = CARTESIAN_POINT ( 'NONE',  ( 6.086077541567210147, 0.7980478301550381071, -5.626979598400000171 ) ) ;
#17965 = ORIENTED_EDGE ( 'NONE', *, *, #13617, .T. ) ;
#17966 = DIRECTION ( 'NONE',  ( -5.962915006522622422E-16, -0.4383711467890810676, -0.8987940462991651502 ) ) ;
#17967 = VECTOR ( 'NONE', #30899, 1000.000000000000000 ) ;
#17968 = DIRECTION ( 'NONE',  ( 5.962915006522623408E-16, 0.4383711467890811231, 0.8987940462991652613 ) ) ;
#17969 = ORIENTED_EDGE ( 'NONE', *, *, #29110, .F. ) ;
#17970 = ORIENTED_EDGE ( 'NONE', *, *, #18429, .T. ) ;
#17971 = ORIENTED_EDGE ( 'NONE', *, *, #8527, .F. ) ;
#17972 = AXIS2_PLACEMENT_3D ( 'NONE', #14840, #14526, #7125 ) ;
#17973 = CARTESIAN_POINT ( 'NONE',  ( 3.043095095518108195, -3.198806979844766474, -95.69213427724059784 ) ) ;
#17974 =( LENGTH_UNIT ( ) NAMED_UNIT ( * ) SI_UNIT ( .MILLI., .METRE. ) );
#17975 = ORIENTED_EDGE ( 'NONE', *, *, #25218, .F. ) ;
#17976 = CARTESIAN_POINT ( 'NONE',  ( -24.52721838136531574, 14.51532614515681097, 4.239732039000021047 ) ) ;
#17977 = AXIS2_PLACEMENT_3D ( 'NONE', #6676, #9038, #21471 ) ;
#17978 = EDGE_CURVE ( 'NONE', #22441, #18380, #26928, .T. ) ;
#17979 = CARTESIAN_POINT ( 'NONE',  ( -8.699999999630685821, -15.59624655979752461, -40.60108361767771612 ) ) ;
#17980 = CARTESIAN_POINT ( 'NONE',  ( -1.219854050253890598, 4.750520449216602437, -66.20876360982499875 ) ) ;
#17981 = CARTESIAN_POINT ( 'NONE',  ( 0.6657531355379500138, -28.49283337230381008, 6.099998581000005693 ) ) ;
#17982 = CARTESIAN_POINT ( 'NONE',  ( -27.37939150969657121, 4.212099059672701706, -0.6577119969999878357 ) ) ;
#17983 = CARTESIAN_POINT ( 'NONE',  ( 9.150827312880000619, 19.99999999999999645, -44.09999999970998630 ) ) ;
#17984 = CARTESIAN_POINT ( 'NONE',  ( -23.70259205116592227, -12.50815390717660058, 5.420582064722430538 ) ) ;
#17985 = FACE_OUTER_BOUND ( 'NONE', #611, .T. ) ;
#17986 = AXIS2_PLACEMENT_3D ( 'NONE', #684, #10276, #5538 ) ;
#17987 = ORIENTED_EDGE ( 'NONE', *, *, #26458, .F. ) ;
#17988 = CARTESIAN_POINT ( 'NONE',  ( 5.067327387632984959, 4.072231104569050686, -8.354586407999999409 ) ) ;
#17989 = CARTESIAN_POINT ( 'NONE',  ( 24.37821946547973084, -14.76389286113969490, 4.791564337000009388 ) ) ;
#17990 = CARTESIAN_POINT ( 'NONE',  ( 19.76610007289999871, 19.51851078889999869, 229.2246588520000046 ) ) ;
#17991 = VERTEX_POINT ( 'NONE', #1583 ) ;
#17992 = CARTESIAN_POINT ( 'NONE',  ( 24.60666743799999878, -12.93650359530000138, 225.0000014190000002 ) ) ;
#17993 = DIRECTION ( 'NONE',  ( -0.7071067811865475727, 0.7071067811865475727, 0.000000000000000000 ) ) ;
#17994 = CYLINDRICAL_SURFACE ( 'NONE', #21343, 2.000000000000004441 ) ;
#17995 = CARTESIAN_POINT ( 'NONE',  ( 18.50495734115402513, 20.74627095469091742, 0.9999999989999952543 ) ) ;
#17996 = FACE_OUTER_BOUND ( 'NONE', #24588, .T. ) ;
#17997 = DIRECTION ( 'NONE',  ( -1.000000000000000000, 0.000000000000000000, -0.000000000000000000 ) ) ;
#17998 = VECTOR ( 'NONE', #2500, 1000.000000000000000 ) ;
#17999 = B_SPLINE_CURVE_WITH_KNOTS ( 'NONE', 4,
 ( #11098, #22903, #24791, #15648, #6051 ),
 .UNSPECIFIED., .F., .F.,
 ( 5, 5 ),
 ( -0.9817477042459999970, 0.9817477042459999970 ),
 .UNSPECIFIED. ) ;
#18000 = DIRECTION ( 'NONE',  ( -0.000000000000000000, -0.000000000000000000, -1.000000000000000000 ) ) ;
#18001 = DIRECTION ( 'NONE',  ( 0.3633921898465276024, -0.9316362575375355393, -1.301042606982605321E-14 ) ) ;
#18002 = VERTEX_POINT ( 'NONE', #8802 ) ;
#18003 = CARTESIAN_POINT ( 'NONE',  ( 2.633098176678708328E-10, -9.034299563938168021, -24.71289265967806514 ) ) ;
#18004 = CARTESIAN_POINT ( 'NONE',  ( -8.700000000030557956, -116.5561065468281186, 18.74526241736806043 ) ) ;
#18005 = ADVANCED_FACE ( 'NONE', ( #18078 ), #1268, .F. ) ;
#18006 =( REPRESENTATION_RELATIONSHIP ('NONE','NONE', #2712, #527 ) REPRESENTATION_RELATIONSHIP_WITH_TRANSFORMATION ( #11614 )SHAPE_REPRESENTATION_RELATIONSHIP( ) );
#18007 = CYLINDRICAL_SURFACE ( 'NONE', #1785, 26.80000000000002203 ) ;
#18008 = TOROIDAL_SURFACE ( 'NONE', #30092, 29.80000000000000071, 3.000000000000000000 ) ;
#18009 = CARTESIAN_POINT ( 'NONE',  ( -10.00045772538970290, 21.69999999997727613, -54.17149754567696363 ) ) ;
#18010 = CARTESIAN_POINT ( 'NONE',  ( -23.81569860410000317, -13.75000000000000000, 226.0999999999999943 ) ) ;
#18011 =( LENGTH_UNIT ( ) NAMED_UNIT ( * ) SI_UNIT ( .MILLI., .METRE. ) );
#18012 = CARTESIAN_POINT ( 'NONE',  ( 14.63279312439965274, -26.20928159737690066, -33.71653667584794078 ) ) ;
#18013 = CARTESIAN_POINT ( 'NONE',  ( -10.89131017139999891, -24.73114799890000270, -1.811764705899998606 ) ) ;
#18014 = CARTESIAN_POINT ( 'NONE',  ( -5.941465883516308999, 0.03012783874251079297, -62.57122063482501062 ) ) ;
#18015 = ORIENTED_EDGE ( 'NONE', *, *, #30993, .F. ) ;
#18016 = CARTESIAN_POINT ( 'NONE',  ( -8.999999999710000864, 19.99999999959999641, -43.74999999991700150 ) ) ;
#18017 = ORIENTED_EDGE ( 'NONE', *, *, #26073, .T. ) ;
#18019 = CARTESIAN_POINT ( 'NONE',  ( 23.45614981985238146, -19.98580328777019943, 0.7069253189999902265 ) ) ;
#18018 = CIRCLE ( 'NONE', #4484, 4.000000004070001225 ) ;
#18020 = VERTEX_POINT ( 'NONE', #12909 ) ;
#18021 = CARTESIAN_POINT ( 'NONE',  ( -10.70170550458792569, 21.69999999997569162, -54.87247492467220411 ) ) ;
#18022 = DIRECTION ( 'NONE',  ( -5.551115123049999208E-18, 0.000000000000000000, -1.000000000000000000 ) ) ;
#18023 = CARTESIAN_POINT ( 'NONE',  ( -27.05781272067678600, 9.945516928293280046, 8.000000000000007105 ) ) ;
#18024 = B_SPLINE_CURVE_WITH_KNOTS ( 'NONE', 3,
 ( #23074, #8734, #6221, #27616, #4179, #8570, #13776, #1827, #8411, #18010 ),
 .UNSPECIFIED., .F., .F.,
 ( 4, 2, 2, 2, 4 ),
 ( 0.000000000000000000, 0.2500000000000000000, 0.5000000000000000000, 0.7500000000000000000, 1.000000000000000000 ),
 .UNSPECIFIED. ) ;
#18025 = CARTESIAN_POINT ( 'NONE',  ( 18.24482546714449072, 10.73903380414593478, -1.400000000000001910 ) ) ;
#18026 = CARTESIAN_POINT ( 'NONE',  ( 7.738200612013472757, -15.86465192213300845, -74.65259062561435144 ) ) ;
#18027 = CARTESIAN_POINT ( 'NONE',  ( -9.897162125286943279, -25.37356426548037547, 138.3395398250000028 ) ) ;
#18028 = VERTEX_POINT ( 'NONE', #13530 ) ;
#18029 = CARTESIAN_POINT ( 'NONE',  ( 0.1566502184896971517, -3.976918879132022688, -44.10000000002499121 ) ) ;
#18030 = CARTESIAN_POINT ( 'NONE',  ( 28.50000000000000000, 1.065814103639999922E-14, 229.0000000000000000 ) ) ;
#18031 = CARTESIAN_POINT ( 'NONE',  ( 9.999999999959999997, -29.30501631460000311, -26.47986984960000001 ) ) ;
#18032 = ADVANCED_FACE ( 'NONE', ( #10555 ), #24464, .F. ) ;
#18033 = AXIS2_PLACEMENT_3D ( 'NONE', #29153, #21774, #4934 ) ;
#18034 = CARTESIAN_POINT ( 'NONE',  ( -3.185244259044060389, 1.482995108822391161, 230.8358029176239938 ) ) ;
#18035 = DIRECTION ( 'NONE',  ( -2.966427579999808118E-12, -0.8902635789278700029, 0.4554456718803465698 ) ) ;
#18036 = DIRECTION ( 'NONE',  ( 1.000000000000000000, -1.843431230204166689E-12, 2.650498504954120002E-12 ) ) ;
#18037 = DIRECTION ( 'NONE',  ( -0.9316362575375349842, 0.3633921898465292122, -0.000000000000000000 ) ) ;
#18038 = DIRECTION ( 'NONE',  ( 0.000000000000000000, 0.000000000000000000, 1.000000000000000000 ) ) ;
#18039 = CARTESIAN_POINT ( 'NONE',  ( 4.421972129926212247, 1.961202595004083005, -51.87998794302499306 ) ) ;
#18040 = EDGE_CURVE ( 'NONE', #9370, #26977, #9586, .T. ) ;
#18041 = VECTOR ( 'NONE', #26982, 1000.000000000000000 ) ;
#18042 = CARTESIAN_POINT ( 'NONE',  ( -17.79876841479999783, 11.52736809289999620, -1.399999999999998579 ) ) ;
#18043 = CARTESIAN_POINT ( 'NONE',  ( 15.51050023680984680, 10.97998838177520931, 0.05106179917585291356 ) ) ;
#18044 = CARTESIAN_POINT ( 'NONE',  ( 14.66141101274631353, -27.86484103574591131, -33.67412216602015462 ) ) ;
#18045 = CARTESIAN_POINT ( 'NONE',  ( -19.81582138730395926, -18.05844329259049985, 43.21714158843889919 ) ) ;
#18046 = LINE ( 'NONE', #6094, #4714 ) ;
#18047 = ORIENTED_EDGE ( 'NONE', *, *, #5761, .T. ) ;
#18048 = CARTESIAN_POINT ( 'NONE',  ( -1.932773295258156887, 4.259541830411037289, -31.72635571290000200 ) ) ;
#18049 = EDGE_LOOP ( 'NONE', ( #1621, #10456, #29640, #15788 ) ) ;
#18050 = EDGE_CURVE ( 'NONE', #24425, #17409, #4676, .T. ) ;
#18051 = FACE_OUTER_BOUND ( 'NONE', #9798, .T. ) ;
#18052 = CARTESIAN_POINT ( 'NONE',  ( -4.320323480314926634, -1.509945384023519965, -50.80743646232500765 ) ) ;
#18053 = ORIENTED_EDGE ( 'NONE', *, *, #23014, .T. ) ;
#18054 = ADVANCED_FACE ( 'NONE', ( #6600 ), #4090, .T. ) ;
#18055 = APPLICATION_PROTOCOL_DEFINITION ( 'draft international standard', 'automotive_design', 1998, #26256 ) ;
#18056 = ORIENTED_EDGE ( 'NONE', *, *, #939, .T. ) ;
#18057 = B_SPLINE_CURVE_WITH_KNOTS ( 'NONE', 3,
 ( #17427, #12401, #28929, #9890, #14769, #14926 ),
 .UNSPECIFIED., .F., .F.,
 ( 4, 2, 4 ),
 ( 0.000000000000000000, 0.5000000000000000000, 1.000000000000000000 ),
 .UNSPECIFIED. ) ;
#18058 = ORIENTED_EDGE ( 'NONE', *, *, #11817, .T. ) ;
#18059 = CARTESIAN_POINT ( 'NONE',  ( -17.93256772572758351, -9.057264202608372727, 0.000000000000000000 ) ) ;
#18060 = DIRECTION ( 'NONE',  ( 0.3633921898465272138, -0.9316362575375356503, 9.251858538542967489E-15 ) ) ;
#18061 = CARTESIAN_POINT ( 'NONE',  ( -17.12540385515261931, -27.23755417213825325, -22.76364927353119683 ) ) ;
#18062 = CIRCLE ( 'NONE', #6013, 4.000000000000000888 ) ;
#18063 = CARTESIAN_POINT ( 'NONE',  ( 5.229687933660000176, -30.84198039109999812, 222.0000000000000000 ) ) ;
#18064 = LINE ( 'NONE', #11319, #21639 ) ;
#18065 = CARTESIAN_POINT ( 'NONE',  ( -3.891464495754538788, 2.436882555160391650, -0.6999999999999989564 ) ) ;
#18066 = CARTESIAN_POINT ( 'NONE',  ( -4.921927080085812811, 2.567569881136803733, -0.4187643563000054137 ) ) ;
#18067 = CARTESIAN_POINT ( 'NONE',  ( 10.69999999997431850, -28.51132621201893258, -31.02125039897099512 ) ) ;
#18068 = PLANE ( 'NONE',  #26556 ) ;
#18069 = ORIENTED_EDGE ( 'NONE', *, *, #3201, .F. ) ;
#18070 = CARTESIAN_POINT ( 'NONE',  ( -0.8069922590487529357, 5.436669193145879042, -11.86772091660000505 ) ) ;
#18071 = CARTESIAN_POINT ( 'NONE',  ( -4.339197174995634398, 0.6278332542688190854, -33.75783976330001224 ) ) ;
#18072 = EDGE_CURVE ( 'NONE', #5252, #23079, #13429, .T. ) ;
#18073 = CARTESIAN_POINT ( 'NONE',  ( 16.62864107198832642, 10.02943855701489895, -0.000000000000000000 ) ) ;
#18074 = CARTESIAN_POINT ( 'NONE',  ( 18.22456968101094077, 20.00000017576654443, -0.6880465830000070948 ) ) ;
#18075 = CARTESIAN_POINT ( 'NONE',  ( 14.60916111670818474, -28.04296597385482315, 8.000000000000007105 ) ) ;
#18076 = CARTESIAN_POINT ( 'NONE',  ( 27.79539923781684507, 0.5057481689249125889, 8.000000000000007105 ) ) ;
#18077 = CARTESIAN_POINT ( 'NONE',  ( -17.39770507059490967, -28.37940622391889178, -33.37710213739777032 ) ) ;
#18078 = FACE_OUTER_BOUND ( 'NONE', #16663, .T. ) ;
#18079 = CARTESIAN_POINT ( 'NONE',  ( 8.000000000355418805, -28.43737202112227536, -25.73763746985420653 ) ) ;
#18080 = CARTESIAN_POINT ( 'NONE',  ( -27.63177371540000138, 3.383804565929999804E-15, 92.63947604839999883 ) ) ;
#18081 = VERTEX_POINT ( 'NONE', #28311 ) ;
#18082 = EDGE_CURVE ( 'NONE', #28317, #2713, #25802, .T. ) ;
#18083 = VECTOR ( 'NONE', #4099, 1000.000000000000000 ) ;
#18084 = CARTESIAN_POINT ( 'NONE',  ( 10.69999999999999929, -55.00000000000000000, -42.39999999999999858 ) ) ;
#18085 = CARTESIAN_POINT ( 'NONE',  ( 2.909761405891116315, 1.959661555859188997, 230.8336353467307447 ) ) ;
#18086 = ORIENTED_EDGE ( 'NONE', *, *, #9626, .T. ) ;
#18087 = CARTESIAN_POINT ( 'NONE',  ( -9.699999999998452083, -18.04864474153841059, -34.59380650651372946 ) ) ;
#18088 = DIRECTION ( 'NONE',  ( -1.000000000000000000, 0.000000000000000000, 0.000000000000000000 ) ) ;
#18089 = CARTESIAN_POINT ( 'NONE',  ( 9.999999999963435471, -41.43235263099278143, -26.99482620601180471 ) ) ;
#18090 = ORIENTED_EDGE ( 'NONE', *, *, #70, .T. ) ;
#18091 = CARTESIAN_POINT ( 'NONE',  ( -0.9560303848909833535, -26.78297053551130702, 4.451032274715761794 ) ) ;
#18092 = ORIENTED_EDGE ( 'NONE', *, *, #7848, .F. ) ;
#18093 = EDGE_LOOP ( 'NONE', ( #9885, #26170 ) ) ;
#18094 = PRESENTATION_STYLE_ASSIGNMENT (( #1284 ) ) ;
#18095 = EDGE_LOOP ( 'NONE', ( #814, #12728 ) ) ;
#18096 = CARTESIAN_POINT ( 'NONE',  ( -1.063084826889999945, -27.77996807399999923, 224.6898005070000011 ) ) ;
#18097 = PRODUCT ( 'Nut', 'Nut', '', ( #18383 ) ) ;
#18098 = EDGE_CURVE ( 'NONE', #6771, #8375, #10370, .T. ) ;
#18099 = ORIENTED_EDGE ( 'NONE', *, *, #8628, .F. ) ;
#18100 = CARTESIAN_POINT ( 'NONE',  ( -7.224034581361331309E-06, 19.99999999982847498, 0.000000000000000000 ) ) ;
#18101 = PRODUCT_DEFINITION ( 'UNKNOWN', '', #22907, #19441 ) ;
#18102 = ORIENTED_EDGE ( 'NONE', *, *, #26237, .F. ) ;
#18103 = CARTESIAN_POINT ( 'NONE',  ( -24.35799198229911866, 13.39970082454098232, 6.098655031999994591 ) ) ;
#18104 = DIRECTION ( 'NONE',  ( -0.000000000000000000, -0.000000000000000000, -1.000000000000000000 ) ) ;
#18105 = CARTESIAN_POINT ( 'NONE',  ( 14.40197535836999876, -22.00000000000000000, -25.51324865394999719 ) ) ;
#18106 = CARTESIAN_POINT ( 'NONE',  ( -10.69999999997181028, -29.62125039897762591, -29.91132621204121733 ) ) ;
#18107 = CARTESIAN_POINT ( 'NONE',  ( -7.999999999672612994, -13.51119859729762496, -34.94474744671868649 ) ) ;
#18108 = B_SPLINE_CURVE_WITH_KNOTS ( 'NONE', 5,
 ( #25046, #30229, #10719, #20320, #29919, #30076, #8042, #8503, #25197 ),
 .UNSPECIFIED., .F., .F.,
 ( 6, 3, 6 ),
 ( 0.000000000000000000, 55.31395627320000585, 94.75474476520000167 ),
 .UNSPECIFIED. ) ;
#18109 = ORIENTED_EDGE ( 'NONE', *, *, #6621, .T. ) ;
#18110 = CARTESIAN_POINT ( 'NONE',  ( 5.530149664617865390, 2.595584118083901881, -3.079170051700004684 ) ) ;
#18111 = CARTESIAN_POINT ( 'NONE',  ( 3.710789578725085303, 2.835545959904683500, -22.86727430110000014 ) ) ;
#18112 = CARTESIAN_POINT ( 'NONE',  ( -4.195523629574152480, -27.17925737118813956, 209.7419767459480227 ) ) ;
#18113 = EDGE_CURVE ( 'NONE', #4997, #1475, #9267, .T. ) ;
#18114 = CARTESIAN_POINT ( 'NONE',  ( -10.00166578765888836, 21.00000000000104095, -54.17273359979817826 ) ) ;
#18115 = CARTESIAN_POINT ( 'NONE',  ( 25.20859211119999799, -13.29584934979999922, 224.6894611300000122 ) ) ;
#18116 = CARTESIAN_POINT ( 'NONE',  ( -27.48714010850000022, 9.611077580710000845, 229.0000000000000000 ) ) ;
#18117 = CARTESIAN_POINT ( 'NONE',  ( -20.30403093138962234, 20.00000000003553424, 1.000000000000000888 ) ) ;
#18118 = CARTESIAN_POINT ( 'NONE',  ( 10.69999999996051621, -35.47440968381866355, -24.90685721729063928 ) ) ;
#18119 = ADVANCED_FACE ( 'NONE', ( #28470 ), #18873, .T. ) ;
#18120 = AXIS2_PLACEMENT_3D ( 'NONE', #8763, #18372, #28274 ) ;
#18121 = FACE_OUTER_BOUND ( 'NONE', #24192, .T. ) ;
#18122 = CARTESIAN_POINT ( 'NONE',  ( 25.15543331629999813, -9.890973000660000736, 230.6999999999999886 ) ) ;
#18123 = CARTESIAN_POINT ( 'NONE',  ( 9.738910687886868089, -24.96785170200598358, 136.7828584120000244 ) ) ;
#18124 = VERTEX_POINT ( 'NONE', #8962 ) ;
#18125 = CARTESIAN_POINT ( 'NONE',  ( -2.948077164825098517, -3.495793300896359312, -58.77407541852498696 ) ) ;
#18126 = CARTESIAN_POINT ( 'NONE',  ( 20.30405755279999980, 20.00000000000000000, 227.7999999360000061 ) ) ;
#18127 = ORIENTED_EDGE ( 'NONE', *, *, #21960, .T. ) ;
#18128 = ADVANCED_FACE ( 'NONE', ( #19027 ), #7069, .F. ) ;
#18129 = CARTESIAN_POINT ( 'NONE',  ( -3.673964118176227700, -4.849481262172373519, -3.728945369300004753 ) ) ;
#18130 = ORIENTED_EDGE ( 'NONE', *, *, #18856, .F. ) ;
#18131 = CARTESIAN_POINT ( 'NONE',  ( -24.69967241520000201, -14.21967358789999913, 226.1000014189999945 ) ) ;
#18132 = CYLINDRICAL_SURFACE ( 'NONE', #4248, 3.000000000000002220 ) ;
#18133 = VERTEX_POINT ( 'NONE', #2360 ) ;
#18134 = CARTESIAN_POINT ( 'NONE',  ( 28.50000000000000000, -3.490128108379999702E-15, 140.0000000000000000 ) ) ;
#18135 = EDGE_LOOP ( 'NONE', ( #8617, #29288, #10714, #16555, #15351 ) ) ;
#18136 = VERTEX_POINT ( 'NONE', #5474 ) ;
#18137 = CYLINDRICAL_SURFACE ( 'NONE', #3204, 4.099999999999999645 ) ;
#18138 = B_SPLINE_CURVE_WITH_KNOTS ( 'NONE', 3,
 ( #4824, #2461, #12053, #15642 ),
 .UNSPECIFIED., .F., .F.,
 ( 4, 4 ),
 ( 0.000000000000000000, 1.000000000000000000 ),
 .UNSPECIFIED. ) ;
#18139 = SURFACE_STYLE_FILL_AREA ( #28211 ) ;
#18140 = ORIENTED_EDGE ( 'NONE', *, *, #673, .F. ) ;
#18141 = DIRECTION ( 'NONE',  ( -0.000000000000000000, -0.000000000000000000, -1.000000000000000000 ) ) ;
#18142 = CARTESIAN_POINT ( 'NONE',  ( -12.12499970530000049, 20.99999999999999645, -55.73512393530000253 ) ) ;
#18143 = CARTESIAN_POINT ( 'NONE',  ( 6.385918709370476343, 0.1527399656023400998, -64.06686508972499894 ) ) ;
#18144 = CARTESIAN_POINT ( 'NONE',  ( -23.10935684530000245, -20.42749692129999772, 228.9999999990000106 ) ) ;
#18145 = CARTESIAN_POINT ( 'NONE',  ( -7.999999999691694619, -25.92947359974649046, -31.20249410826873415 ) ) ;
#18146 = CYLINDRICAL_SURFACE ( 'NONE', #5991, 1.100000000000002309 ) ;
#18147 = DIRECTION ( 'NONE',  ( 0.000000000000000000, 0.000000000000000000, -1.000000000000000000 ) ) ;
#18148 = CARTESIAN_POINT ( 'NONE',  ( -25.16696685483287155, 13.37570800105703306, 3.997190761000024573 ) ) ;
#18149 = CARTESIAN_POINT ( 'NONE',  ( -4.602605444716575178, -1.443872896163948205, -9.085730889000004140 ) ) ;
#18150 = B_SPLINE_CURVE_WITH_KNOTS ( 'NONE', 3,
 ( #7003, #4337, #19113, #30924, #16589, #16281 ),
 .UNSPECIFIED., .F., .F.,
 ( 4, 2, 4 ),
 ( 0.000000000000000000, 0.5000000000000000000, 1.000000000000000000 ),
 .UNSPECIFIED. ) ;
#18151 = LINE ( 'NONE', #6518, #18830 ) ;
#18152 = B_SPLINE_CURVE_WITH_KNOTS ( 'NONE', 3,
 ( #21020, #30623, #18495, #4024, #1517, #13775, #28093, #18644, #11574, #3866, #27773, #28242 ),
 .UNSPECIFIED., .F., .F.,
 ( 4, 2, 2, 2, 2, 4 ),
 ( 0.000000000000000000, 0.1250000000000003886, 0.2500000000000007216, 0.5000000000000003331, 0.7500000000000001110, 1.000000000000000000 ),
 .UNSPECIFIED. ) ;
#18153 = EDGE_CURVE ( 'NONE', #17533, #7025, #14930, .T. ) ;
#18154 = DIRECTION ( 'NONE',  ( 0.8090169943751909232, 0.5877852522921378498, 0.000000000000000000 ) ) ;
#18155 = ORIENTED_EDGE ( 'NONE', *, *, #16901, .T. ) ;
#18156 = CARTESIAN_POINT ( 'NONE',  ( 24.09271802129999784, -13.87022289859999979, 223.9000014189999774 ) ) ;
#18157 = CARTESIAN_POINT ( 'NONE',  ( 24.09856112909999837, -15.21545593799999985, 225.0000014190000002 ) ) ;
#18158 = CARTESIAN_POINT ( 'NONE',  ( -23.55444264242456498, 16.04540112444970390, 8.000000000000007105 ) ) ;
#18159 = CARTESIAN_POINT ( 'NONE',  ( 18.03439872975474145, 20.21871556473540110, 0.02487532100001188518 ) ) ;
#18160 = CARTESIAN_POINT ( 'NONE',  ( -8.881784197000000993E-16, -8.881784197000000993E-16, 227.6412452697800006 ) ) ;
#18161 = EDGE_CURVE ( 'NONE', #16227, #5034, #17868, .T. ) ;
#18162 = CARTESIAN_POINT ( 'NONE',  ( -4.064488300603595228, -4.392874523441014034, -50.19612412472499585 ) ) ;
#18163 = CARTESIAN_POINT ( 'NONE',  ( -23.23277126416379801, -15.26692729116844482, 5.104183903000020450 ) ) ;
#18165 = EDGE_CURVE ( 'NONE', #15209, #30015, #16388, .T. ) ;
#18164 = CARTESIAN_POINT ( 'NONE',  ( 17.16657240419154462, 10.99999999996915179, -0.6999999999999784173 ) ) ;
#18166 = ORIENTED_EDGE ( 'NONE', *, *, #12034, .F. ) ;
#18167 = CARTESIAN_POINT ( 'NONE',  ( 23.88992819277635959, -14.21747995518237317, 4.319167818000013703 ) ) ;
#18168 = CARTESIAN_POINT ( 'NONE',  ( 27.79999999999999716, -2.355626804729999831E-11, 222.0000000000000000 ) ) ;
#18169 = CARTESIAN_POINT ( 'NONE',  ( 2.795517707053192691, -3.729300093007118289, -68.10000000002500542 ) ) ;
#18170 = TOROIDAL_SURFACE ( 'NONE', #4614, 30.50000000000000000, 3.000000000000000000 ) ;
#18171 = AXIS2_PLACEMENT_3D ( 'NONE', #6509, #9172, #11393 ) ;
#18172 = CARTESIAN_POINT ( 'NONE',  ( -1.065814103639999922E-14, 1.421085471519999843E-14, 186.3944487249999895 ) ) ;
#18173 = CARTESIAN_POINT ( 'NONE',  ( -23.77308074864635401, 14.41182440788991848, 5.146095667219259262 ) ) ;
#18174 = CARTESIAN_POINT ( 'NONE',  ( -9.000000000229999131, 20.99999999999999645, -51.10000000000000142 ) ) ;
#18175 = CARTESIAN_POINT ( 'NONE',  ( -26.57440914490000239, -3.469982507400000582, -0.6999999999999992895 ) ) ;
#18176 = CARTESIAN_POINT ( 'NONE',  ( -1.595193757947241497, 6.212219048941578059, -66.68876360962499916 ) ) ;
#18177 = ORIENTED_EDGE ( 'NONE', *, *, #1443, .T. ) ;
#18178 = CARTESIAN_POINT ( 'NONE',  ( 18.53746668656496510, 20.00005358620013141, 230.6344766825556576 ) ) ;
#18179 = ORIENTED_EDGE ( 'NONE', *, *, #17755, .T. ) ;
#18180 = CARTESIAN_POINT ( 'NONE',  ( -27.08859402333795430, -0.4928875713624353283, 0.02487529600000981667 ) ) ;
#18181 = COLOUR_RGB ( '', 0.40784314, 0.44705882, 0.49803922) ;
#18182 = EDGE_LOOP ( 'NONE', ( #2790, #12075, #6873, #15283 ) ) ;
#18183 = CARTESIAN_POINT ( 'NONE',  ( -4.000000000000000000, -31.15538618883996946, -82.34631830372681804 ) ) ;
#18184 = VECTOR ( 'NONE', #25171, 1000.000000000000000 ) ;
#18185 = LINE ( 'NONE', #21184, #10538 ) ;
#18186 = EDGE_CURVE ( 'NONE', #21002, #24719, #13370, .T. ) ;
#18187 = CARTESIAN_POINT ( 'NONE',  ( -12.29999999973083114, -29.92191803000494232, -29.18524365327784409 ) ) ;
#18188 = CARTESIAN_POINT ( 'NONE',  ( 23.81776757409229361, 15.65134803726813217, 4.999998581000003384 ) ) ;
#18189 = CARTESIAN_POINT ( 'NONE',  ( -17.38746449168020902, -25.68346034424820701, -33.41339816745249891 ) ) ;
#18190 = CARTESIAN_POINT ( 'NONE',  ( -0.9902521520970002378, -27.78273347009999839, 224.4935097720000101 ) ) ;
#18191 = VERTEX_POINT ( 'NONE', #2510 ) ;
#18192 = CARTESIAN_POINT ( 'NONE',  ( -28.49528339128749366, -0.5184828350247797646, 1.000000000000000888 ) ) ;
#18193 = DIRECTION ( 'NONE',  ( 0.000000000000000000, 2.257157423930000049E-12, 1.000000000000000000 ) ) ;
#18194 = DIRECTION ( 'NONE',  ( -1.000000000000000000, 0.000000000000000000, -6.771289003360644742E-12 ) ) ;
#18195 = DIRECTION ( 'NONE',  ( 0.000000000000000000, 0.000000000000000000, 1.000000000000000000 ) ) ;
#18196 = B_SPLINE_CURVE_WITH_KNOTS ( 'NONE', 3,
 ( #948, #23126, #5806, #1251, #1565, #27665, #5650, #13039, #29876, #3761, #10536, #20133 ),
 .UNSPECIFIED., .F., .F.,
 ( 4, 2, 2, 2, 2, 4 ),
 ( 0.000000000000000000, 0.2499999999999997780, 0.4999999999999995559, 0.6250000000000000000, 0.7500000000000004441, 1.000000000000000000 ),
 .UNSPECIFIED. ) ;
#18197 = CARTESIAN_POINT ( 'NONE',  ( -6.999999999884560786, -60.75400889059761766, -3.446705952697758590 ) ) ;
#18198 = DIRECTION ( 'NONE',  ( 0.000000000000000000, 0.9396926207858125046, 0.3420201433259318358 ) ) ;
#18199 = CARTESIAN_POINT ( 'NONE',  ( -24.83827471527357744, 12.48687850854618198, 4.999998581000003384 ) ) ;
#18200 = DIRECTION ( 'NONE',  ( 8.579942312181285869E-13, 0.9431856258987900699, 0.3322662713817151059 ) ) ;
#18201 = CARTESIAN_POINT ( 'NONE',  ( -4.652656055762370180, -1.626095028925849562, -49.65743646232498776 ) ) ;
#18202 = CARTESIAN_POINT ( 'NONE',  ( 14.77204036655656338, -23.49651729866158334, -24.64923398872036842 ) ) ;
#18203 = CARTESIAN_POINT ( 'NONE',  ( -9.000000000229999131, 21.70000000000000284, -53.60000000000000142 ) ) ;
#18204 = LINE ( 'NONE', #13655, #29364 ) ;
#18205 = VECTOR ( 'NONE', #12023, 1000.000000000000000 ) ;
#18206 = CARTESIAN_POINT ( 'NONE',  ( -14.00000000000000000, 20.99999999996851940, -58.04568740119480452 ) ) ;
#18207 = ORIENTED_EDGE ( 'NONE', *, *, #20784, .F. ) ;
#18208 = CARTESIAN_POINT ( 'NONE',  ( 1.882647771056453756, 3.960165260869607629, -32.65113063600000487 ) ) ;
#18209 = EDGE_LOOP ( 'NONE', ( #11848, #3988, #9484, #28302, #17965 ) ) ;
#18210 = EDGE_CURVE ( 'NONE', #669, #3831, #22415, .T. ) ;
#18211 = CARTESIAN_POINT ( 'NONE',  ( -5.212126283948660621, -2.851000302232811201, -53.34982952342500084 ) ) ;
#18212 = VERTEX_POINT ( 'NONE', #27038 ) ;
#18213 = ADVANCED_FACE ( 'NONE', ( #15082 ), #17724, .T. ) ;
#18214 = ORIENTED_EDGE ( 'NONE', *, *, #5615, .F. ) ;
#18215 = ORIENTED_EDGE ( 'NONE', *, *, #11958, .F. ) ;
#18216 = CARTESIAN_POINT ( 'NONE',  ( 14.67158610511795480, -31.09694805760351244, -24.99235543444519081 ) ) ;
#18217 = ADVANCED_FACE ( 'NONE', ( #14773 ), #24375, .T. ) ;
#18218 = PLANE ( 'NONE',  #3394 ) ;
#18219 = CARTESIAN_POINT ( 'NONE',  ( -17.35782682096789031, -28.15616391712504551, -23.29400885707979896 ) ) ;
#18220 = PLANE ( 'NONE',  #15447 ) ;
#18221 = CARTESIAN_POINT ( 'NONE',  ( -7.999999999718669486, -5.981227587262960554, -27.94042817487965991 ) ) ;
#18222 = CARTESIAN_POINT ( 'NONE',  ( -1.243449787579999883E-14, 0.000000000000000000, -0.6999999999999992895 ) ) ;
#18223 = CARTESIAN_POINT ( 'NONE',  ( 3.950106903291092930, 1.853988655799142959, -1.979170051700004374 ) ) ;
#18224 = LINE ( 'NONE', #13193, #21029 ) ;
#18225 = FACE_OUTER_BOUND ( 'NONE', #29166, .T. ) ;
#18226 = CARTESIAN_POINT ( 'NONE',  ( 5.093259405240584847, 0.3640143666580218373, -15.58204535869999852 ) ) ;
#18227 = CARTESIAN_POINT ( 'NONE',  ( -3.554763430470064822, 2.566410659217317924, -34.46696136359999940 ) ) ;
#18228 = CARTESIAN_POINT ( 'NONE',  ( -18.95046173579999760, -18.95046173579999760, 36.78285841159999592 ) ) ;
#18229 = ADVANCED_FACE ( 'NONE', ( #19345 ), #2813, .T. ) ;
#18230 = CARTESIAN_POINT ( 'NONE',  ( 27.74223843740156425, -9.623426708017472464, -0.5592437529999827461 ) ) ;
#18231 = CARTESIAN_POINT ( 'NONE',  ( -18.92328505709462405, 19.72870074452574940, 0.1493323239999955199 ) ) ;
#18232 = CARTESIAN_POINT ( 'NONE',  ( 18.81999291203268854, -20.80334143950547698, 8.000000000000007105 ) ) ;
#18233 = CARTESIAN_POINT ( 'NONE',  ( -3.504469657370753222, 0.9297831746172884326, 227.7188583759496794 ) ) ;
#18234 = CARTESIAN_POINT ( 'NONE',  ( 21.52822896111007367, 17.37722137477383910, -0.6577119969999878357 ) ) ;
#18235 = CARTESIAN_POINT ( 'NONE',  ( -10.00000000000000000, -13.98526668056139144, -73.96855033896248699 ) ) ;
#18236 = CARTESIAN_POINT ( 'NONE',  ( 0.4368970292349217965, -27.79681690464249044, 3.901345920999998995 ) ) ;
#18237 = VERTEX_POINT ( 'NONE', #473 ) ;
#18238 = EDGE_CURVE ( 'NONE', #16714, #2554, #5677, .T. ) ;
#18239 = AXIS2_PLACEMENT_3D ( 'NONE', #25812, #8960, #13528 ) ;
#18240 = AXIS2_PLACEMENT_3D ( 'NONE', #2580, #22089, #15002 ) ;
#18241 = CARTESIAN_POINT ( 'NONE',  ( 24.21906834310036771, 15.02342240524378703, 6.042470792000015578 ) ) ;
#18242 = CARTESIAN_POINT ( 'NONE',  ( 10.08101130880000085, 19.99999999999999645, -1.830192468500003944 ) ) ;
#18243 = VERTEX_POINT ( 'NONE', #3266 ) ;
#18244 = CIRCLE ( 'NONE', #16747, 26.80000000000000071 ) ;
#18245 = CARTESIAN_POINT ( 'NONE',  ( -2.020725942269999909, -3.500000000000000000, 227.9588918784999976 ) ) ;
#18246 = DIRECTION ( 'NONE',  ( -1.000000000000000000, 0.000000000000000000, 0.000000000000000000 ) ) ;
#18247 = CARTESIAN_POINT ( 'NONE',  ( -0.8477857712645231469, -5.155403977784983383, -0.7000226607131746492 ) ) ;
#18249 = ORIENTED_EDGE ( 'NONE', *, *, #6762, .F. ) ;
#18248 = AXIS2_PLACEMENT_3D ( 'NONE', #15108, #2993, #29728 ) ;
#18250 = DIRECTION ( 'NONE',  ( 3.924189347185962345E-12, -0.4082287037029530552, -0.9128796883888953273 ) ) ;
#18251 = ORIENTED_EDGE ( 'NONE', *, *, #6748, .T. ) ;
#18252 = VERTEX_POINT ( 'NONE', #20575 ) ;
#18253 = B_SPLINE_CURVE_WITH_KNOTS ( 'NONE', 3,
 ( #12965, #1019, #25241, #17671 ),
 .UNSPECIFIED., .F., .F.,
 ( 4, 4 ),
 ( 0.000000000000000000, 1.000000000000000000 ),
 .UNSPECIFIED. ) ;
#18254 = ORIENTED_EDGE ( 'NONE', *, *, #28669, .F. ) ;
#18255 = CARTESIAN_POINT ( 'NONE',  ( 21.59673437689999886, 17.31628621529999990, 230.6577119970000069 ) ) ;
#18256 = VERTEX_POINT ( 'NONE', #22779 ) ;
#18257 = DIRECTION ( 'NONE',  ( -1.000000000000000000, 5.687697999151106851E-16, -6.771501495036750356E-12 ) ) ;
#18258 = CARTESIAN_POINT ( 'NONE',  ( 0.000000000000000000, 22.40709319595134730, -62.85117013414870257 ) ) ;
#18259 = EDGE_CURVE ( 'NONE', #9520, #97, #15535, .T. ) ;
#18260 = CARTESIAN_POINT ( 'NONE',  ( -10.89131017139999891, -24.73114799890000270, -1.811764705899998606 ) ) ;
#18261 = CARTESIAN_POINT ( 'NONE',  ( -0.5968465743326634154, -28.49391676915515603, 5.208100973000007627 ) ) ;
#18262 = CARTESIAN_POINT ( 'NONE',  ( -26.80000000069999899, 3.281945028329999726E-15, 137.1101814800000227 ) ) ;
#18263 = CARTESIAN_POINT ( 'NONE',  ( -25.94183207552246273, -6.953987411061866020, -0.000000000000000000 ) ) ;
#18264 = CARTESIAN_POINT ( 'NONE',  ( -1.115050571030000048, -28.47845913019999742, 225.2081166120000262 ) ) ;
#18265 = AXIS2_PLACEMENT_3D ( 'NONE', #26125, #13853, #11175 ) ;
#18266 = EDGE_LOOP ( 'NONE', ( #2904, #23937, #2896, #21719 ) ) ;
#18267 = VECTOR ( 'NONE', #21553, 1000.000000000000114 ) ;
#18268 = CARTESIAN_POINT ( 'NONE',  ( -4.274305095845718938, 2.229731738857087642, -2.356264356300000085 ) ) ;
#18269 = CARTESIAN_POINT ( 'NONE',  ( -0.4514894588696835021, 4.335480228600247621, -25.38903409330000116 ) ) ;
#18270 = VECTOR ( 'NONE', #30768, 1000.000000000000000 ) ;
#18271 = CARTESIAN_POINT ( 'NONE',  ( -9.221751571650349533, -25.90851042236080914, 205.5747784761970820 ) ) ;
#18272 = B_SPLINE_CURVE_WITH_KNOTS ( 'NONE', 5,
 ( #21870, #19501, #9424, #26271, #21402, #2206, #14474, #19185, #19347, #14160, #28772, #4711, #28938, #11796, #22023 ),
 .UNSPECIFIED., .F., .F.,
 ( 6, 3, 3, 3, 6 ),
 ( 0.000000000000000000, 0.1000000000005725753, 0.4000000000022904123, 0.6999999999994271915, 1.000000000000000000 ),
 .UNSPECIFIED. ) ;
#18273 = CARTESIAN_POINT ( 'NONE',  ( -8.999999999722247068, 21.00000000000650147, -51.75449846961598865 ) ) ;
#18274 = CARTESIAN_POINT ( 'NONE',  ( 3.067534055298709816, -2.342249653522415098, -93.15928300860232980 ) ) ;
#18275 = EDGE_CURVE ( 'NONE', #14489, #16947, #21775, .T. ) ;
#18276 = CARTESIAN_POINT ( 'NONE',  ( -24.38821816920000174, 13.52880949539999911, 230.6577119970000069 ) ) ;
#18277 = CARTESIAN_POINT ( 'NONE',  ( -3.982632971385690279, -21.02717377734789039, -30.56133709589786207 ) ) ;
#18278 = CARTESIAN_POINT ( 'NONE',  ( -23.62732472759999780, -14.64974168880000072, 225.6808321819999890 ) ) ;
#18279 = EDGE_CURVE ( 'NONE', #49, #27161, #1229, .T. ) ;
#18280 = CARTESIAN_POINT ( 'NONE',  ( -9.999999999969999109, -24.87872937729999734, -30.52127062079999931 ) ) ;
#18281 = EDGE_CURVE ( 'NONE', #13263, #6773, #8180, .T. ) ;
#18282 = CARTESIAN_POINT ( 'NONE',  ( -3.511472728539999810, -17.90077611009999714, 230.6999999999999886 ) ) ;
#18283 = CARTESIAN_POINT ( 'NONE',  ( -10.00000000005918288, -28.83786139291737882, -19.12343975056708700 ) ) ;
#18284 = VERTEX_POINT ( 'NONE', #24835 ) ;
#18285 = CARTESIAN_POINT ( 'NONE',  ( 5.896017893897736784, 2.415859114112482775, -60.89141554682500157 ) ) ;
#18286 = CARTESIAN_POINT ( 'NONE',  ( -16.20306687547018143, -21.42689369263768029, 36.78285841147716440 ) ) ;
#18287 = EDGE_LOOP ( 'NONE', ( #7271, #3614, #13576, #23437 ) ) ;
#18288 = EDGE_CURVE ( 'NONE', #27710, #14643, #30305, .T. ) ;
#18289 = CARTESIAN_POINT ( 'NONE',  ( -3.845413171441346201, -3.659953273256227213, -0.8157167102000040249 ) ) ;
#18290 = VERTEX_POINT ( 'NONE', #15384 ) ;
#18291 = CARTESIAN_POINT ( 'NONE',  ( -24.80426825129999813, -14.03688870149999879, 226.0798679069999935 ) ) ;
#18292 = DIRECTION ( 'NONE',  ( 0.000000000000000000, 0.000000000000000000, 1.000000000000000000 ) ) ;
#18293 = AXIS2_PLACEMENT_3D ( 'NONE', #5293, #14896, #737 ) ;
#18294 = VERTEX_POINT ( 'NONE', #10363 ) ;
#18295 = CARTESIAN_POINT ( 'NONE',  ( -17.49999999932747130, -30.00000000000000000, -28.40000000020000215 ) ) ;
#18296 = COLOUR_RGB ( '', 0.72549020, 0.75294118, 0.79215686) ;
#18297 = ORIENTED_EDGE ( 'NONE', *, *, #4894, .F. ) ;
#18298 = VECTOR ( 'NONE', #19696, 1000.000000000000114 ) ;
#18299 = ORIENTED_EDGE ( 'NONE', *, *, #21926, .T. ) ;
#18300 = AXIS2_PLACEMENT_3D ( 'NONE', #27415, #844, #27264 ) ;
#18301 = CARTESIAN_POINT ( 'NONE',  ( 24.33346004068834034, -12.81155130650358132, 4.713248588629746827 ) ) ;
#18302 =( NAMED_UNIT ( * ) PLANE_ANGLE_UNIT ( ) SI_UNIT ( $, .RADIAN. ) );
#18303 = AXIS2_PLACEMENT_3D ( 'NONE', #8454, #27657, #24848 ) ;
#18304 = EDGE_LOOP ( 'NONE', ( #17929, #15239, #24035, #29183 ) ) ;
#18305 = CARTESIAN_POINT ( 'NONE',  ( 24.60726958095619565, -14.37955347759689317, 5.901399682999991292 ) ) ;
#18306 = ADVANCED_FACE ( 'NONE', ( #10830 ), #29548, .F. ) ;
#18307 = CARTESIAN_POINT ( 'NONE',  ( -8.699999999628362346, -14.95623164695839513, -40.37561726986208299 ) ) ;
#18308 = CARTESIAN_POINT ( 'NONE',  ( -0.8291470764733243071, -4.443337602648614215, -67.50745670422500666 ) ) ;
#18309 = CARTESIAN_POINT ( 'NONE',  ( 26.94142135619999934, 6.750155989720000084E-14, 230.0000000000000000 ) ) ;
#18310 = CARTESIAN_POINT ( 'NONE',  ( -7.999999999692273711, -26.69088343935172958, -31.40976070826679489 ) ) ;
#18311 = DIRECTION ( 'NONE',  ( -1.000000000000000000, 0.000000000000000000, 0.000000000000000000 ) ) ;
#18312 = MECHANICAL_DESIGN_GEOMETRIC_PRESENTATION_REPRESENTATION (  '', ( #25351 ), #30386 ) ;
#18313 = CARTESIAN_POINT ( 'NONE',  ( -17.32507820269023924, -22.93869108212583185, -24.97139291864791488 ) ) ;
#18314 = CARTESIAN_POINT ( 'NONE',  ( 23.47715715144835613, -20.00370206646645599, 8.000000000000007105 ) ) ;
#18315 = EDGE_CURVE ( 'NONE', #5864, #20431, #13336, .T. ) ;
#18316 = DIRECTION ( 'NONE',  ( -1.000000000000000000, 1.224606353819999829E-16, 0.000000000000000000 ) ) ;
#18317 = CARTESIAN_POINT ( 'NONE',  ( 2.536150288113637963, -3.576595042060325635, -12.12388893670000201 ) ) ;
#18318 = DIRECTION ( 'NONE',  ( -1.000000000000000000, 0.000000000000000000, 0.000000000000000000 ) ) ;
#18319 = AXIS2_PLACEMENT_3D ( 'NONE', #24377, #26727, #30992 ) ;
#18320 = CARTESIAN_POINT ( 'NONE',  ( -28.35455043824866550, -0.5159221438580913199, 0.2374258030000131470 ) ) ;
#18321 = ORIENTED_EDGE ( 'NONE', *, *, #25582, .T. ) ;
#18322 = CARTESIAN_POINT ( 'NONE',  ( -8.699999998983425797, -29.80249410822303346, -29.47052640025896508 ) ) ;
#18323 = DIRECTION ( 'NONE',  ( 0.1542166437529879919, 0.9880370573969197157, 0.000000000000000000 ) ) ;
#18324 = CARTESIAN_POINT ( 'NONE',  ( -8.999999999883337765, 20.26179938780245138, -44.10000000000000142 ) ) ;
#18325 = AXIS2_PLACEMENT_3D ( 'NONE', #14216, #2868, #28990 ) ;
#18326 = CARTESIAN_POINT ( 'NONE',  ( 26.65905076765696791, 9.650916058398387065, 0.7069222140000108734 ) ) ;
#18327 = B_SPLINE_CURVE_WITH_KNOTS ( 'NONE', 5,
 ( #5222, #11849, #23816, #9485, #2264, #21924 ),
 .UNSPECIFIED., .F., .F.,
 ( 6, 6 ),
 ( 0.000000000000000000, 2.319814892610000179 ),
 .UNSPECIFIED. ) ;
#18328 = CARTESIAN_POINT ( 'NONE',  ( -17.49199711315135986, -24.60220466956999985, -24.01086508779000184 ) ) ;
#18329 = CARTESIAN_POINT ( 'NONE',  ( -5.463799992266447525, -1.435916617982112342, -56.45102360502500005 ) ) ;
#18330 = CARTESIAN_POINT ( 'NONE',  ( -11.02757632650000019, -24.42656469639999983, -0.8308237180999975546 ) ) ;
#18331 = DIRECTION ( 'NONE',  ( 1.000000000000000000, -1.843431230198065424E-12, 2.650498504953516580E-12 ) ) ;
#18332 = ORIENTED_EDGE ( 'NONE', *, *, #21982, .F. ) ;
#18333 = LINE ( 'NONE', #18641, #24347 ) ;
#18334 = CARTESIAN_POINT ( 'NONE',  ( 27.79999999990000248, 4.333901782529999025, 226.2000000000000171 ) ) ;
#18335 = CARTESIAN_POINT ( 'NONE',  ( 2.572981240252346868, -3.481270928177104818, -68.10000000002499121 ) ) ;
#18336 = TOROIDAL_SURFACE ( 'NONE', #3255, 24.50000000000000000, 4.000000000000000000 ) ;
#18337 = MECHANICAL_DESIGN_GEOMETRIC_PRESENTATION_REPRESENTATION (  '', ( #6275 ), #7292 ) ;
#18338 = CARTESIAN_POINT ( 'NONE',  ( -3.040504020835836041, -1.733590291693717145, -0.6999999999999784173 ) ) ;
#18339 = CARTESIAN_POINT ( 'NONE',  ( -4.246103237644704542, 0.8932448209632969371, -44.10000000002499121 ) ) ;
#18340 = FILL_AREA_STYLE_COLOUR ( '', #3235 ) ;
#18341 = CARTESIAN_POINT ( 'NONE',  ( 7.801126876359127493, -5.730966291675875013, -27.38079468629169355 ) ) ;
#18342 = CARTESIAN_POINT ( 'NONE',  ( -0.1113126277073478027, 4.304903297084355707, -39.57881079973518723 ) ) ;
#18343 = EDGE_CURVE ( 'NONE', #24119, #29525, #17582, .T. ) ;
#18344 = CARTESIAN_POINT ( 'NONE',  ( -1.470080522021702363, 5.724986182348157371, -67.00876360962500655 ) ) ;
#18345 = TOROIDAL_SURFACE ( 'NONE', #2283, 18.16530045470000232, 1.000000000000000000 ) ;
#18346 = ORIENTED_EDGE ( 'NONE', *, *, #18315, .F. ) ;
#18347 = CARTESIAN_POINT ( 'NONE',  ( 19.47906472345739459, 20.00001843740129814, 230.2805668407570181 ) ) ;
#18348 = ADVANCED_FACE ( 'NONE', ( #1387 ), #25139, .T. ) ;
#18349 = ORIENTED_EDGE ( 'NONE', *, *, #1919, .T. ) ;
#18350 = ADVANCED_FACE ( 'NONE', ( #19955 ), #22476, .F. ) ;
#18351 = CARTESIAN_POINT ( 'NONE',  ( -27.77052805885580966, -0.5052956280425512370, 0.7069222069999991920 ) ) ;
#18352 = EDGE_CURVE ( 'NONE', #16525, #26528, #29531, .T. ) ;
#18353 = ORIENTED_EDGE ( 'NONE', *, *, #30622, .F. ) ;
#18354 = CARTESIAN_POINT ( 'NONE',  ( 23.66291322330000213, -14.59162663150000050, 225.7601370010000039 ) ) ;
#18355 = B_SPLINE_CURVE_WITH_KNOTS ( 'NONE', 3,
 ( #8227, #27138, #8385, #22261, #17832, #29488 ),
 .UNSPECIFIED., .F., .F.,
 ( 4, 2, 4 ),
 ( 0.000000000000000000, 0.5000000000000000000, 1.000000000000000000 ),
 .UNSPECIFIED. ) ;
#18356 = FILL_AREA_STYLE ('',( #18814 ) ) ;
#18357 = CARTESIAN_POINT ( 'NONE',  ( -8.699999999660043670, -18.28443321518998133, -36.42483785847389299 ) ) ;
#18358 = CARTESIAN_POINT ( 'NONE',  ( -7.105427357599999217E-15, 0.000000000000000000, 86.78285841159998881 ) ) ;
#18359 = CARTESIAN_POINT ( 'NONE',  ( -10.69999999999999929, -24.69736308950000137, -26.47023749829999772 ) ) ;
#18360 = CARTESIAN_POINT ( 'NONE',  ( -12.59531001298596387, -22.00000000000000355, -30.73779220032784210 ) ) ;
#18361 = AXIS2_PLACEMENT_3D ( 'NONE', #17192, #12164, #23986 ) ;
#18362 = CARTESIAN_POINT ( 'NONE',  ( -17.12355120911344741, -21.99999999999975842, -25.78113483056816690 ) ) ;
#18363 = ORIENTED_EDGE ( 'NONE', *, *, #947, .T. ) ;
#18364 = CARTESIAN_POINT ( 'NONE',  ( -0.1685424049532343038, -3.960684645455483377, -44.10000000002498410 ) ) ;
#18365 = DIRECTION ( 'NONE',  ( -1.000000000000000000, -1.771497531999344233E-11, 0.000000000000000000 ) ) ;
#18366 = CARTESIAN_POINT ( 'NONE',  ( 9.707106781189999367, -55.00000000000000000, -43.10710678118599759 ) ) ;
#18367 = CARTESIAN_POINT ( 'NONE',  ( -3.341854967535827114, 1.211737404705432564, 230.8123217011524844 ) ) ;
#18368 = CARTESIAN_POINT ( 'NONE',  ( -8.699999998935181722, -13.66682223737418944, -36.55330428419230060 ) ) ;
#18369 = DIRECTION ( 'NONE',  ( 1.667044707805962905E-12, -0.4082287037029530552, -0.9128796883888953273 ) ) ;
#18370 = B_SPLINE_CURVE_WITH_KNOTS ( 'NONE', 1,
 ( #25931, #23426 ),
 .UNSPECIFIED., .F., .F.,
 ( 2, 2 ),
 ( -0.7000000000219999130, 5.329070518200751394E-15 ),
 .UNSPECIFIED. ) ;
#18371 = DIRECTION ( 'NONE',  ( 0.000000000000000000, 0.000000000000000000, -1.000000000000000000 ) ) ;
#18372 = DIRECTION ( 'NONE',  ( -1.000000000000000000, 0.000000000000000000, -6.771000000000000128E-12 ) ) ;
#18373 = CARTESIAN_POINT ( 'NONE',  ( 1.321824945545745145, 4.319062652178982553, -51.46125421262499344 ) ) ;
#18374 = CARTESIAN_POINT ( 'NONE',  ( -23.24663841809999809, -14.69162354060000020, 5.000000000000000000 ) ) ;
#18375 = CARTESIAN_POINT ( 'NONE',  ( 7.603592957572457678, 4.263853735895689390, -39.55878959099714365 ) ) ;
#18376 = DIRECTION ( 'NONE',  ( 0.000000000000000000, -1.000000000000000000, 2.257145581549999994E-12 ) ) ;
#18377 = CARTESIAN_POINT ( 'NONE',  ( -1.087768546147131588, -27.47890868157812605, 224.7820750495661741 ) ) ;
#18378 = VERTEX_POINT ( 'NONE', #17380 ) ;
#18379 = CARTESIAN_POINT ( 'NONE',  ( 3.123710955063047745, -2.074832491810059132, -36.45875473020001323 ) ) ;
#18380 = VERTEX_POINT ( 'NONE', #26985 ) ;
#18381 = CARTESIAN_POINT ( 'NONE',  ( -3.985743628842679076, -2.180176701716177057, -53.34982952342500084 ) ) ;
#18382 = ORIENTED_EDGE ( 'NONE', *, *, #19309, .T. ) ;
#18383 = PRODUCT_CONTEXT ( 'NONE', #21852, 'mechanical' ) ;
#18384 = ORIENTED_EDGE ( 'NONE', *, *, #26028, .T. ) ;
#18385 = EDGE_CURVE ( 'NONE', #10023, #20819, #12217, .T. ) ;
#18386 = VERTEX_POINT ( 'NONE', #24625 ) ;
#18387 = CARTESIAN_POINT ( 'NONE',  ( -10.99999999999209344, -15.94902145825930617, -35.53273252503056767 ) ) ;
#18388 = CARTESIAN_POINT ( 'NONE',  ( 4.847509070911421247, -10.00908554550677643, -35.93521779026085028 ) ) ;
#18389 = CARTESIAN_POINT ( 'NONE',  ( 0.000000000000000000, -55.00000000000000000, -44.10000000000000142 ) ) ;
#18390 = CARTESIAN_POINT ( 'NONE',  ( 3.555688610909999881, -11.76883225949999989, 232.6627648150000027 ) ) ;
#18391 = CARTESIAN_POINT ( 'NONE',  ( -0.09701118521228915825, -27.50000000070000539, 3.900000000000003020 ) ) ;
#18392 = CARTESIAN_POINT ( 'NONE',  ( -17.49999999969999820, -27.00000000000000000, -28.40000000020000215 ) ) ;
#18393 = CARTESIAN_POINT ( 'NONE',  ( 4.345117593642236820, 2.039387521354418809, -1.541670051700000377 ) ) ;
#18394 = DIRECTION ( 'NONE',  ( -0.9690327085511358796, 0.2219413702090850260, -0.1082480390019309596 ) ) ;
#18395 = CARTESIAN_POINT ( 'NONE',  ( 8.000000000279957391, -18.28443193505134445, -36.42483736938841332 ) ) ;
#18396 = CARTESIAN_POINT ( 'NONE',  ( -4.278952157217899455, -0.8066629416743122949, -16.59949426530001304 ) ) ;
#18397 = CARTESIAN_POINT ( 'NONE',  ( 3.956700543085249322, -2.628121156294186633, -34.95875473020000612 ) ) ;
#18398 = CARTESIAN_POINT ( 'NONE',  ( 2.504034607669999968, 5.302315698040000136, 226.6412452697800006 ) ) ;
#18399 = ADVANCED_FACE ( 'NONE', ( #16917 ), #16240, .T. ) ;
#18400 = CARTESIAN_POINT ( 'NONE',  ( -1.087555935801710172, -26.77834284441886226, 5.218051574395796699 ) ) ;
#18401 = CARTESIAN_POINT ( 'NONE',  ( 0.8260714173989999187, -28.48835664879999996, 224.2403730839999980 ) ) ;
#18402 = CARTESIAN_POINT ( 'NONE',  ( 8.522909508489858510, -26.72774706475087569, 8.000000000000007105 ) ) ;
#18403 = CARTESIAN_POINT ( 'NONE',  ( -28.49999999990000177, 3.410703877680000051, 222.0000000000000000 ) ) ;
#18404 = CARTESIAN_POINT ( 'NONE',  ( 22.36497543530602172, 18.05262891234276168, 0.2374258030000131470 ) ) ;
#18405 = FACE_OUTER_BOUND ( 'NONE', #1436, .T. ) ;
#18406 = DIRECTION ( 'NONE',  ( 1.000000000000000000, 0.000000000000000000, 0.000000000000000000 ) ) ;
#18407 = B_SPLINE_CURVE_WITH_KNOTS ( 'NONE', 3,
 ( #20683, #15486, #25566, #4002, #20366, #2275, #23983, #23831, #25725, #21150 ),
 .UNSPECIFIED., .F., .F.,
 ( 4, 2, 2, 2, 4 ),
 ( 0.000000000000000000, 0.2499999999999999445, 0.4999999999999998890, 0.7499999999999997780, 1.000000000000000000 ),
 .UNSPECIFIED. ) ;
#18408 = ADVANCED_FACE ( 'NONE', ( #2911 ), #17224, .F. ) ;
#18409 = CARTESIAN_POINT ( 'NONE',  ( -3.766115772130143036, -0.5867141459235316603, -69.09187603409807821 ) ) ;
#18410 = EDGE_LOOP ( 'NONE', ( #17210, #4642, #11420, #14450 ) ) ;
#18411 = DIRECTION ( 'NONE',  ( 0.000000000000000000, 0.8660254037843289066, 0.5000000000001899592 ) ) ;
#18412 = CARTESIAN_POINT ( 'NONE',  ( -25.08454981450000076, -13.52946590090000178, 224.2397332909999932 ) ) ;
#18413 = CARTESIAN_POINT ( 'NONE',  ( 0.6094692351073999204, -5.151249438444421180, -0.7000440620407059056 ) ) ;
#18414 = ORIENTED_EDGE ( 'NONE', *, *, #4030, .F. ) ;
#18415 = CARTESIAN_POINT ( 'NONE',  ( 0.5498575204214891654, -4.501552459773711767, -44.18057807742500387 ) ) ;
#18416 = ORIENTED_EDGE ( 'NONE', *, *, #14303, .F. ) ;
#18417 = EDGE_LOOP ( 'NONE', ( #4883, #8656, #875, #16833, #17098 ) ) ;
#18418 =( LENGTH_UNIT ( ) NAMED_UNIT ( * ) SI_UNIT ( .MILLI., .METRE. ) );
#18419 = VERTEX_POINT ( 'NONE', #22426 ) ;
#18420 = CARTESIAN_POINT ( 'NONE',  ( -2.020725942159999899, 3.500000000000000000, 229.2412452703699728 ) ) ;
#18421 = EDGE_LOOP ( 'NONE', ( #13741, #12764, #6963, #12609, #294 ) ) ;
#18422 = B_SPLINE_CURVE_WITH_KNOTS ( 'NONE', 5,
 ( #8206, #27266, #17807, #25219, #3975, #13571 ),
 .UNSPECIFIED., .F., .F.,
 ( 6, 6 ),
 ( -2.000000000000000000, 0.000000000000000000 ),
 .UNSPECIFIED. ) ;
#18423 = LINE ( 'NONE', #13389, #24115 ) ;
#18424 = FILL_AREA_STYLE ('',( #8821 ) ) ;
#18425 = FACE_OUTER_BOUND ( 'NONE', #28424, .T. ) ;
#18426 = CARTESIAN_POINT ( 'NONE',  ( -3.873164306258084277, -2.119290473559455101, -95.69213427732501032 ) ) ;
#18427 = CARTESIAN_POINT ( 'NONE',  ( 8.903108651239925564, -22.82508830966962421, 190.0000000000000000 ) ) ;
#18428 = CARTESIAN_POINT ( 'NONE',  ( -0.1000000000151932966, -15.94902145824367246, -35.53273252498938461 ) ) ;
#18429 = EDGE_CURVE ( 'NONE', #20670, #7630, #22115, .T. ) ;
#18430 = DIRECTION ( 'NONE',  ( 2.197671641579999817E-16, 1.000000000000000000, 0.000000000000000000 ) ) ;
#18431 = VERTEX_POINT ( 'NONE', #15032 ) ;
#18432 = B_SPLINE_CURVE_WITH_KNOTS ( 'NONE', 3,
 ( #14343, #26747, #23942, #7697, #19671, #11965, #5184, #9919, #9758, #14797, #28955 ),
 .UNSPECIFIED., .F., .F.,
 ( 4, 1, 1, 1, 2, 2, 4 ),
 ( 0.000000000000000000, 0.2499999999999971134, 0.3749999999999970579, 0.4374999999999971689, 0.4687499999999974465, 0.4999999999999977796, 1.000000000000000000 ),
 .UNSPECIFIED. ) ;
#18433 = CARTESIAN_POINT ( 'NONE',  ( 4.116710911288352648, -1.508563155650267884, -5.836105321700007842 ) ) ;
#18434 = CARTESIAN_POINT ( 'NONE',  ( -6.202057249109299342, 1.908294659314309305, -22.32289663399999924 ) ) ;
#18435 = DIRECTION ( 'NONE',  ( 1.000000000000000000, -0.000000000000000000, -2.257150022439999944E-12 ) ) ;
#18436 = CARTESIAN_POINT ( 'NONE',  ( -10.49791847189999849, -25.00000000000000000, -3.602081527999998034 ) ) ;
#18437 = DIRECTION ( 'NONE',  ( 1.000000000000000000, -3.981000000000000101E-12, 1.940999999999999908E-12 ) ) ;
#18438 = CARTESIAN_POINT ( 'NONE',  ( -7.999999999722595234, -5.572998883578264895, -27.02754848648259767 ) ) ;
#18439 = DIRECTION ( 'NONE',  ( 0.000000000000000000, 0.000000000000000000, -1.000000000000000000 ) ) ;
#18440 = CIRCLE ( 'NONE', #21463, 17.61822726820000184 ) ;
#18441 = CARTESIAN_POINT ( 'NONE',  ( -8.903108651239966420, -22.82508830966961000, 140.0000000000000000 ) ) ;
#18442 = DIRECTION ( 'NONE',  ( 0.000000000000000000, -0.3420201433259318913, 0.9396926207858126157 ) ) ;
#18443 = CARTESIAN_POINT ( 'NONE',  ( -11.69999999989999928, -24.11120071630000083, -1.399999999999998579 ) ) ;
#18444 = EDGE_LOOP ( 'NONE', ( #30022, #9324, #10335, #1900 ) ) ;
#18445 = CARTESIAN_POINT ( 'NONE',  ( 1.672654430053971852, 5.259243695923226269, -59.66492395752499789 ) ) ;
#18446 = CARTESIAN_POINT ( 'NONE',  ( 20.30405755279999980, 20.00000000000000000, 227.3999999149999951 ) ) ;
#18447 = VERTEX_POINT ( 'NONE', #21964 ) ;
#18448 = EDGE_CURVE ( 'NONE', #25327, #974, #4021, .T. ) ;
#18449 = ORIENTED_EDGE ( 'NONE', *, *, #14527, .F. ) ;
#18450 = CARTESIAN_POINT ( 'NONE',  ( 23.55447120710000064, 16.04539730700000177, 222.0000000000000000 ) ) ;
#18451 = CARTESIAN_POINT ( 'NONE',  ( -1.058439502263211374, 6.005994971325610443, -19.83583244400000112 ) ) ;
#18452 = EDGE_LOOP ( 'NONE', ( #20620, #17931, #13361, #27571 ) ) ;
#18453 = CARTESIAN_POINT ( 'NONE',  ( -24.71725143720000162, -14.18911829940000047, 226.0986578700000109 ) ) ;
#18454 = LINE ( 'NONE', #6649, #12255 ) ;
#18455 = EDGE_LOOP ( 'NONE', ( #15277, #11256, #15743 ) ) ;
#18456 = ORIENTED_EDGE ( 'NONE', *, *, #22144, .F. ) ;
#18457 = VERTEX_POINT ( 'NONE', #5575 ) ;
#18458 = CARTESIAN_POINT ( 'NONE',  ( -16.85343921402336775, -7.900182044543379689, -0.6999999999999784173 ) ) ;
#18459 = ORIENTED_EDGE ( 'NONE', *, *, #13774, .T. ) ;
#18460 = CARTESIAN_POINT ( 'NONE',  ( 24.37165445055180157, -14.77472140295711434, 4.999998581000003384 ) ) ;
#18461 = CARTESIAN_POINT ( 'NONE',  ( 0.2748893566200901750, -2.100000000056975402, 226.6412452697800290 ) ) ;
#18462 = EDGE_CURVE ( 'NONE', #4458, #15161, #21638, .T. ) ;
#18463 = CARTESIAN_POINT ( 'NONE',  ( 4.441146713721680683, -1.990734395214994734, -66.87841551502499726 ) ) ;
#18464 = CARTESIAN_POINT ( 'NONE',  ( -6.394884621839999216E-14, -26.80000000000000071, 226.0999999999999943 ) ) ;
#18465 =( GEOMETRIC_REPRESENTATION_CONTEXT ( 3 ) GLOBAL_UNCERTAINTY_ASSIGNED_CONTEXT ( ( #17569 ) ) GLOBAL_UNIT_ASSIGNED_CONTEXT ( ( #7363, #23747, #12233 ) ) REPRESENTATION_CONTEXT ( 'NONE', 'WORKASPACE' ) );
#18466 = EDGE_CURVE ( 'NONE', #17290, #10264, #8856, .T. ) ;
#18467 = CARTESIAN_POINT ( 'NONE',  ( 7.638687372243864182, -5.597492073746726859, -34.74908987207204092 ) ) ;
#18468 = CARTESIAN_POINT ( 'NONE',  ( -8.237618942580001047, -27.55517656820000028, 222.0000000000000000 ) ) ;
#18469 = CARTESIAN_POINT ( 'NONE',  ( -17.42785659857125324, -23.57399342402652920, -24.60449948155520516 ) ) ;
#18470 = ORIENTED_EDGE ( 'NONE', *, *, #11756, .F. ) ;
#18471 = CARTESIAN_POINT ( 'NONE',  ( 11.63809019220000174, -24.14124255329999968, -0.6999999999999992895 ) ) ;
#18472 = EDGE_CURVE ( 'NONE', #26129, #27980, #15175, .T. ) ;
#18473 = CARTESIAN_POINT ( 'NONE',  ( 3.550610403408205329, -5.007233058897099021, -12.12388893670000201 ) ) ;
#18474 = CARTESIAN_POINT ( 'NONE',  ( 24.08872333959831380, -11.87645233066226069, 136.7828584119999960 ) ) ;
#18475 = CARTESIAN_POINT ( 'NONE',  ( -10.69999999968908355, -29.79578670632410820, -30.01215105656972071 ) ) ;
#18476 = VERTEX_POINT ( 'NONE', #3214 ) ;
#18477 = CARTESIAN_POINT ( 'NONE',  ( 21.51557202503504129, 16.01570388398135236, -1.399999999999998579 ) ) ;
#18478 = DIRECTION ( 'NONE',  ( 0.3090169943750400994, -0.9510565162951234441, 0.000000000000000000 ) ) ;
#18479 = CARTESIAN_POINT ( 'NONE',  ( -26.49877110809999792, 8.898239018390000865, 222.0000000000000000 ) ) ;
#18480 = CARTESIAN_POINT ( 'NONE',  ( 27.16228374367956988, 4.990250640343800725, 0.08279779300002232389 ) ) ;
#18481 = CARTESIAN_POINT ( 'NONE',  ( -9.000000000000000000, -130.0000000000000000, -44.10000000000000142 ) ) ;
#18482 = CARTESIAN_POINT ( 'NONE',  ( 5.235465350887244185, -2.882605534178610984, -58.30843849682499780 ) ) ;
#18483 = AXIS2_PLACEMENT_3D ( 'NONE', #11544, #20675, #1639 ) ;
#18484 = ADVANCED_FACE ( 'NONE', ( #12823 ), #24163, .F. ) ;
#18485 = CARTESIAN_POINT ( 'NONE',  ( -10.89131017139999891, -24.73114799960000099, -1.811764705899998606 ) ) ;
#18486 = CARTESIAN_POINT ( 'NONE',  ( 0.000000000000000000, 0.000000000000000000, 210.0000000000000284 ) ) ;
#18487 = ORIENTED_EDGE ( 'NONE', *, *, #14841, .T. ) ;
#18488 = CARTESIAN_POINT ( 'NONE',  ( 24.60726958085803417, -14.37955347769869263, 4.098597479000015475 ) ) ;
#18489 = CARTESIAN_POINT ( 'NONE',  ( -8.700000000022731328, -117.0726643331094152, 17.59013758954728246 ) ) ;
#18490 = VECTOR ( 'NONE', #30548, 1000.000000000000000 ) ;
#18491 = CARTESIAN_POINT ( 'NONE',  ( 2.491610509676117857, -3.506118418580284946, -68.10000000002500542 ) ) ;
#18492 = VECTOR ( 'NONE', #21939, 1000.000000000000000 ) ;
#18493 = EDGE_CURVE ( 'NONE', #18717, #25785, #22047, .T. ) ;
#18494 = B_SPLINE_CURVE_WITH_KNOTS ( 'NONE', 1,
 ( #28757, #16493 ),
 .UNSPECIFIED., .F., .F.,
 ( 2, 2 ),
 ( -0.7000000000189999794, 2.331468351712828735E-15 ),
 .UNSPECIFIED. ) ;
#18495 = CARTESIAN_POINT ( 'NONE',  ( 0.4344627458603688153, 2.676789689232947467, -67.90405777868647874 ) ) ;
#18496 = CARTESIAN_POINT ( 'NONE',  ( -4.411068591882468581, 1.131342447431700871, -44.10000000002499121 ) ) ;
#18497 = PRESENTATION_STYLE_ASSIGNMENT (( #28410 ) ) ;
#18498 = ORIENTED_EDGE ( 'NONE', *, *, #27405, .F. ) ;
#18499 = CARTESIAN_POINT ( 'NONE',  ( -9.700000000002093614, -15.94902145825307826, -35.53273252502644652 ) ) ;
#18500 = CARTESIAN_POINT ( 'NONE',  ( 3.542472921321142110, 4.818407451951889797, -66.64226422552501106 ) ) ;
#18501 = ORIENTED_EDGE ( 'NONE', *, *, #11718, .F. ) ;
#18502 = LINE ( 'NONE', #18966, #30517 ) ;
#18503 = ORIENTED_EDGE ( 'NONE', *, *, #14700, .T. ) ;
#18504 = CARTESIAN_POINT ( 'NONE',  ( -19.79257232079999795, 19.51192870039999860, 229.1494017060000203 ) ) ;
#18505 = EDGE_LOOP ( 'NONE', ( #9207, #23499, #18127, #10175 ) ) ;
#18506 = CARTESIAN_POINT ( 'NONE',  ( 8.881784197000000993E-16, -2.220446049249999755E-16, 227.6412452699999847 ) ) ;
#18507 = CARTESIAN_POINT ( 'NONE',  ( 24.49999999589999788, -3.000285566359999846E-15, 190.0000000000000000 ) ) ;
#18508 = CARTESIAN_POINT ( 'NONE',  ( -3.361572482953519625, -1.073845131765873484, 0.000000000000000000 ) ) ;
#18509 = CARTESIAN_POINT ( 'NONE',  ( -0.3682501489830092845, -27.79783598715961901, 4.319846982000025370 ) ) ;
#18510 = VECTOR ( 'NONE', #23283, 1000.000000000000000 ) ;
#18511 = DIRECTION ( 'NONE',  ( -0.3090169943750401549, -0.9510565162951233331, 0.000000000000000000 ) ) ;
#18512 = CARTESIAN_POINT ( 'NONE',  ( 10.49791847189999849, -25.00000000000000000, -3.602081527999998034 ) ) ;
#18513 = VERTEX_POINT ( 'NONE', #15409 ) ;
#18514 = DIRECTION ( 'NONE',  ( 0.7071067811865467956, 0.6644630243886068266, 0.2418447626481644297 ) ) ;
#18515 = CARTESIAN_POINT ( 'NONE',  ( 26.11035454923439403, 9.897950727584628794, 8.000000000000007105 ) ) ;
#18516 = CARTESIAN_POINT ( 'NONE',  ( 19.06862361850000198, 19.69237242210000005, 229.7996270940000159 ) ) ;
#18517 = CARTESIAN_POINT ( 'NONE',  ( 4.334836395473461224, -2.879286697580460519, -35.69999999999999574 ) ) ;
#18518 = DIRECTION ( 'NONE',  ( -1.000000000000000000, 5.687697999151106851E-16, -6.771501495036750356E-12 ) ) ;
#18519 = CARTESIAN_POINT ( 'NONE',  ( 11.93900533800000119, -2.124654349530000097, 230.6412452697800006 ) ) ;
#18520 = ADVANCED_FACE ( 'NONE', ( #5189 ), #27063, .F. ) ;
#18521 = CARTESIAN_POINT ( 'NONE',  ( 23.23277120355932723, 15.26692725134781625, 4.854156652956985951 ) ) ;
#18522 = CARTESIAN_POINT ( 'NONE',  ( -17.84839340654884055, 10.55214128775187810, -1.400000000000001910 ) ) ;
#18523 = CARTESIAN_POINT ( 'NONE',  ( -0.9881560945370695404, 5.823346091562972227, -50.77792092402498980 ) ) ;
#18524 = CIRCLE ( 'NONE', #23052, 1.099999999570000497 ) ;
#18525 = EDGE_CURVE ( 'NONE', #22642, #29777, #3293, .T. ) ;
#18526 = CARTESIAN_POINT ( 'NONE',  ( -23.30309534863303256, -14.60301215427377031, 5.490554140840532504 ) ) ;
#18527 = CARTESIAN_POINT ( 'NONE',  ( 14.79527398937326410, -28.65846030549727175, -33.21580101399630536 ) ) ;
#18528 = CARTESIAN_POINT ( 'NONE',  ( -16.95798644146054812, 9.897551528143511135, 0.000000000000000000 ) ) ;
#18529 = CARTESIAN_POINT ( 'NONE',  ( -8.699999999715885224, -26.99999999997790923, -28.40000000002690683 ) ) ;
#18530 = ORIENTED_EDGE ( 'NONE', *, *, #3269, .F. ) ;
#18531 = CARTESIAN_POINT ( 'NONE',  ( -24.25909092259999866, -14.95913241689999928, 224.2397348780000073 ) ) ;
#18532 = TOROIDAL_SURFACE ( 'NONE', #4967, 24.50000000000000000, 3.200000000000000178 ) ;
#18533 = VERTEX_POINT ( 'NONE', #10543 ) ;
#18534 = CARTESIAN_POINT ( 'NONE',  ( -1.065285671501096765, -5.119323817795550902, -53.67706695232500635 ) ) ;
#18535 = ORIENTED_EDGE ( 'NONE', *, *, #15121, .F. ) ;
#18536 = PRODUCT_CONTEXT ( 'NONE', #6954, 'mechanical' ) ;
#18537 = VERTEX_POINT ( 'NONE', #5501 ) ;
#18538 = CARTESIAN_POINT ( 'NONE',  ( 0.000000000000000000, 0.000000000000000000, 87.93968498540000667 ) ) ;
#18539 = EDGE_LOOP ( 'NONE', ( #9440, #29868, #16908, #2416, #24304, #19250, #23466, #27118 ) ) ;
#18540 = CARTESIAN_POINT ( 'NONE',  ( 14.84842474946386126, -29.69419767703834623, -24.18168994580233289 ) ) ;
#18541 = CARTESIAN_POINT ( 'NONE',  ( 5.480062667635420937, -9.140703088408896448, -36.35875621392638379 ) ) ;
#18542 = CARTESIAN_POINT ( 'NONE',  ( -17.40775135787899686, -30.56179203344806083, -24.68289889760973210 ) ) ;
#18543 = VECTOR ( 'NONE', #25287, 1000.000000000000000 ) ;
#18544 = FACE_OUTER_BOUND ( 'NONE', #16065, .T. ) ;
#18545 = CARTESIAN_POINT ( 'NONE',  ( -16.17397428881745469, -8.107840965152638191, -0.6999999999999783062 ) ) ;
#18546 = DIRECTION ( 'NONE',  ( 0.000000000000000000, 0.000000000000000000, 1.000000000000000000 ) ) ;
#18547 = CARTESIAN_POINT ( 'NONE',  ( 1.699015317690025118, 6.330513620609809600, -1.453410702900004292 ) ) ;
#18548 = ADVANCED_BREP_SHAPE_REPRESENTATION ( '', ( #72, #17722 ), #16292 ) ;
#18549 = CARTESIAN_POINT ( 'NONE',  ( 26.05511440539999768, -14.93230011240000010, 229.0000000000000000 ) ) ;
#18550 = EDGE_LOOP ( 'NONE', ( #6399, #5341, #6734, #2220 ) ) ;
#18551 = CARTESIAN_POINT ( 'NONE',  ( -4.498618707852113374, 2.988074248075567318, -44.10000000002499121 ) ) ;
#18552 = CARTESIAN_POINT ( 'NONE',  ( -2.183849900456023896, 3.899926742306373928, -16.67761783620000315 ) ) ;
#18553 = CARTESIAN_POINT ( 'NONE',  ( -4.901082056047598279, -4.330235462250267453, -33.23447003409999212 ) ) ;
#18554 = VECTOR ( 'NONE', #3057, 1000.000000000000000 ) ;
#18555 = VECTOR ( 'NONE', #7592, 1000.000000000000114 ) ;
#18556 = CARTESIAN_POINT ( 'NONE',  ( -1.100000000000000089, -26.77741585740000119, 5.000000000000000000 ) ) ;
#18557 = CARTESIAN_POINT ( 'NONE',  ( 1.063086518139999992, -27.77985718819999761, 224.6898179359999972 ) ) ;
#18558 = CARTESIAN_POINT ( 'NONE',  ( -27.77990052619939476, -1.357541420128717702, 8.000000000000007105 ) ) ;
#18559 = CARTESIAN_POINT ( 'NONE',  ( -2.631336845234771626, 2.442053353369756152, 227.6979960600623087 ) ) ;
#18560 = EDGE_CURVE ( 'NONE', #15714, #10036, #22288, .T. ) ;
#18561 = CARTESIAN_POINT ( 'NONE',  ( 26.71513120331102797, 4.908099852724521206, -0.6999999999999784173 ) ) ;
#18562 = DIRECTION ( 'NONE',  ( 0.000000000000000000, 0.000000000000000000, -1.000000000000000000 ) ) ;
#18563 = CARTESIAN_POINT ( 'NONE',  ( -17.72521362118247623, 11.65988689034122316, -4.336808689942018722E-16 ) ) ;
#18564 = EDGE_CURVE ( 'NONE', #25887, #17381, #4697, .T. ) ;
#18565 = DIRECTION ( 'NONE',  ( -1.224606353819999829E-16, -1.000000000000000000, 0.000000000000000000 ) ) ;
#18566 = VERTEX_POINT ( 'NONE', #10686 ) ;
#18567 = CARTESIAN_POINT ( 'NONE',  ( -22.63992238019999803, -14.34133587289999845, 225.0000000000000000 ) ) ;
#18568 = DIRECTION ( 'NONE',  ( 1.000000000000000000, 0.000000000000000000, 0.000000000000000000 ) ) ;
#18569 = CARTESIAN_POINT ( 'NONE',  ( -27.79999999999999716, -2.354383354940000152E-11, 222.0000000000000000 ) ) ;
#18570 = EDGE_LOOP ( 'NONE', ( #14295, #11069, #14176, #22951 ) ) ;
#18571 = CARTESIAN_POINT ( 'NONE',  ( 2.472051776111518162, -3.869239954018615535, -44.31966640442499994 ) ) ;
#18572 = VERTEX_POINT ( 'NONE', #17305 ) ;
#18573 = VERTEX_POINT ( 'NONE', #20138 ) ;
#18574 = VECTOR ( 'NONE', #12049, 1000.000000000000000 ) ;
#18575 =( NAMED_UNIT ( * ) SI_UNIT ( $, .STERADIAN. ) SOLID_ANGLE_UNIT ( ) );
#18576 = VERTEX_POINT ( 'NONE', #14803 ) ;
#18577 = DIRECTION ( 'NONE',  ( 0.000000000000000000, 0.000000000000000000, 1.000000000000000000 ) ) ;
#18578 = ORIENTED_EDGE ( 'NONE', *, *, #9471, .F. ) ;
#18579 = LINE ( 'NONE', #9444, #22605 ) ;
#18580 = DIRECTION ( 'NONE',  ( -2.257102469710000208E-12, 0.000000000000000000, 1.000000000000000000 ) ) ;
#18581 = CARTESIAN_POINT ( 'NONE',  ( 3.742179766445304256, 0.3990864396118201651, -35.70000000000000284 ) ) ;
#18582 = B_SPLINE_CURVE_WITH_KNOTS ( 'NONE', 3,
 ( #13867, #21257, #23474, #23160, #14026, #27868 ),
 .UNSPECIFIED., .F., .F.,
 ( 4, 2, 4 ),
 ( 0.000000000000000000, 0.5000000000000000000, 1.000000000000000000 ),
 .UNSPECIFIED. ) ;
#18583 = CLOSED_SHELL ( 'NONE', ( #8281, #18399, #3832, #2531, #25465, #20410, #11566, #389, #13331, #9508 ) ) ;
#18584 = CARTESIAN_POINT ( 'NONE',  ( -4.861312627696710464, 6.462009008221268225, -40.63090155203819620 ) ) ;
#18585 = CARTESIAN_POINT ( 'NONE',  ( 14.76350381782003218, -21.99999999999998934, -29.62663954576006020 ) ) ;
#18586 = DIRECTION ( 'NONE',  ( -1.000000000000000000, 0.000000000000000000, 0.000000000000000000 ) ) ;
#18587 = CARTESIAN_POINT ( 'NONE',  ( -17.83931601680000156, 20.00000000000000000, 230.7000111870000012 ) ) ;
#18588 = ORIENTED_EDGE ( 'NONE', *, *, #3819, .F. ) ;
#18589 = ADVANCED_FACE ( 'NONE', ( #2835 ), #798, .F. ) ;
#18590 = CARTESIAN_POINT ( 'NONE',  ( -1.641527485091622385, 5.277626912542655369, -5.774955258300002114 ) ) ;
#18591 = CARTESIAN_POINT ( 'NONE',  ( 3.710789578725101734, 2.835545959904678170, -23.36727430110000014 ) ) ;
#18592 = CARTESIAN_POINT ( 'NONE',  ( -6.336630981016737607, -26.76091511895456776, 208.8270003598715050 ) ) ;
#18593 = CARTESIAN_POINT ( 'NONE',  ( 0.000000000000000000, 0.000000000000000000, 0.000000000000000000 ) ) ;
#18594 = PLANE ( 'NONE',  #29862 ) ;
#18595 = CARTESIAN_POINT ( 'NONE',  ( -25.20441737622035205, 13.30520055017012204, 5.965619087901981921 ) ) ;
#18596 = LINE ( 'NONE', #2082, #14322 ) ;
#18597 = B_SPLINE_CURVE_WITH_KNOTS ( 'NONE', 3,
 ( #28754, #9719, #7362, #19167 ),
 .UNSPECIFIED., .F., .F.,
 ( 4, 4 ),
 ( 0.000000000000000000, 1.000000000000000000 ),
 .UNSPECIFIED. ) ;
#18598 = CARTESIAN_POINT ( 'NONE',  ( 23.77307027441306531, -14.41181805765238444, 4.999998581000003384 ) ) ;
#18599 = CARTESIAN_POINT ( 'NONE',  ( 0.5184513693225644149, -28.49550581263314086, 6.099998581000020792 ) ) ;
#18600 = CARTESIAN_POINT ( 'NONE',  ( -1.598721155459999804E-14, 0.000000000000000000, -0.6999999999999992895 ) ) ;
#18601 = ORIENTED_EDGE ( 'NONE', *, *, #16488, .T. ) ;
#18602 = CARTESIAN_POINT ( 'NONE',  ( 4.508719565894404369, 1.847421675581905953, -60.49141554682498878 ) ) ;
#18603 = CARTESIAN_POINT ( 'NONE',  ( -21.20818545079999851, 16.99505982179999819, 230.0000000000000000 ) ) ;
#18604 = ORIENTED_EDGE ( 'NONE', *, *, #25859, .F. ) ;
#18605 = ORIENTED_EDGE ( 'NONE', *, *, #24494, .F. ) ;
#18606 = CARTESIAN_POINT ( 'NONE',  ( 9.993285220779439371, -25.61999708228226069, 115.0000000000000000 ) ) ;
#18607 = CARTESIAN_POINT ( 'NONE',  ( 4.904813032679735230, 3.691647504909488564, -32.36032172560000930 ) ) ;
#18608 = VERTEX_POINT ( 'NONE', #24864 ) ;
#18609 = CARTESIAN_POINT ( 'NONE',  ( -9.000000000000000000, -54.99999999999998579, -42.39999999999999858 ) ) ;
#18610 = CARTESIAN_POINT ( 'NONE',  ( 20.19076655603537418, -17.71015691556361205, 186.7828584119999675 ) ) ;
#18611 = EDGE_LOOP ( 'NONE', ( #6957, #16075, #11613, #24227 ) ) ;
#18612 = VERTEX_POINT ( 'NONE', #27371 ) ;
#18613 = EDGE_LOOP ( 'NONE', ( #14870, #20069, #24801, #17551, #3600, #29059, #17443, #14945 ) ) ;
#18614 = VERTEX_POINT ( 'NONE', #20282 ) ;
#18615 = CARTESIAN_POINT ( 'NONE',  ( -12.30000000044999986, -30.20000000000000284, -28.40000000001083791 ) ) ;
#18616 = CARTESIAN_POINT ( 'NONE',  ( 23.25354871329972895, -14.68148953537714441, 4.782075050810997041 ) ) ;
#18617 = CARTESIAN_POINT ( 'NONE',  ( -1.084269253894827534, -5.810518403417324507, -67.42745670422499416 ) ) ;
#18618 = EDGE_CURVE ( 'NONE', #7124, #25355, #10236, .T. ) ;
#18619 = CARTESIAN_POINT ( 'NONE',  ( 5.214112608739999821, -30.75012229510000239, 229.4485748759999808 ) ) ;
#18620 = APPLICATION_CONTEXT ( 'automotive_design' ) ;
#18621 = CARTESIAN_POINT ( 'NONE',  ( -9.999999999969999109, -24.00000000000000000, -28.40000000000000213 ) ) ;
#18622 = CARTESIAN_POINT ( 'NONE',  ( 8.000000000860607585, -29.89895010222698701, -27.53380090417111958 ) ) ;
#18623 = DIRECTION ( 'NONE',  ( 0.6941258031311203780, 0.7198537139083029945, 0.000000000000000000 ) ) ;
#18624 = ORIENTED_EDGE ( 'NONE', *, *, #8753, .F. ) ;
#18625 = ADVANCED_FACE ( 'NONE', ( #12430 ), #8010, .F. ) ;
#18626 = CARTESIAN_POINT ( 'NONE',  ( -19.31846164438172053, 19.99998910362869964, -0.3730415779728155634 ) ) ;
#18627 = CARTESIAN_POINT ( 'NONE',  ( 0.7763070146520694159, 4.277613328189615594, -13.52400681850000197 ) ) ;
#18628 = DIRECTION ( 'NONE',  ( 1.000000000000000000, 0.000000000000000000, 0.000000000000000000 ) ) ;
#18629 = CARTESIAN_POINT ( 'NONE',  ( -10.69999999967833659, -26.58048418417539338, -31.59992976938654508 ) ) ;
#18630 = EDGE_LOOP ( 'NONE', ( #6991, #14901, #13422, #8616 ) ) ;
#18631 = DIRECTION ( 'NONE',  ( 0.000000000000000000, 0.000000000000000000, -1.000000000000000000 ) ) ;
#18632 = CARTESIAN_POINT ( 'NONE',  ( -7.999999999975165643, -111.9817663810327275, 5.760339591561383088 ) ) ;
#18633 = CARTESIAN_POINT ( 'NONE',  ( -27.33171861409999792, 5.762471333930000661, 222.0000000000000000 ) ) ;
#18634 = CARTESIAN_POINT ( 'NONE',  ( -5.414213562369999622, -31.28896728272270877, -80.26658230080884948 ) ) ;
#18635 = CARTESIAN_POINT ( 'NONE',  ( 11.09640327169999807, -24.58282405819999994, -1.600739409500000265 ) ) ;
#18636 = CARTESIAN_POINT ( 'NONE',  ( 3.449241269337446791, -4.803451378176493591, -61.52197827312500067 ) ) ;
#18637 = CARTESIAN_POINT ( 'NONE',  ( -23.81569860410000317, -13.75000000000000000, 226.0999999999999943 ) ) ;
#18638 = CARTESIAN_POINT ( 'NONE',  ( 17.16657240420000008, 10.97998838177520931, 0.05106179917585291356 ) ) ;
#18639 = ORIENTED_EDGE ( 'NONE', *, *, #23286, .T. ) ;
#18640 = ADVANCED_FACE ( 'NONE', ( #7703 ), #12716, .T. ) ;
#18641 = CARTESIAN_POINT ( 'NONE',  ( 4.276011752470107119, -42.94729992904354532, -9.547410993441516780 ) ) ;
#18642 = FACE_OUTER_BOUND ( 'NONE', #18777, .T. ) ;
#18643 = CARTESIAN_POINT ( 'NONE',  ( 2.400858303373162528, -3.536441939007071600, -68.10000000002501963 ) ) ;
#18644 = CARTESIAN_POINT ( 'NONE',  ( 2.731088122681216923, 1.619435980086911586, -68.28890305590695675 ) ) ;
#18645 = CARTESIAN_POINT ( 'NONE',  ( -4.245077499289021894, 0.8871105264785797972, -44.10000000002499121 ) ) ;
#18646 = VECTOR ( 'NONE', #28192, 1000.000000000000114 ) ;
#18647 = ORIENTED_EDGE ( 'NONE', *, *, #4639, .F. ) ;
#18648 = CARTESIAN_POINT ( 'NONE',  ( 27.50000000000000000, -3.367667472999999580E-15, 36.71909809219999943 ) ) ;
#18649 = CARTESIAN_POINT ( 'NONE',  ( 4.962532606735698515, 2.397722036449358107, -67.65315453642499222 ) ) ;
#18650 = VERTEX_POINT ( 'NONE', #16038 ) ;
#18651 = CARTESIAN_POINT ( 'NONE',  ( -7.999999999730073696, -28.07052495761531219, -25.59750966829892960 ) ) ;
#18652 = B_SPLINE_CURVE_WITH_KNOTS ( 'NONE', 5,
 ( #23127, #26411, #11924, #4691, #23908, #16954, #9403, #26561, #14610 ),
 .UNSPECIFIED., .F., .F.,
 ( 6, 3, 6 ),
 ( 0.000000000000000000, 0.6978155539409999220, 1.118801870760000039 ),
 .UNSPECIFIED. ) ;
#18653 = CARTESIAN_POINT ( 'NONE',  ( -19.76603762889999771, 19.51852293520000003, 229.2245375310000099 ) ) ;
#18654 = ORIENTED_EDGE ( 'NONE', *, *, #10073, .T. ) ;
#18655 = DIRECTION ( 'NONE',  ( -5.551115123049999208E-18, 0.000000000000000000, -1.000000000000000000 ) ) ;
#18656 = SURFACE_STYLE_FILL_AREA ( #18356 ) ;
#18657 = CARTESIAN_POINT ( 'NONE',  ( 27.92857142860000152, -3.116236426490000064E-16, 42.06031501460000044 ) ) ;
#18658 = CARTESIAN_POINT ( 'NONE',  ( -16.04158851046123502, 10.23646161653652875, -0.6999999999999784173 ) ) ;
#18659 = EDGE_CURVE ( 'NONE', #13152, #18447, #4084, .T. ) ;
#18660 = FACE_OUTER_BOUND ( 'NONE', #4873, .T. ) ;
#18661 = CARTESIAN_POINT ( 'NONE',  ( -7.261438393647745571, 4.106456578431311399, -42.81982768937970718 ) ) ;
#18662 = CARTESIAN_POINT ( 'NONE',  ( 3.043095095529606997, -3.198806979771088077, -95.69213427732501032 ) ) ;
#18663 = ORIENTED_EDGE ( 'NONE', *, *, #1377, .T. ) ;
#18664 = CARTESIAN_POINT ( 'NONE',  ( -27.23548387060000309, 8.881784196999999612E-15, 191.6604601750000256 ) ) ;
#18665 = FACE_OUTER_BOUND ( 'NONE', #10302, .T. ) ;
#18666 = CARTESIAN_POINT ( 'NONE',  ( 2.426970918150000323, 12.02853619149999886, 232.6627643349999914 ) ) ;
#18667 = CARTESIAN_POINT ( 'NONE',  ( -15.97608884582789734, -9.690347176502019266, 0.000000000000000000 ) ) ;
#18668 = CIRCLE ( 'NONE', #27206, 1.000000000000000888 ) ;
#18669 = CARTESIAN_POINT ( 'NONE',  ( 20.97486217528226149, 18.32139343332559989, 4.666666666666781538 ) ) ;
#18670 = CARTESIAN_POINT ( 'NONE',  ( 5.871915332789999553, -10.61013173299999934, 230.6412452697800006 ) ) ;
#18671 = EDGE_CURVE ( 'NONE', #20613, #5639, #14505, .T. ) ;
#18672 = CARTESIAN_POINT ( 'NONE',  ( 12.55799324160000019, 21.70000000000000284, -55.95247857500000066 ) ) ;
#18673 = DIRECTION ( 'NONE',  ( -0.8660254037843290176, -0.5000000000001900702, -0.000000000000000000 ) ) ;
#18674 = CARTESIAN_POINT ( 'NONE',  ( 0.6613659943793989138, -4.850238491497672833, -49.36468436622500633 ) ) ;
#18675 = EDGE_CURVE ( 'NONE', #22953, #18690, #4750, .T. ) ;
#18676 = PLANE ( 'NONE',  #7257 ) ;
#18677 = CARTESIAN_POINT ( 'NONE',  ( 7.393561943475508436, 4.882965509336187004, -39.86075057886888118 ) ) ;
#18678 = CARTESIAN_POINT ( 'NONE',  ( 3.342478061398093114, -1.210236869212865551, 230.8050258245734199 ) ) ;
#18679 = CARTESIAN_POINT ( 'NONE',  ( -24.05715877267779490, -13.32261293328696539, 224.0051167719747696 ) ) ;
#18680 = EDGE_CURVE ( 'NONE', #28330, #6498, #11876, .T. ) ;
#18681 = CARTESIAN_POINT ( 'NONE',  ( -24.10559463919999956, -15.20494734660000091, 224.7915671760000009 ) ) ;
#18682 = EDGE_LOOP ( 'NONE', ( #12851, #28610, #10702, #26011 ) ) ;
#18683 = CARTESIAN_POINT ( 'NONE',  ( 3.357378826396555382, -2.722208303779470651, -55.80923804942499800 ) ) ;
#18684 = VERTEX_POINT ( 'NONE', #23757 ) ;
#18685 = VECTOR ( 'NONE', #11902, 1000.000000000000114 ) ;
#18686 = ORIENTED_EDGE ( 'NONE', *, *, #204, .T. ) ;
#18688 = EDGE_CURVE ( 'NONE', #8808, #8336, #14313, .T. ) ;
#18687 = DIRECTION ( 'NONE',  ( 1.000000000000000000, 4.445489947300000020E-24, -2.257150022439999944E-12 ) ) ;
#18689 = PRODUCT_DEFINITION_SHAPE ( 'NONE', 'NONE',  #4652 ) ;
#18690 = VERTEX_POINT ( 'NONE', #2353 ) ;
#18691 = CARTESIAN_POINT ( 'NONE',  ( 14.74466352505200284, -28.32694284507041260, -23.39287652031412179 ) ) ;
#18692 = CARTESIAN_POINT ( 'NONE',  ( -2.486939662212003466, -15.93335509046200826, -109.1271631200378351 ) ) ;
#18693 = DIRECTION ( 'NONE',  ( 0.000000000000000000, 0.000000000000000000, 1.000000000000000000 ) ) ;
#18694 = EDGE_CURVE ( 'NONE', #30938, #21756, #8116, .T. ) ;
#18695 = B_SPLINE_CURVE_WITH_KNOTS ( 'NONE', 5,
 ( #30518, #28614, #7053, #28145, #30820, #1720 ),
 .UNSPECIFIED., .F., .F.,
 ( 6, 6 ),
 ( 0.000000000000000000, 1.000000000000000000 ),
 .UNSPECIFIED. ) ;
#18696 = EDGE_LOOP ( 'NONE', ( #25550, #789, #31033, #17821 ) ) ;
#18697 = CARTESIAN_POINT ( 'NONE',  ( -5.208546124329999749, -11.06211866609999994, 232.6627648150000027 ) ) ;
#18698 = CARTESIAN_POINT ( 'NONE',  ( -27.24406355354269849, -0.4957164003159654775, 0.08279779300002232389 ) ) ;
#18699 = CARTESIAN_POINT ( 'NONE',  ( 7.105427357599999217E-15, 0.000000000000000000, 136.3944487250000179 ) ) ;
#18700 = CARTESIAN_POINT ( 'NONE',  ( -1.295942751353772238, 4.166547562507297187, -4.774955258300003891 ) ) ;
#18701 = CARTESIAN_POINT ( 'NONE',  ( -13.37464065170000005, -26.85454942340000173, 230.6999999999999886 ) ) ;
#18702 = VERTEX_POINT ( 'NONE', #14465 ) ;
#18703 = CARTESIAN_POINT ( 'NONE',  ( 24.84442124000000263, 12.90866478800000117, 222.0000000000000000 ) ) ;
#18704 = EDGE_CURVE ( 'NONE', #5036, #5533, #16750, .T. ) ;
#18705 = CARTESIAN_POINT ( 'NONE',  ( 5.782996427689181651, 1.709881257618839356, -17.54190840230000603 ) ) ;
#18706 = CARTESIAN_POINT ( 'NONE',  ( 6.760007715859398303, 5.672256964398498802, -40.24571374337934770 ) ) ;
#18707 = VECTOR ( 'NONE', #18631, 1000.000000000000000 ) ;
#18708 = CARTESIAN_POINT ( 'NONE',  ( 27.21667690494597380, -9.441116152978883846, -0.6999999999999784173 ) ) ;
#18709 = CARTESIAN_POINT ( 'NONE',  ( 1.087695520339999833, -27.77888045939999984, 224.7918990269999995 ) ) ;
#18710 = CARTESIAN_POINT ( 'NONE',  ( 26.38956582071493528, -11.43351142516159058, 8.000000000000007105 ) ) ;
#18711 = CARTESIAN_POINT ( 'NONE',  ( 7.013234437640000065E-10, 20.99999999999999645, -60.10000000000000142 ) ) ;
#18712 = B_SPLINE_SURFACE_WITH_KNOTS ( 'NONE', 5, 1, ( 
 ( #2228, #14802 ),
 ( #14652, #26752 ),
 ( #14498, #24094 ),
 ( #17001, #26913 ),
 ( #2834, #26604 ),
 ( #29112, #9763 ),
 ( #9610, #5043 ),
 ( #21425, #179 ),
 ( #12429, #26293 ),
 ( #19209, #24237 ),
 ( #28793, #7251 ),
 ( #16683, #28959 ),
 ( #2533, #22046 ),
 ( #2682, #21894 ),
 ( #9924, #12120 ) ),
 .UNSPECIFIED., .F., .F., .F.,
 ( 6, 3, 3, 3, 6 ),
 ( 2, 2 ),
 ( 0.000000000000000000, 0.5239055191900000574, 1.047811038380000115, 1.571716557570000061, 1.746351730630000043 ),
 ( -0.7000000000009999335, 2.557307477669999647E-06 ),
 .UNSPECIFIED. ) ;
#18713 = CARTESIAN_POINT ( 'NONE',  ( 26.20132165689940962, 9.485175511428851181, -0.6577119969999878357 ) ) ;
#18714 = DIRECTION ( 'NONE',  ( -1.000000000000000000, 0.000000000000000000, 0.000000000000000000 ) ) ;
#18715 = LINE ( 'NONE', #6602, #15806 ) ;
#18716 = CARTESIAN_POINT ( 'NONE',  ( -27.69999999930000101, 3.392159599999999562E-15, 140.0000000000000000 ) ) ;
#18717 = VERTEX_POINT ( 'NONE', #2503 ) ;
#18718 = CYLINDRICAL_SURFACE ( 'NONE', #30342, 2.100000000000000977 ) ;
#18719 =( NAMED_UNIT ( * ) PLANE_ANGLE_UNIT ( ) SI_UNIT ( $, .RADIAN. ) );
#18720 = LINE ( 'NONE', #6306, #18083 ) ;
#18721 = ORIENTED_EDGE ( 'NONE', *, *, #15572, .T. ) ;
#18722 = CARTESIAN_POINT ( 'NONE',  ( 4.248246898893026646, -2.821772188863608921, -43.35875473022499449 ) ) ;
#18723 = ORIENTED_EDGE ( 'NONE', *, *, #6705, .T. ) ;
#18724 = EDGE_LOOP ( 'NONE', ( #13860, #30150, #3950, #17253, #8334 ) ) ;
#18725 = ORIENTED_EDGE ( 'NONE', *, *, #8484, .F. ) ;
#18726 = CARTESIAN_POINT ( 'NONE',  ( 3.540054785840129892, -1.372664319004998745, -35.69999999999999574 ) ) ;
#18727 = EDGE_CURVE ( 'NONE', #15436, #31086, #9889, .T. ) ;
#18728 = VERTEX_POINT ( 'NONE', #21229 ) ;
#18729 = AXIS2_PLACEMENT_3D ( 'NONE', #26463, #16395, #4906 ) ;
#18730 = CARTESIAN_POINT ( 'NONE',  ( 27.69999999930000101, -3.392159599989999961E-15, 40.00000000000000000 ) ) ;
#18731 = CARTESIAN_POINT ( 'NONE',  ( 23.81776757409229361, 15.65134803726813217, 4.895813257000003915 ) ) ;
#18732 = CARTESIAN_POINT ( 'NONE',  ( -24.40022624598054435, -14.72688605908970239, 3.899998581000013509 ) ) ;
#18733 = CARTESIAN_POINT ( 'NONE',  ( 1.914928416346060702, 3.478121177954408783, -35.69999999999998863 ) ) ;
#18734 = ADVANCED_FACE ( 'NONE', ( #2649 ), #2655, .F. ) ;
#18735 = EDGE_CURVE ( 'NONE', #4103, #19446, #23223, .T. ) ;
#18736 = CARTESIAN_POINT ( 'NONE',  ( 8.700000000278567569, -14.35781456214690266, -33.57689241567665306 ) ) ;
#18737 = EDGE_CURVE ( 'NONE', #20099, #12344, #25023, .T. ) ;
#18738 = CARTESIAN_POINT ( 'NONE',  ( 18.09234735182029041, -19.80227287648861889, -1.399999999999998579 ) ) ;
#18739 = CARTESIAN_POINT ( 'NONE',  ( -15.86808677770000209, 10.47263190749999495, -0.7000000003999986564 ) ) ;
#18740 = CARTESIAN_POINT ( 'NONE',  ( -19.65706407100000064, 20.00000595720000263, 230.1821686570000054 ) ) ;
#18741 = EDGE_LOOP ( 'NONE', ( #6680, #19082, #25395, #10108 ) ) ;
#18742 = CARTESIAN_POINT ( 'NONE',  ( -1.425537026491585868, 4.583202318768851313, -5.712455258300007443 ) ) ;
#18743 = CARTESIAN_POINT ( 'NONE',  ( -4.856400125594941386, 3.359828160699422472, -24.46779765530000361 ) ) ;
#18744 = DIRECTION ( 'NONE',  ( 0.000000000000000000, 0.000000000000000000, 1.000000000000000000 ) ) ;
#18745 = CARTESIAN_POINT ( 'NONE',  ( -23.48238834522544494, -12.91648733505556201, 224.0393715185676626 ) ) ;
#18746 = DIRECTION ( 'NONE',  ( 1.000000000000000000, 0.000000000000000000, 0.000000000000000000 ) ) ;
#18747 = CARTESIAN_POINT ( 'NONE',  ( -2.646164081324360762, -21.74690406887915728, -30.21030117774004964 ) ) ;
#18748 = CARTESIAN_POINT ( 'NONE',  ( -23.50695179570000093, -14.84192241259999889, 225.0000014190000002 ) ) ;
#18749 = CIRCLE ( 'NONE', #2182, 4.276011752367109509 ) ;
#18750 = STYLED_ITEM ( 'NONE', ( #1200 ), #14437 ) ;
#18751 = CARTESIAN_POINT ( 'NONE',  ( 0.000000000000000000, 0.000000000000000000, 86.39444872359999295 ) ) ;
#18752 = CARTESIAN_POINT ( 'NONE',  ( 0.5890437901237028928, -28.49417040867362516, 6.098651075000017130 ) ) ;
#18753 = CARTESIAN_POINT ( 'NONE',  ( -17.91041692047024370, 11.26717219323752062, -0.6999999999999784173 ) ) ;
#18754 = EDGE_LOOP ( 'NONE', ( #8846, #30710, #29874, #16242 ) ) ;
#18755 = CARTESIAN_POINT ( 'NONE',  ( 1.387947292976102087, 4.364053279572885025, -60.46492395752500215 ) ) ;
#18756 = AXIS2_PLACEMENT_3D ( 'NONE', #811, #24569, #7568 ) ;
#18757 = CARTESIAN_POINT ( 'NONE',  ( -27.71720220719999972, 4.673546953369999812, 229.4485730569999760 ) ) ;
#18758 = DIRECTION ( 'NONE',  ( -3.924189347185962345E-12, 0.4082287037029531107, 0.9128796883888953273 ) ) ;
#18759 = CARTESIAN_POINT ( 'NONE',  ( -3.251750336246070461, -5.089746299513510763, -21.70891267860000795 ) ) ;
#18760 = ORIENTED_EDGE ( 'NONE', *, *, #22641, .F. ) ;
#18761 = CARTESIAN_POINT ( 'NONE',  ( 26.80000000069999899, -3.281945028320000125E-15, 165.0000000000000000 ) ) ;
#18762 = CARTESIAN_POINT ( 'NONE',  ( 21.17691543559999801, 18.05241775060000009, 224.9999999359999947 ) ) ;
#18763 = VERTEX_POINT ( 'NONE', #2808 ) ;
#18764 = EDGE_LOOP ( 'NONE', ( #7082, #28132, #15054, #9989 ) ) ;
#18765 = VERTEX_POINT ( 'NONE', #12400 ) ;
#18766 =( NAMED_UNIT ( * ) SI_UNIT ( $, .STERADIAN. ) SOLID_ANGLE_UNIT ( ) );
#18767 = VERTEX_POINT ( 'NONE', #10511 ) ;
#18768 = CARTESIAN_POINT ( 'NONE',  ( -8.699999999642283655, -16.96959321760381556, -37.81493174590716677 ) ) ;
#18769 = DIRECTION ( 'NONE',  ( 0.000000000000000000, -1.000000000000000000, 0.000000000000000000 ) ) ;
#18771 = CARTESIAN_POINT ( 'NONE',  ( 4.782773383987898974, -2.143867810222768178, -66.52841551492500116 ) ) ;
#18770 = VECTOR ( 'NONE', #9741, 1000.000000000000000 ) ;
#18772 = CARTESIAN_POINT ( 'NONE',  ( 20.64716981389999972, -20.77933506589999979, 229.0000000020000073 ) ) ;
#18773 = AXIS2_PLACEMENT_3D ( 'NONE', #18172, #6220, #13458 ) ;
#18774 = DIRECTION ( 'NONE',  ( 2.764840495839172514E-12, 0.9128796883888952163, -0.4082287037029530552 ) ) ;
#18775 = CARTESIAN_POINT ( 'NONE',  ( 17.16657240421717390, -9.000000000001264766, -0.6999999999999784173 ) ) ;
#18776 = CARTESIAN_POINT ( 'NONE',  ( 5.131765537970109037, -1.193580270428616696, -35.69999999999999574 ) ) ;
#18777 = EDGE_LOOP ( 'NONE', ( #8537, #11145, #2349, #28045 ) ) ;
#18778 = CARTESIAN_POINT ( 'NONE',  ( -18.58704431631444010, 19.99991904899251338, -0.6240947616942604803 ) ) ;
#18779 = CARTESIAN_POINT ( 'NONE',  ( 0.9833222185976336904, 5.418310215658684648, -13.02400681849999842 ) ) ;
#18780 = CARTESIAN_POINT ( 'NONE',  ( 24.08627744698562267, -11.88207008772947049, 0.000000000000000000 ) ) ;
#18781 = CARTESIAN_POINT ( 'NONE',  ( 12.32633748798225071, -0.2818134555603850622, 232.6627636236952412 ) ) ;
#18782 = ORIENTED_EDGE ( 'NONE', *, *, #20537, .F. ) ;
#18783 = FACE_OUTER_BOUND ( 'NONE', #13382, .T. ) ;
#18784 = CARTESIAN_POINT ( 'NONE',  ( -10.69999999999999929, -129.6759735804000115, -38.47487552122000665 ) ) ;
#18785 = CARTESIAN_POINT ( 'NONE',  ( 0.000000000000000000, 0.000000000000000000, 115.0000000000000000 ) ) ;
#18786 = CARTESIAN_POINT ( 'NONE',  ( 0.6686231747779999290, -28.49266848160000265, 225.9009072510000067 ) ) ;
#18787 = CARTESIAN_POINT ( 'NONE',  ( -13.15654851664530511, 20.99999999997228528, -56.37844548362021868 ) ) ;
#18788 = LINE ( 'NONE', #24142, #29779 ) ;
#18789 = DIRECTION ( 'NONE',  ( 0.000000000000000000, -0.9128796883888953273, 0.4082287037029528332 ) ) ;
#18790 = CARTESIAN_POINT ( 'NONE',  ( 8.000000000247633025, -27.86541989009443654, -31.29929855349184464 ) ) ;
#18791 = VECTOR ( 'NONE', #29509, 999.9999999999998863 ) ;
#18792 = ORIENTED_EDGE ( 'NONE', *, *, #4926, .T. ) ;
#18793 = EDGE_CURVE ( 'NONE', #23982, #4159, #19189, .T. ) ;
#18794 = LINE ( 'NONE', #31073, #13787 ) ;
#18795 = DIRECTION ( 'NONE',  ( 0.7071067811865475727, -0.6644630243886071597, -0.2418447626481610435 ) ) ;
#18796 = AXIS2_PLACEMENT_3D ( 'NONE', #29510, #7947, #17691 ) ;
#18797 = AXIS2_PLACEMENT_3D ( 'NONE', #26992, #27148, #17230 ) ;
#18798 = CARTESIAN_POINT ( 'NONE',  ( 2.608536516501943403, -3.962017450064297286, -68.10000000002500542 ) ) ;
#18799 = EDGE_CURVE ( 'NONE', #8301, #16868, #25761, .T. ) ;
#18800 = LINE ( 'NONE', #30466, #12234 ) ;
#18801 = CARTESIAN_POINT ( 'NONE',  ( 24.49999999470000134, -3.000285566199999922E-15, 89.99999999930000172 ) ) ;
#18802 = ORIENTED_EDGE ( 'NONE', *, *, #17436, .F. ) ;
#18803 = CARTESIAN_POINT ( 'NONE',  ( 0.2818134420171679588, 12.32633706535993312, 232.6627637660202197 ) ) ;
#18804 = COLOUR_RGB ( '', 0.08235294, 0.09019608, 0.10196078) ;
#18805 = CARTESIAN_POINT ( 'NONE',  ( 2.917330641183085049, 3.968100254485465328, -67.39226422542500927 ) ) ;
#18806 = ORIENTED_EDGE ( 'NONE', *, *, #28306, .T. ) ;
#18807 = DIRECTION ( 'NONE',  ( -1.000000000000000000, 0.000000000000000000, 0.000000000000000000 ) ) ;
#18808 = CARTESIAN_POINT ( 'NONE',  ( -26.93696268452645981, -0.4901285798020263984, 0.000000000000000000 ) ) ;
#18809 = ORIENTED_EDGE ( 'NONE', *, *, #9098, .F. ) ;
#18811 = DIRECTION ( 'NONE',  ( 1.000000000000000000, 0.000000000000000000, 0.000000000000000000 ) ) ;
#18810 = CIRCLE ( 'NONE', #23349, 26.80000000000000071 ) ;
#18812 = B_SPLINE_CURVE_WITH_KNOTS ( 'NONE', 3,
 ( #21316, #4485, #19264, #30919 ),
 .UNSPECIFIED., .F., .F.,
 ( 4, 4 ),
 ( 0.000000000000000000, 1.000000000000000000 ),
 .UNSPECIFIED. ) ;
#18813 = AXIS2_PLACEMENT_3D ( 'NONE', #1700, #18376, #6720 ) ;
#18814 = FILL_AREA_STYLE_COLOUR ( '', #12045 ) ;
#18815 = CARTESIAN_POINT ( 'NONE',  ( 9.998463852539998697, 19.99999999999999645, -42.46069674353999801 ) ) ;
#18816 = UNCERTAINTY_MEASURE_WITH_UNIT (LENGTH_MEASURE( 1.000000000000000082E-05 ), #26854, 'distance_accuracy_value', 'NONE');
#18817 = VECTOR ( 'NONE', #9816, 1000.000000000000000 ) ;
#18818 = DIRECTION ( 'NONE',  ( -6.326189572192214457E-12, -0.3568421334038989756, 0.9341647027306019258 ) ) ;
#18819 = DIRECTION ( 'NONE',  ( 0.000000000000000000, 0.000000000000000000, 1.000000000000000000 ) ) ;
#18820 = CARTESIAN_POINT ( 'NONE',  ( 0.000000000000000000, 5.495185456771864096, -69.00660115587162124 ) ) ;
#18821 = EDGE_CURVE ( 'NONE', #10703, #12816, #22470, .T. ) ;
#18822 = ORIENTED_EDGE ( 'NONE', *, *, #29259, .F. ) ;
#18823 = FACE_OUTER_BOUND ( 'NONE', #14171, .T. ) ;
#18824 = CARTESIAN_POINT ( 'NONE',  ( 10.69999999999999929, -29.06671945340000107, -26.22544931050000017 ) ) ;
#18825 = DIRECTION ( 'NONE',  ( 0.000000000000000000, 1.000000000000000000, 0.000000000000000000 ) ) ;
#18826 = B_SPLINE_CURVE_WITH_KNOTS ( 'NONE', 3,
 ( #21846, #17107, #19166, #21998, #28611, #19326 ),
 .UNSPECIFIED., .F., .F.,
 ( 4, 2, 4 ),
 ( 0.000000000000000000, 0.5000000000000000000, 1.000000000000000000 ),
 .UNSPECIFIED. ) ;
#18827 = CARTESIAN_POINT ( 'NONE',  ( -22.83911268609999823, 16.42879705520000044, 223.3999999999999773 ) ) ;
#18828 = DIRECTION ( 'NONE',  ( -2.537652630420000242E-15, 0.000000000000000000, 1.000000000000000000 ) ) ;
#18829 = CARTESIAN_POINT ( 'NONE',  ( 12.09628639090000135, 1.465387503880000164, 230.6412452697800006 ) ) ;
#18830 = VECTOR ( 'NONE', #16115, 1000.000000000000114 ) ;
#18831 = MECHANICAL_DESIGN_GEOMETRIC_PRESENTATION_REPRESENTATION (  '', ( #25377 ), #22855 ) ;
#18832 = CARTESIAN_POINT ( 'NONE',  ( -25.16696685483287155, 13.37570800105703306, 3.997190761000024573 ) ) ;
#18833 = CARTESIAN_POINT ( 'NONE',  ( 4.276011752472853367, -43.23306002163561601, -10.18642677531374829 ) ) ;
#18834 = CARTESIAN_POINT ( 'NONE',  ( -3.221934060409652023, 3.671197199744479001, -53.98587006832499924 ) ) ;
#18835 = CARTESIAN_POINT ( 'NONE',  ( 24.83827260360999389, -12.48687744688666967, 4.999998581000003384 ) ) ;
#18836 = CARTESIAN_POINT ( 'NONE',  ( -27.24857305730000334, -4.411353757410000576E-12, 229.9172022069999741 ) ) ;
#18837 = CARTESIAN_POINT ( 'NONE',  ( -16.81341597756113515, 9.900182044522454206, -1.000005633855494125E-09 ) ) ;
#18838 = ORIENTED_EDGE ( 'NONE', *, *, #14126, .T. ) ;
#18839 = AXIS2_PLACEMENT_3D ( 'NONE', #23850, #9983, #31077 ) ;
#18840 = EDGE_CURVE ( 'NONE', #55, #13075, #630, .T. ) ;
#18841 = CARTESIAN_POINT ( 'NONE',  ( -0.09666810103353495887, -27.50000000000000711, 223.9000000000000057 ) ) ;
#18842 = DIRECTION ( 'NONE',  ( 1.000000000000000000, 0.000000000000000000, 0.000000000000000000 ) ) ;
#18843 = CARTESIAN_POINT ( 'NONE',  ( 4.046071919042645959, -3.280610007112897186, -56.20923804942499657 ) ) ;
#18844 = ORIENTED_EDGE ( 'NONE', *, *, #25496, .F. ) ;
#18845 = CONTEXT_DEPENDENT_SHAPE_REPRESENTATION ( #8779, #16745 ) ;
#18846 = COLOUR_RGB ( '', 0.09019608, 0.27058824, 0.51372549) ;
#18847 = ORIENTED_EDGE ( 'NONE', *, *, #23193, .T. ) ;
#18848 = CARTESIAN_POINT ( 'NONE',  ( -17.48838570233685275, -29.74446036096981771, -32.58900154053760900 ) ) ;
#18849 = ORIENTED_EDGE ( 'NONE', *, *, #1024, .F. ) ;
#18850 = CONICAL_SURFACE ( 'NONE', #5294, 0.9999999999991034949, 0.7853981633970000820 ) ;
#18851 = COLOUR_RGB ( '', 0.66274510, 0.83137255, 0.94901961) ;
#18852 = EDGE_CURVE ( 'NONE', #24939, #12916, #29218, .T. ) ;
#18853 = CARTESIAN_POINT ( 'NONE',  ( 14.74203063447538753, -28.31189348597844102, -23.38419426985683813 ) ) ;
#18854 = DIRECTION ( 'NONE',  ( 0.1090476345695675503, 0.6986477033489619792, 0.7071067811865496822 ) ) ;
#18855 = CARTESIAN_POINT ( 'NONE',  ( -25.38146355688813216, 12.59839640969179975, 2.400000000000013234 ) ) ;
#18856 = EDGE_CURVE ( 'NONE', #11023, #20745, #6242, .T. ) ;
#18857 = DIRECTION ( 'NONE',  ( 0.000000000000000000, 1.000000000000000000, 0.000000000000000000 ) ) ;
#18858 = CARTESIAN_POINT ( 'NONE',  ( -25.14597776469364732, -15.02549348228339454, 8.000000000000007105 ) ) ;
#18859 = CARTESIAN_POINT ( 'NONE',  ( -16.06988921231594603, 11.79183908526949054, 0.000000000000000000 ) ) ;
#18860 = CARTESIAN_POINT ( 'NONE',  ( -3.052679639724403593, 3.117809041995149411, -4.068732180600004078 ) ) ;
#18861 = CARTESIAN_POINT ( 'NONE',  ( -28.04325408079999704, -10.30313394320000064, 230.2432540810000319 ) ) ;
#18862 = EDGE_LOOP ( 'NONE', ( #7548, #21784, #12639, #22135 ) ) ;
#18863 = FACE_OUTER_BOUND ( 'NONE', #20106, .T. ) ;
#18864 = EDGE_CURVE ( 'NONE', #27730, #1828, #30268, .T. ) ;
#18865 = CARTESIAN_POINT ( 'NONE',  ( 5.320018516182488000, -2.211191048809329374, -17.87122516810000405 ) ) ;
#18866 = CARTESIAN_POINT ( 'NONE',  ( 24.31044119090657318, 13.69178363021313949, 8.000000000000007105 ) ) ;
#18867 = CARTESIAN_POINT ( 'NONE',  ( 24.83827260360999389, -12.48687744688666967, 4.999998581000003384 ) ) ;
#18868 = CARTESIAN_POINT ( 'NONE',  ( 22.63260994176697238, -19.28417101125922883, -0.6999999999999784173 ) ) ;
#18869 = CARTESIAN_POINT ( 'NONE',  ( -24.50074272580000212, -13.13701158840000005, 224.3191686030000369 ) ) ;
#18870 = CARTESIAN_POINT ( 'NONE',  ( -7.999999999635500458, -22.00621177641532000, -40.24039824850300562 ) ) ;
#18871 = CARTESIAN_POINT ( 'NONE',  ( -4.592700181227117540, -1.655560342997611123, -44.01497819512500342 ) ) ;
#18872 = B_SPLINE_CURVE_WITH_KNOTS ( 'NONE', 1,
 ( #30488, #28423 ),
 .UNSPECIFIED., .F., .F.,
 ( 2, 2 ),
 ( -0.7017616274569999923, 4.107825191113079200E-15 ),
 .UNSPECIFIED. ) ;
#18873 = PLANE ( 'NONE',  #1671 ) ;
#18874 = CARTESIAN_POINT ( 'NONE',  ( 1.270718008852894654, -3.293366139498758560, 226.6412452697750268 ) ) ;
#18875 = CYLINDRICAL_SURFACE ( 'NONE', #20314, 1.100000000000000089 ) ;
#18876 = EDGE_CURVE ( 'NONE', #29870, #11243, #15655, .T. ) ;
#18877 = PRODUCT_DEFINITION_FORMATION_WITH_SPECIFIED_SOURCE ( 'ANY', '', #13934, .NOT_KNOWN. ) ;
#18878 = CARTESIAN_POINT ( 'NONE',  ( -24.83827471527357744, 12.48687850854618198, 4.999998581000003384 ) ) ;
#18879 = ORIENTED_EDGE ( 'NONE', *, *, #20119, .T. ) ;
#18880 = FACE_OUTER_BOUND ( 'NONE', #10533, .T. ) ;
#18881 = DIRECTION ( 'NONE',  ( 0.000000000000000000, 2.257157423930000049E-12, 1.000000000000000000 ) ) ;
#18882 =( LENGTH_UNIT ( ) NAMED_UNIT ( * ) SI_UNIT ( .MILLI., .METRE. ) );
#18883 = FACE_OUTER_BOUND ( 'NONE', #20213, .T. ) ;
#18884 = ORIENTED_EDGE ( 'NONE', *, *, #5232, .F. ) ;
#18885 = CARTESIAN_POINT ( 'NONE',  ( -4.757978549728680839, 2.797812790916673897, -45.64354844312499893 ) ) ;
#18886 = ORIENTED_EDGE ( 'NONE', *, *, #2018, .F. ) ;
#18887 = EDGE_CURVE ( 'NONE', #565, #22567, #11133, .T. ) ;
#18888 = ORIENTED_EDGE ( 'NONE', *, *, #19533, .T. ) ;
#18889 = CARTESIAN_POINT ( 'NONE',  ( 0.000000000000000000, 0.000000000000000000, 0.000000000000000000 ) ) ;
#18890 = B_SPLINE_CURVE_WITH_KNOTS ( 'NONE', 3,
 ( #16544, #4125, #30568, #18595, #6949, #14193, #23796, #6635, #2243, #8676, #16233, #9779 ),
 .UNSPECIFIED., .F., .F.,
 ( 4, 2, 2, 2, 2, 4 ),
 ( 0.000000000000000000, 0.2500000000000008882, 0.5000000000000017764, 0.6250000000000016653, 0.7500000000000015543, 1.000000000000000000 ),
 .UNSPECIFIED. ) ;
#18891 = ORIENTED_EDGE ( 'NONE', *, *, #24110, .F. ) ;
#18892 = CARTESIAN_POINT ( 'NONE',  ( -0.4702726640079999965, -27.79650200060000031, 223.9974845609999932 ) ) ;
#18893 = EDGE_LOOP ( 'NONE', ( #14936, #23625, #10877, #27198 ) ) ;
#18894 = CARTESIAN_POINT ( 'NONE',  ( 27.98121187870611593, -9.706323496128696604, 1.000000000000000888 ) ) ;
#18895 = CARTESIAN_POINT ( 'NONE',  ( 9.999999999939999995, -25.00000000000000000, -16.71944709739999979 ) ) ;
#18896 = CARTESIAN_POINT ( 'NONE',  ( 1.388368458387652105, 3.811721462276582706, -35.69999999999999574 ) ) ;
#18897 = CARTESIAN_POINT ( 'NONE',  ( 19.98778790343742529, 20.00007856030388353, 0.1551495369530143942 ) ) ;
#18898 = CARTESIAN_POINT ( 'NONE',  ( 15.51202505004052057, -21.88245214056498611, -1.399999999999998357 ) ) ;
#18899 = CARTESIAN_POINT ( 'NONE',  ( -6.630653307694315046, -7.257150041126550377, -33.93962059595295955 ) ) ;
#18900 = CARTESIAN_POINT ( 'NONE',  ( 17.85846454799866834, -9.867189877967701861, -4.336808689942017736E-16 ) ) ;
#18901 = CARTESIAN_POINT ( 'NONE',  ( 4.781918068392163157, 0.6270375808061986467, -6.564479598400001059 ) ) ;
#18902 = CARTESIAN_POINT ( 'NONE',  ( 2.499950477468926291, 3.566222500441432075, -29.21106724380000230 ) ) ;
#18903 = DIRECTION ( 'NONE',  ( 0.000000000000000000, 0.000000000000000000, -1.000000000000000000 ) ) ;
#18904 = CARTESIAN_POINT ( 'NONE',  ( -3.542914729026271914, -0.003443490030646811917, -88.52261276311425320 ) ) ;
#18905 = CARTESIAN_POINT ( 'NONE',  ( -1.380865576431546504, 3.499743769987727404, 227.7972036410087640 ) ) ;
#18906 = CARTESIAN_POINT ( 'NONE',  ( -26.30711198659999894, 9.878896915450001259, 222.0000000000000000 ) ) ;
#18907 = CARTESIAN_POINT ( 'NONE',  ( 3.904508939291361003, -1.994718106397497914, -11.91474735220000092 ) ) ;
#18908 = CARTESIAN_POINT ( 'NONE',  ( -20.30403093128963476, 20.00000000003735323, 3.000000106999994642 ) ) ;
#18909 = DIRECTION ( 'NONE',  ( 0.000000000000000000, 0.4794255386042040601, 0.8775825618903722036 ) ) ;
#18910 = CARTESIAN_POINT ( 'NONE',  ( -24.04002993240373698, -11.89710236790277520, -1.399999999999998579 ) ) ;
#18911 = EDGE_CURVE ( 'NONE', #11807, #13075, #22738, .T. ) ;
#18912 = ORIENTED_EDGE ( 'NONE', *, *, #21391, .T. ) ;
#18913 = CARTESIAN_POINT ( 'NONE',  ( -24.37165444408190851, 14.77472139917419369, 4.999998581000003384 ) ) ;
#18914 = ORIENTED_EDGE ( 'NONE', *, *, #18050, .F. ) ;
#18915 = ADVANCED_FACE ( 'NONE', ( #20567 ), #23418, .T. ) ;
#18916 = DIRECTION ( 'NONE',  ( -9.216661250624602488E-13, -0.9128796883888954383, 0.4082287037029530552 ) ) ;
#18917 = CARTESIAN_POINT ( 'NONE',  ( -2.496099253731141943, 5.577352528212363048, -22.73780126169999605 ) ) ;
#18918 = ORIENTED_EDGE ( 'NONE', *, *, #16401, .F. ) ;
#18919 = ADVANCED_FACE ( 'NONE', ( #30164 ), #8597, .F. ) ;
#18920 = DIRECTION ( 'NONE',  ( 0.000000000000000000, 0.7113488923935485930, -0.7028390664230835805 ) ) ;
#18921 = CARTESIAN_POINT ( 'NONE',  ( 21.71012070049999920, 18.50699920749999805, 224.9999999359999947 ) ) ;
#18922 = ORIENTED_EDGE ( 'NONE', *, *, #20540, .T. ) ;
#18923 = ORIENTED_EDGE ( 'NONE', *, *, #15135, .T. ) ;
#18924 = ORIENTED_EDGE ( 'NONE', *, *, #14258, .T. ) ;
#18925 =( LENGTH_UNIT ( ) NAMED_UNIT ( * ) SI_UNIT ( .MILLI., .METRE. ) );
#18926 = ORIENTED_EDGE ( 'NONE', *, *, #1972, .T. ) ;
#18927 = CARTESIAN_POINT ( 'NONE',  ( -17.49999999969999465, -27.78076054102322345, -31.32371301078582704 ) ) ;
#18928 = CARTESIAN_POINT ( 'NONE',  ( -9.993285220779425160, -25.61999708228226069, 115.0000000000000000 ) ) ;
#18929 = CARTESIAN_POINT ( 'NONE',  ( 2.708949881112997282, 3.684664522020660193, -66.64226422532500749 ) ) ;
#18930 = CARTESIAN_POINT ( 'NONE',  ( 5.179147464839999770, -30.54390743120000096, 229.7313277700000071 ) ) ;
#18931 = B_SPLINE_CURVE_WITH_KNOTS ( 'NONE', 3,
 ( #27408, #5846, #15449, #30, #19212, #6940 ),
 .UNSPECIFIED., .F., .F.,
 ( 4, 2, 4 ),
 ( 0.000000000000000000, 0.5000000000000002220, 1.000000000000000000 ),
 .UNSPECIFIED. ) ;
#18932 = DIRECTION ( 'NONE',  ( -1.000000000000000000, 5.063197998645201881E-16, -2.257212216166322864E-12 ) ) ;
#18933 = CARTESIAN_POINT ( 'NONE',  ( 23.46242932110000012, -15.37847435530000162, 222.0000000000000000 ) ) ;
#18934 = CARTESIAN_POINT ( 'NONE',  ( 5.213923276575050281, -0.6319207471432233270, -35.69999999999999574 ) ) ;
#18935 = ORIENTED_EDGE ( 'NONE', *, *, #17643, .F. ) ;
#18936 = CARTESIAN_POINT ( 'NONE',  ( -20.28349499515899268, 20.00041701855139564, 0.7434420671224396537 ) ) ;
#18937 = VECTOR ( 'NONE', #256, 999.9999999999998863 ) ;
#18938 = CARTESIAN_POINT ( 'NONE',  ( 4.315341029122434335, -4.279276102762477940, -15.06112212870000455 ) ) ;
#18939 = CARTESIAN_POINT ( 'NONE',  ( -7.999999999650066584, -15.36103638014619222, -37.97055538590272761 ) ) ;
#18940 = CARTESIAN_POINT ( 'NONE',  ( -10.69999999969433446, -23.88311731680927608, -29.23695679439294537 ) ) ;
#18941 = ORIENTED_EDGE ( 'NONE', *, *, #27247, .F. ) ;
#18942 = CARTESIAN_POINT ( 'NONE',  ( -23.23277431135011994, -15.26692929364048013, 4.853020674800981205 ) ) ;
#18943 = CARTESIAN_POINT ( 'NONE',  ( 0.7646642646963620615, -28.49022165133369455, 3.920206710000012862 ) ) ;
#18944 = CARTESIAN_POINT ( 'NONE',  ( -23.66805819309999848, 15.87731454680000098, 222.0000000000000000 ) ) ;
#18945 = B_SPLINE_CURVE_WITH_KNOTS ( 'NONE', 3,
 ( #4554, #21866, #10054, #19181, #24212, #4706 ),
 .UNSPECIFIED., .F., .F.,
 ( 4, 2, 4 ),
 ( 0.000000000000000000, 0.5000000000000000000, 1.000000000000000000 ),
 .UNSPECIFIED. ) ;
#18946 = CARTESIAN_POINT ( 'NONE',  ( 7.999999999489548763, -115.5267901939644446, 21.04701626999689168 ) ) ;
#18947 = B_SPLINE_CURVE_WITH_KNOTS ( 'NONE', 3,
 ( #11142, #4369, #18206, #28281 ),
 .UNSPECIFIED., .F., .F.,
 ( 4, 4 ),
 ( 0.000000000000000000, 1.000000000000000000 ),
 .UNSPECIFIED. ) ;
#18948 = DIRECTION ( 'NONE',  ( 1.000000000000000000, 0.000000000000000000, 0.000000000000000000 ) ) ;
#18949 = CARTESIAN_POINT ( 'NONE',  ( -9.999999999979998222, -27.00000000000000000, -31.39999999999999858 ) ) ;
#18950 = CARTESIAN_POINT ( 'NONE',  ( 10.69999999998082174, -126.8166236165483554, -33.90282598914290446 ) ) ;
#18951 = EDGE_LOOP ( 'NONE', ( #5793, #9563, #19194, #1902, #559 ) ) ;
#18952 = CARTESIAN_POINT ( 'NONE',  ( 27.79999999999999716, -2.355626804729999831E-11, 222.0000000000000000 ) ) ;
#18953 = LINE ( 'NONE', #23846, #13089 ) ;
#18954 = ADVANCED_FACE ( 'NONE', ( #5929 ), #21047, .F. ) ;
#18955 = CARTESIAN_POINT ( 'NONE',  ( 12.41421356240000051, 25.87105682045942245, -59.46203493729375822 ) ) ;
#18956 = CARTESIAN_POINT ( 'NONE',  ( -4.781437088831645532, 0.4141712122942822205, -68.10000000002500542 ) ) ;
#18957 = EDGE_CURVE ( 'NONE', #4180, #12069, #27642, .T. ) ;
#18958 = VECTOR ( 'NONE', #15705, 1000.000000000000227 ) ;
#18959 = CARTESIAN_POINT ( 'NONE',  ( 10.45000000009999930, -27.00000000000000000, -28.39999999989999679 ) ) ;
#18960 = CARTESIAN_POINT ( 'NONE',  ( 6.778377084329999747, 9.970142431730000254, 230.6412452697800006 ) ) ;
#18961 = AXIS2_PLACEMENT_3D ( 'NONE', #14304, #26415, #23911 ) ;
#18962 = ORIENTED_EDGE ( 'NONE', *, *, #598, .T. ) ;
#18963 = CARTESIAN_POINT ( 'NONE',  ( -11.49589586079802750, -4.456723305597296125, 232.6627637660202197 ) ) ;
#18964 = CARTESIAN_POINT ( 'NONE',  ( 1.568292632099254291, -27.75603058367145692, 4.689797669000017599 ) ) ;
#18965 = EDGE_LOOP ( 'NONE', ( #2875, #18487, #30069, #10134, #10627 ) ) ;
#18966 = CARTESIAN_POINT ( 'NONE',  ( -4.175165894169885483, -55.00000000000000000, -44.10000000000000142 ) ) ;
#18967 = CARTESIAN_POINT ( 'NONE',  ( 0.8372177269581546621, 4.490875019823945991, -63.42744533512499316 ) ) ;
#18968 = ORIENTED_EDGE ( 'NONE', *, *, #5805, .F. ) ;
#18969 = CARTESIAN_POINT ( 'NONE',  ( -380005.9281980000087, -207598.1847299999790, 250226.6334002700169 ) ) ;
#18970 = SURFACE_STYLE_FILL_AREA ( #9534 ) ;
#18971 = CARTESIAN_POINT ( 'NONE',  ( 27.50000000000000000, -3.367667472999999580E-15, 43.28090191849999968 ) ) ;
#18972 = CARTESIAN_POINT ( 'NONE',  ( -17.31982526421443680, -22.92225716952031078, -31.81921677123528980 ) ) ;
#18973 = CARTESIAN_POINT ( 'NONE',  ( 9.897162125286888212, -25.37356426548039678, 138.3395398250000028 ) ) ;
#18974 = FACE_OUTER_BOUND ( 'NONE', #24764, .T. ) ;
#18975 = EDGE_LOOP ( 'NONE', ( #22872, #6616, #17971, #30255 ) ) ;
#18976 = LINE ( 'NONE', #28584, #1949 ) ;
#18977 = CARTESIAN_POINT ( 'NONE',  ( 0.9560301455467571374, -26.78297054432951896, 225.5489681738553713 ) ) ;
#18978 = EDGE_CURVE ( 'NONE', #23086, #22033, #6558, .T. ) ;
#18979 = CARTESIAN_POINT ( 'NONE',  ( 20.15227961529999945, 20.00000826590000003, 229.6286087310000141 ) ) ;
#18980 = AXIS2_PLACEMENT_3D ( 'NONE', #18389, #11002, #28144 ) ;
#18981 = CARTESIAN_POINT ( 'NONE',  ( -15.82777162301967167, -9.463291056475755525, 0.000000000000000000 ) ) ;
#18982 = CARTESIAN_POINT ( 'NONE',  ( -12.37231291231705832, -30.42659210113913915, -32.19515882010285424 ) ) ;
#18983 = CARTESIAN_POINT ( 'NONE',  ( -1.127665019380000189, -28.47796022459999676, 225.1040592169999854 ) ) ;
#18984 = VECTOR ( 'NONE', #10639, 1000.000000000000000 ) ;
#18985 = DIRECTION ( 'NONE',  ( -0.000000000000000000, 1.000000000000000000, -2.257145581549999994E-12 ) ) ;
#18986 = AXIS2_PLACEMENT_3D ( 'NONE', #12170, #4940, #19417 ) ;
#18987 = CYLINDRICAL_SURFACE ( 'NONE', #240, 27.50000000000000000 ) ;
#18988 = CARTESIAN_POINT ( 'NONE',  ( -14.90000000006999947, -30.00000000000000000, -28.40000000020000215 ) ) ;
#18989 = CARTESIAN_POINT ( 'NONE',  ( 6.136659917679837761, 0.6935318534637759935, -54.53771407622500078 ) ) ;
#18990 = CARTESIAN_POINT ( 'NONE',  ( -19.80526803560000104, 19.50877411510000314, 227.0000000000000000 ) ) ;
#18991 = CARTESIAN_POINT ( 'NONE',  ( -16.46626780658883504, -7.955406060106740895, 0.000000000000000000 ) ) ;
#18992 = CARTESIAN_POINT ( 'NONE',  ( 24.45473033137484720, 14.63622297804190175, 6.098654221000004760 ) ) ;
#18993 = VERTEX_POINT ( 'NONE', #28120 ) ;
#18994 = VECTOR ( 'NONE', #5080, 1000.000000000000114 ) ;
#18995 = FACE_OUTER_BOUND ( 'NONE', #18049, .T. ) ;
#18996 = VERTEX_POINT ( 'NONE', #22938 ) ;
#18997 = CARTESIAN_POINT ( 'NONE',  ( -24.05864279069999867, -13.92996648929999992, 223.9000014189999774 ) ) ;
#18998 = CARTESIAN_POINT ( 'NONE',  ( -4.178199994060139311, -1.098053884355550069, -56.85102360502499153 ) ) ;
#18999 = EDGE_LOOP ( 'NONE', ( #17824, #12961, #2635, #8456 ) ) ;
#19000 = AXIS2_PLACEMENT_3D ( 'NONE', #8541, #15022, #12811 ) ;
#19001 = VERTEX_POINT ( 'NONE', #6085 ) ;
#19002 = B_SPLINE_CURVE_WITH_KNOTS ( 'NONE', 3,
 ( #7273, #16863, #29438, #2856, #24257, #5062 ),
 .UNSPECIFIED., .F., .F.,
 ( 4, 2, 4 ),
 ( 0.000000000000000000, 0.5000000000000000000, 1.000000000000000000 ),
 .UNSPECIFIED. ) ;
#19004 = DIRECTION ( 'NONE',  ( -1.000000000000000000, 0.000000000000000000, -2.257144471330000330E-12 ) ) ;
#19003 = AXIS2_PLACEMENT_3D ( 'NONE', #19176, #4547, #4700 ) ;
#19005 = ORIENTED_EDGE ( 'NONE', *, *, #6912, .T. ) ;
#19006 = CARTESIAN_POINT ( 'NONE',  ( 6.000000000000000000, -23.85203919881242385, -77.55976184388477179 ) ) ;
#19007 = CARTESIAN_POINT ( 'NONE',  ( 4.969149274760951585, -9.773525261618496884, -36.05010821728498627 ) ) ;
#19008 = DIRECTION ( 'NONE',  ( -2.537652630420000242E-15, 0.000000000000000000, 1.000000000000000000 ) ) ;
#19009 = ADVANCED_FACE ( 'NONE', ( #4202 ), #30647, .F. ) ;
#19010 = PRODUCT_DEFINITION_SHAPE ( 'NONE', 'NONE',  #31142 ) ;
#19011 = CARTESIAN_POINT ( 'NONE',  ( 2.476301338670000352, -11.81090098049999959, 231.9999991140000191 ) ) ;
#19012 = CARTESIAN_POINT ( 'NONE',  ( -4.000000000000000000, -31.83942647549183746, -80.46693306215520636 ) ) ;
#19013 = CARTESIAN_POINT ( 'NONE',  ( 27.50000000000000000, 1.776356839399999804E-15, 86.39444872449999480 ) ) ;
#19014 = CARTESIAN_POINT ( 'NONE',  ( -2.564224011386423641, 5.541743391105337757, -7.731725184300000997 ) ) ;
#19015 = CARTESIAN_POINT ( 'NONE',  ( 21.16705260759999874, -21.30254494060000070, 229.0000000000000000 ) ) ;
#19016 = ORIENTED_EDGE ( 'NONE', *, *, #23525, .F. ) ;
#19017 = CARTESIAN_POINT ( 'NONE',  ( -16.83342759575507586, 10.99999999997565503, -0.6999999999999784173 ) ) ;
#19018 = EDGE_CURVE ( 'NONE', #25501, #10676, #25458, .T. ) ;
#19019 = AXIS2_PLACEMENT_3D ( 'NONE', #28143, #300, #9569 ) ;
#19020 = CARTESIAN_POINT ( 'NONE',  ( -4.663991843195165465, -3.413757688390889555, -18.87254627010000263 ) ) ;
#19021 = CARTESIAN_POINT ( 'NONE',  ( -1.022169856810371869, 3.500000000000000000, 230.7522105547308797 ) ) ;
#19022 = DIRECTION ( 'NONE',  ( 0.6986477033485309907, -0.1090476345690993831, -0.7071067811870476172 ) ) ;
#19023 = VECTOR ( 'NONE', #10305, 1000.000000000000114 ) ;
#19024 = CARTESIAN_POINT ( 'NONE',  ( -12.47331730070000155, 21.70000000000000284, -55.90289625529999995 ) ) ;
#19025 = CARTESIAN_POINT ( 'NONE',  ( 27.76135144349999706, -3.399672736829999707E-15, 192.3385858899999903 ) ) ;
#19026 = CARTESIAN_POINT ( 'NONE',  ( -2.036891525988612894, -5.569677580567498509, -43.98640794712500224 ) ) ;
#19027 = FACE_OUTER_BOUND ( 'NONE', #26876, .T. ) ;
#19028 = CARTESIAN_POINT ( 'NONE',  ( -0.08634664488581689223, -3.528971028952712530, 226.6412452697750268 ) ) ;
#19029 = FACE_OUTER_BOUND ( 'NONE', #4142, .T. ) ;
#19030 = EDGE_CURVE ( 'NONE', #24695, #13818, #12642, .T. ) ;
#19031 = ADVANCED_FACE ( 'NONE', ( #4975 ), #24174, .F. ) ;
#19032 = CARTESIAN_POINT ( 'NONE',  ( 9.999999999949999108, -30.49251257979999963, -21.04205368479999905 ) ) ;
#19033 = EDGE_LOOP ( 'NONE', ( #5762, #10570, #20233, #17130, #13767, #18663, #22957, #30745, #4032, #9633 ) ) ;
#19034 = DIRECTION ( 'NONE',  ( 0.000000000000000000, 0.3420201433259318358, -0.9396926207858125046 ) ) ;
#19035 = CARTESIAN_POINT ( 'NONE',  ( -0.1113126277255008650, -0.6952657331094624915, -40.47787123679744070 ) ) ;
#19036 = VERTEX_POINT ( 'NONE', #12206 ) ;
#19037 = CARTESIAN_POINT ( 'NONE',  ( -24.08872333959829959, -11.87645233066230332, 186.7828584124166866 ) ) ;
#19038 = CARTESIAN_POINT ( 'NONE',  ( 4.248246898893026646, -2.821772188863608921, -43.83875473022499847 ) ) ;
#19039 = ORIENTED_EDGE ( 'NONE', *, *, #20020, .F. ) ;
#19040 = ORIENTED_EDGE ( 'NONE', *, *, #27545, .T. ) ;
#19041 = PRODUCT_RELATED_PRODUCT_CATEGORY ( 'part', '', ( #25418 ) ) ;
#19042 = CARTESIAN_POINT ( 'NONE',  ( 0.000000000000000000, 0.000000000000000000, 0.000000000000000000 ) ) ;
#19043 = B_SPLINE_SURFACE_WITH_KNOTS ( 'NONE', 5, 1, ( 
 ( #4199, #21045 ),
 ( #30645, #18666 ),
 ( #2158, #1691 ),
 ( #23876, #2317 ),
 ( #6710, #4047 ),
 ( #13644, #23248 ),
 ( #14584, #19141 ),
 ( #14730, #12666 ),
 ( #21662, #21972 ),
 ( #17232, #12204 ),
 ( #29186, #24326 ),
 ( #26836, #7788 ),
 ( #3068, #24171 ),
 ( #112, #9692 ),
 ( #24633, #9543 ),
 ( #7634, #19762 ),
 ( #2466, #22272 ),
 ( #5120, #2610 ),
 ( #28730, #24024 ),
 ( #22121, #21814 ),
 ( #2771, #426 ),
 ( #29040, #7487 ),
 ( #12058, #19296 ),
 ( #12363, #14890 ),
 ( #2918, #4973 ),
 ( #7179, #24482 ),
 ( #19449, #17081 ) ),
 .UNSPECIFIED., .F., .F., .F.,
 ( 6, 3, 3, 3, 3, 3, 3, 3, 6 ),
 ( 2, 2 ),
 ( 0.000000000000000000, 5.260060211419999909, 10.52012024700000126, 15.78018131380000000, 21.04024955639999916, 26.30030806260000276, 31.56036812210000164, 36.82042849589999634, 41.80426500389999944 ),
 ( -1.078245758850000184E-06, 0.7004350674429999923 ),
 .UNSPECIFIED. ) ;
#19044 = ORIENTED_EDGE ( 'NONE', *, *, #29773, .T. ) ;
#19045 = CARTESIAN_POINT ( 'NONE',  ( -1.419173372210000086E-06, -27.80022181310000207, 223.9000014189999774 ) ) ;
#19046 = ORIENTED_EDGE ( 'NONE', *, *, #16163, .F. ) ;
#19047 = PLANE ( 'NONE',  #2504 ) ;
#19048 = CARTESIAN_POINT ( 'NONE',  ( 23.94466869970572986, 15.45669658583985751, 4.319305385000027364 ) ) ;
#19049 = DIRECTION ( 'NONE',  ( -1.224606353819999829E-16, -1.000000000000000000, 0.000000000000000000 ) ) ;
#19050 = CARTESIAN_POINT ( 'NONE',  ( 0.2160344365416065338, 4.544544668867353643, -35.69999999999999574 ) ) ;
#19051 = B_SPLINE_CURVE_WITH_KNOTS ( 'NONE', 3,
 ( #9205, #11581, #4031, #23859, #13628, #21028, #30629, #1674, #7013, #13943, #4501, #23704 ),
 .UNSPECIFIED., .F., .F.,
 ( 4, 2, 2, 2, 2, 4 ),
 ( 0.000000000000000000, 0.2499999999999984457, 0.4999999999999968914, 0.6249999999999976685, 0.7499999999999984457, 1.000000000000000000 ),
 .UNSPECIFIED. ) ;
#19052 = CARTESIAN_POINT ( 'NONE',  ( 19.32427370919018017, 20.00008879814301466, -0.3673419808590195901 ) ) ;
#19054 = EDGE_CURVE ( 'NONE', #23803, #20395, #28271, .T. ) ;
#19053 = AXIS2_PLACEMENT_3D ( 'NONE', #17685, #881, #8246 ) ;
#19055 = CARTESIAN_POINT ( 'NONE',  ( 10.95000000009999930, -22.55999999999999872, -28.39999999989999679 ) ) ;
#19056 = LINE ( 'NONE', #28960, #28194 ) ;
#19057 = FACE_OUTER_BOUND ( 'NONE', #15274, .T. ) ;
#19058 = ORIENTED_EDGE ( 'NONE', *, *, #8269, .T. ) ;
#19059 = CARTESIAN_POINT ( 'NONE',  ( -3.993179150428259661, -2.644027878211168581, -7.827429326000001630 ) ) ;
#19060 = CARTESIAN_POINT ( 'NONE',  ( 3.499930668453409055, 4.992711500635231836, -28.61106724379999733 ) ) ;
#19061 = CARTESIAN_POINT ( 'NONE',  ( 14.94562240850000023, -8.628859120750000500, 5.000000000000000000 ) ) ;
#19062 = DIRECTION ( 'NONE',  ( 0.000000000000000000, 0.9396926207858125046, 0.3420201433259318358 ) ) ;
#19063 = DIRECTION ( 'NONE',  ( 0.000000000000000000, 0.000000000000000000, -1.000000000000000000 ) ) ;
#19064 = CARTESIAN_POINT ( 'NONE',  ( -17.40631048005291959, 11.95034962824490066, -0.6999999999999784173 ) ) ;
#19065 = CARTESIAN_POINT ( 'NONE',  ( -2.507187057889194381, 3.594686560818127763, -1.627651354100000169 ) ) ;
#19066 = EDGE_CURVE ( 'NONE', #4970, #20193, #25926, .T. ) ;
#19068 = DIRECTION ( 'NONE',  ( 0.3090169943750400994, -0.9510565162951234441, 0.000000000000000000 ) ) ;
#19067 = B_SPLINE_CURVE_WITH_KNOTS ( 'NONE', 5,
 ( #2927, #5126, #3230, #24334, #24641, #14736 ),
 .UNSPECIFIED., .F., .F.,
 ( 6, 6 ),
 ( 64.89339659379999148, 88.33140247330000250 ),
 .UNSPECIFIED. ) ;
#19069 = CARTESIAN_POINT ( 'NONE',  ( 1.379247882482921517, -27.76613141686462782, 5.680166690000016061 ) ) ;
#19070 = CARTESIAN_POINT ( 'NONE',  ( 16.37473331889771089, 11.76353838340827984, 0.000000000000000000 ) ) ;
#19071 = ORIENTED_EDGE ( 'NONE', *, *, #20716, .F. ) ;
#19072 = EDGE_CURVE ( 'NONE', #17371, #11184, #30612, .T. ) ;
#19073 = PRESENTATION_LAYER_ASSIGNMENT (  '', '', ( #6515 ) ) ;
#19074 = EDGE_LOOP ( 'NONE', ( #29674, #20128, #3282, #26493 ) ) ;
#19075 = CYLINDRICAL_SURFACE ( 'NONE', #10269, 4.276011752367109509 ) ;
#19076 = CARTESIAN_POINT ( 'NONE',  ( -5.902313038799129608, -1.548398769286710053, -25.04656121680000425 ) ) ;
#19077 = AXIS2_PLACEMENT_3D ( 'NONE', #15797, #3675, #12820 ) ;
#19078 = VERTEX_POINT ( 'NONE', #4519 ) ;
#19079 = EDGE_CURVE ( 'NONE', #19543, #18386, #15594, .T. ) ;
#19080 = CARTESIAN_POINT ( 'NONE',  ( 23.26185891373408055, -14.66761890384653633, 5.286751411448414650 ) ) ;
#19081 = CARTESIAN_POINT ( 'NONE',  ( 21.02350438529999721, 19.26967166389999875, 225.9999999149999894 ) ) ;
#19082 = ORIENTED_EDGE ( 'NONE', *, *, #27687, .F. ) ;
#19083 = ORIENTED_EDGE ( 'NONE', *, *, #23329, .F. ) ;
#19084 = EDGE_LOOP ( 'NONE', ( #21467, #12972, #28201, #4506 ) ) ;
#19085 = CLOSED_SHELL ( 'NONE', ( #14315, #24603, #24786, #10735, #26414, #28479, #24834, #4266, #22128, #18213, #17702, #11666, #23080, #5898 ) ) ;
#19086 = ORIENTED_EDGE ( 'NONE', *, *, #26867, .T. ) ;
#19087 = CARTESIAN_POINT ( 'NONE',  ( 9.999999999958301800, -27.75984822500470273, -25.47305230110710994 ) ) ;
#19088 = DIRECTION ( 'NONE',  ( 0.3633921898465292122, 0.9316362575375348731, 3.469446951953613400E-15 ) ) ;
#19089 = DIRECTION ( 'NONE',  ( 0.000000000000000000, 0.000000000000000000, 1.000000000000000000 ) ) ;
#19090 = ORIENTED_EDGE ( 'NONE', *, *, #11820, .F. ) ;
#19091 =( LENGTH_UNIT ( ) NAMED_UNIT ( * ) SI_UNIT ( .MILLI., .METRE. ) );
#19092 = DIRECTION ( 'NONE',  ( 1.000000000000000000, -0.000000000000000000, 0.000000000000000000 ) ) ;
#19093 = EDGE_CURVE ( 'NONE', #29138, #20583, #14428, .T. ) ;
#19094 = CARTESIAN_POINT ( 'NONE',  ( 27.76736546530000282, -1.703869824139999878, 222.0000000000000000 ) ) ;
#19095 = CARTESIAN_POINT ( 'NONE',  ( 0.8959394325450000807, -28.48619164239999790, 225.6801530179999986 ) ) ;
#19096 = ORIENTED_EDGE ( 'NONE', *, *, #5628, .F. ) ;
#19097 = CARTESIAN_POINT ( 'NONE',  ( 11.32877539780000120, -24.28840541759999994, -0.7339858088999950958 ) ) ;
#19098 = EDGE_CURVE ( 'NONE', #28870, #13182, #13710, .T. ) ;
#19099 = CARTESIAN_POINT ( 'NONE',  ( 4.813350086082918367, -2.000601425115993148, -16.87122516810000405 ) ) ;
#19100 = DIRECTION ( 'NONE',  ( 0.000000000000000000, 1.000000000000000000, 0.000000000000000000 ) ) ;
#19101 = CARTESIAN_POINT ( 'NONE',  ( 27.06563796540000411, -3.314475222259999564E-15, 88.05973140640000452 ) ) ;
#19102 = ORIENTED_EDGE ( 'NONE', *, *, #6620, .F. ) ;
#19103 = DIRECTION ( 'NONE',  ( 0.3633921898465291567, 0.9316362575375349842, 1.850371707708594444E-14 ) ) ;
#19104 = CARTESIAN_POINT ( 'NONE',  ( -10.69999999999999929, -130.0000000000000000, -40.31722800480000046 ) ) ;
#19105 = CARTESIAN_POINT ( 'NONE',  ( 22.77466902168790241, -14.12660345740818713, 5.703642738130775491 ) ) ;
#19106 = EDGE_CURVE ( 'NONE', #18533, #13699, #23878, .T. ) ;
#19107 = PLANE ( 'NONE',  #18986 ) ;
#19108 = DIRECTION ( 'NONE',  ( -1.000000000000000000, 0.000000000000000000, 0.000000000000000000 ) ) ;
#19109 = LINE ( 'NONE', #26046, #16743 ) ;
#19110 = CARTESIAN_POINT ( 'NONE',  ( 4.175165894169885483, -119.7166638525666826, -44.10000000000000142 ) ) ;
#19111 = ORIENTED_EDGE ( 'NONE', *, *, #30478, .T. ) ;
#19112 = CARTESIAN_POINT ( 'NONE',  ( -10.69999999999999929, -24.87868251500000127, -30.52131748510000264 ) ) ;
#19113 = CARTESIAN_POINT ( 'NONE',  ( 16.21564467616125071, -9.571375077537407350, -0.6999999999999785283 ) ) ;
#19114 = CIRCLE ( 'NONE', #35, 4.000000004070001225 ) ;
#19115 = CARTESIAN_POINT ( 'NONE',  ( -27.02151979721923780, 4.157043372987225816, 0.000000000000000000 ) ) ;
#19116 = CARTESIAN_POINT ( 'NONE',  ( -7.520978907653607770, 5.062343813926256431, -39.94823922369914015 ) ) ;
#19117 = ORIENTED_EDGE ( 'NONE', *, *, #13335, .F. ) ;
#19118 = DIRECTION ( 'NONE',  ( 0.000000000000000000, 0.000000000000000000, -1.000000000000000000 ) ) ;
#19119 =( NAMED_UNIT ( * ) PLANE_ANGLE_UNIT ( ) SI_UNIT ( $, .RADIAN. ) );
#19120 = ORIENTED_EDGE ( 'NONE', *, *, #18957, .F. ) ;
#19121 = DIRECTION ( 'NONE',  ( -1.000000000000000000, 6.565028073413479156E-24, -2.257144471327815248E-12 ) ) ;
#19122 = CARTESIAN_POINT ( 'NONE',  ( -1.449312944839797890, 3.998683954144016894, -69.15099036452500059 ) ) ;
#19123 = ORIENTED_EDGE ( 'NONE', *, *, #3411, .T. ) ;
#19124 = CARTESIAN_POINT ( 'NONE',  ( 1.984841800599668638, 5.152205253018144582, -27.09462237480000368 ) ) ;
#19125 = CARTESIAN_POINT ( 'NONE',  ( 27.23548387060000309, -1.776356839399999804E-15, 138.3395398250000028 ) ) ;
#19126 = CARTESIAN_POINT ( 'NONE',  ( 3.389692407805913632, 3.523397910813151679, -48.69426496242499525 ) ) ;
#19127 = EDGE_CURVE ( 'NONE', #21856, #17533, #29740, .T. ) ;
#19128 = DIRECTION ( 'NONE',  ( -1.000000000000000000, 5.665498452320000818E-16, 0.000000000000000000 ) ) ;
#19129 = CARTESIAN_POINT ( 'NONE',  ( -24.16679028379773797, -15.10730798416152609, 3.997250019000003540 ) ) ;
#19130 = LINE ( 'NONE', #22545, #26569 ) ;
#19131 = MECHANICAL_DESIGN_GEOMETRIC_PRESENTATION_REPRESENTATION (  '', ( #20635 ), #17769 ) ;
#19132 = UNCERTAINTY_MEASURE_WITH_UNIT (LENGTH_MEASURE( 1.000000000000000082E-05 ), #22909, 'distance_accuracy_value', 'NONE');
#19133 = CARTESIAN_POINT ( 'NONE',  ( 1.776356839399999922E-14, 0.000000000000000000, 232.6627637660000119 ) ) ;
#19134 = EDGE_CURVE ( 'NONE', #17637, #7280, #4680, .T. ) ;
#19135 = CARTESIAN_POINT ( 'NONE',  ( 11.78524365254896011, 20.99999999989818278, -70.02191803005808879 ) ) ;
#19136 = ADVANCED_FACE ( 'NONE', ( #21505 ), #16770, .F. ) ;
#19137 = CARTESIAN_POINT ( 'NONE',  ( -6.000000000000000000, -17.74403716370463968, -75.33663091226621589 ) ) ;
#19138 = ORIENTED_EDGE ( 'NONE', *, *, #1001, .T. ) ;
#19139 = CARTESIAN_POINT ( 'NONE',  ( 21.81247352487541136, 17.27884107588915796, 6.000000000000005329 ) ) ;
#19140 = CARTESIAN_POINT ( 'NONE',  ( 10.69999999996178985, -27.75961006684773835, -25.47288920101188125 ) ) ;
#19141 = CARTESIAN_POINT ( 'NONE',  ( -4.865153911790000230, 11.29064247420000022, 232.6627643349999914 ) ) ;
#19142 = CARTESIAN_POINT ( 'NONE',  ( -26.95773186790000153, 8.656139623419999651, 226.2000000000000171 ) ) ;
#19143 = CARTESIAN_POINT ( 'NONE',  ( -12.58977862431063244, -31.50799326805841361, -31.57081156527973675 ) ) ;
#19144 = LINE ( 'NONE', #26390, #11508 ) ;
#19145 = DIRECTION ( 'NONE',  ( -1.000000000000000000, 0.000000000000000000, 0.000000000000000000 ) ) ;
#19146 = CARTESIAN_POINT ( 'NONE',  ( -25.25401215124432852, 13.21081861195569296, 4.098596794000014754 ) ) ;
#19147 = FACE_OUTER_BOUND ( 'NONE', #12755, .T. ) ;
#19148 = CIRCLE ( 'NONE', #21151, 3.000000000000001332 ) ;
#19149 = CARTESIAN_POINT ( 'NONE',  ( -6.000000000000000000, -17.74403716370463968, -75.33663091226621589 ) ) ;
#19150 = FACE_OUTER_BOUND ( 'NONE', #25549, .T. ) ;
#19151 = CARTESIAN_POINT ( 'NONE',  ( -2.107992564109736566, -27.41908764619380889, 20.00000000000000355 ) ) ;
#19152 = B_SPLINE_CURVE_WITH_KNOTS ( 'NONE', 5,
 ( #25864, #10745, #13255, #22873, #1315, #14519 ),
 .UNSPECIFIED., .F., .F.,
 ( 6, 6 ),
 ( 0.000000000000000000, 2.319814964899999943 ),
 .UNSPECIFIED. ) ;
#19153 = ORIENTED_EDGE ( 'NONE', *, *, #10588, .F. ) ;
#19154 = CARTESIAN_POINT ( 'NONE',  ( -17.04621913067799710, -22.00000000000000000, -25.51324865357000249 ) ) ;
#19155 = ORIENTED_EDGE ( 'NONE', *, *, #13270, .F. ) ;
#19156 = CARTESIAN_POINT ( 'NONE',  ( 27.50000000000000000, -3.367667472999999580E-15, 43.60555127639999995 ) ) ;
#19157 = EDGE_CURVE ( 'NONE', #17178, #10044, #2612, .T. ) ;
#19158 = CARTESIAN_POINT ( 'NONE',  ( -0.06606756225350368661, 5.646037861211643083, -57.31818518972499277 ) ) ;
#19159 = VERTEX_POINT ( 'NONE', #14586 ) ;
#19160 = EDGE_CURVE ( 'NONE', #18191, #662, #23868, .T. ) ;
#19161 = CONTEXT_DEPENDENT_SHAPE_REPRESENTATION ( #8355, #15187 ) ;
#19162 =( BOUNDED_SURFACE ( )  B_SPLINE_SURFACE ( 5, 3, ( 
 ( #7768, #24463, #29323, #1012 ),
 ( #8220, #19586, #10601, #24615 ),
 ( #22414, #12808, #25077, #26972 ),
 ( #858, #29168, #14871, #7916 ),
 ( #10301, #5409, #19897, #17521 ),
 ( #29480, #27127, #27278, #10450 ),
 ( #5562, #7614, #5718, #22103 ),
 ( #15163, #20044, #2897, #15324 ),
 ( #8070, #17665, #24767, #17211 ),
 ( #20194, #24924, #3352, #26816 ),
 ( #5261, #12959, #29788, #17822 ),
 ( #27431, #5867, #15477, #3509 ),
 ( #12492, #13106, #561, #10141 ),
 ( #19741, #1636, #3835, #11225 ),
 ( #27740, #16101, #25553, #17973 ) ),
 .UNSPECIFIED., .F., .F., .T. ) 
 B_SPLINE_SURFACE_WITH_KNOTS ( ( 6, 3, 3, 3, 6 ),
 ( 4, 4 ),
 ( 0.000000000000000000, 2.784556496770000056, 5.569112993540000112, 8.353669490309998835, 11.13822598710000022 ),
 ( 0.000000000000000000, 1.000000000000000000 ),
 .UNSPECIFIED. ) 
 GEOMETRIC_REPRESENTATION_ITEM ( )  RATIONAL_B_SPLINE_SURFACE ( (
 ( 1.000000000000000000, 0.9492530216734372805, 0.9492530216734372805, 1.000000000000000000),
 ( 1.000000000000000000, 0.9492530216734372805, 0.9492530216734372805, 1.000000000000000000),
 ( 1.000000000000000000, 0.9492530216734372805, 0.9492530216734372805, 1.000000000000000000),
 ( 1.000000000000000000, 0.9492530216734372805, 0.9492530216734372805, 1.000000000000000000),
 ( 1.000000000000000000, 0.9492530216734372805, 0.9492530216734372805, 1.000000000000000000),
 ( 1.000000000000000000, 0.9492530216734372805, 0.9492530216734372805, 1.000000000000000000),
 ( 1.000000000000000000, 0.9492530216734372805, 0.9492530216734372805, 1.000000000000000000),
 ( 1.000000000000000000, 0.9492530216734372805, 0.9492530216734372805, 1.000000000000000000),
 ( 1.000000000000000000, 0.9492530216734372805, 0.9492530216734372805, 1.000000000000000000),
 ( 1.000000000000000000, 0.9492530216734372805, 0.9492530216734372805, 1.000000000000000000),
 ( 1.000000000000000000, 0.9492530216734372805, 0.9492530216734372805, 1.000000000000000000),
 ( 1.000000000000000000, 0.9492530216734372805, 0.9492530216734372805, 1.000000000000000000),
 ( 1.000000000000000000, 0.9492530216734372805, 0.9492530216734372805, 1.000000000000000000),
 ( 1.000000000000000000, 0.9492530216734372805, 0.9492530216734372805, 1.000000000000000000),
 ( 1.000000000000000000, 0.9492530216734372805, 0.9492530216734372805, 1.000000000000000000) ) ) 
 REPRESENTATION_ITEM ( '' )  SURFACE ( )  );
#19163 = ORIENTED_EDGE ( 'NONE', *, *, #6098, .T. ) ;
#19164 = CARTESIAN_POINT ( 'NONE',  ( -28.49999999979999998, 4.437032521639999949, 229.0000000000000000 ) ) ;
#19165 = VERTEX_POINT ( 'NONE', #24790 ) ;
#19166 = CARTESIAN_POINT ( 'NONE',  ( 8.000000000251308307, -25.22417743378453281, -30.84961367804113763 ) ) ;
#19167 = CARTESIAN_POINT ( 'NONE',  ( 12.12499559729999810, 20.99999999999999645, -55.73512174120000395 ) ) ;
#19168 = PRESENTATION_STYLE_ASSIGNMENT (( #9247 ) ) ;
#19169 = PRESENTATION_LAYER_ASSIGNMENT (  '', '', ( #30719 ) ) ;
#19170 = FACE_OUTER_BOUND ( 'NONE', #3408, .T. ) ;
#19171 = CARTESIAN_POINT ( 'NONE',  ( -25.14597776469910428, -15.02549348198344603, 1.000000000000000888 ) ) ;
#19172 = CARTESIAN_POINT ( 'NONE',  ( 27.63177356690000153, -3.383804547719999749E-15, 87.36052363810000543 ) ) ;
#19173 = CARTESIAN_POINT ( 'NONE',  ( -1.295942751353782674, 4.166547562507306957, -4.274955258300005667 ) ) ;
#19174 = CARTESIAN_POINT ( 'NONE',  ( 25.63755059829999894, -14.69299249370000204, 230.2432540810000319 ) ) ;
#19175 = ORIENTED_EDGE ( 'NONE', *, *, #5213, .T. ) ;
#19176 = CARTESIAN_POINT ( 'NONE',  ( -11.49999999969999998, 20.99999999990000887, -70.09999999999999432 ) ) ;
#19177 = CARTESIAN_POINT ( 'NONE',  ( 0.7420639427752478978, -6.011517603930927045, -18.37054674910000429 ) ) ;
#19178 = CARTESIAN_POINT ( 'NONE',  ( 2.020725942159999899, 3.500000000000000000, 230.5235986622430175 ) ) ;
#19179 = CARTESIAN_POINT ( 'NONE',  ( -10.07772970569999949, -25.00000000000000000, -1.850024072400001440 ) ) ;
#19180 = CARTESIAN_POINT ( 'NONE',  ( -3.796508279279999787, -11.43135309280000023, 230.6412452697800006 ) ) ;
#19181 = CARTESIAN_POINT ( 'NONE',  ( -15.88307796653755055, 11.57288288501910856, -0.6999999999999784173 ) ) ;
#19182 = CARTESIAN_POINT ( 'NONE',  ( 2.472051776111518162, -3.869239954018615535, -42.81966640442499994 ) ) ;
#19183 = CARTESIAN_POINT ( 'NONE',  ( -7.999999999946012075, -112.2299448184148645, 5.890987397396584946 ) ) ;
#19184 = CARTESIAN_POINT ( 'NONE',  ( 0.09707459473891824620, -26.79999999950000245, 223.8999999999999773 ) ) ;
#19185 = CARTESIAN_POINT ( 'NONE',  ( -24.75645986059670278, -14.12045945564184279, 5.901294544000013076 ) ) ;
#19186 = EDGE_CURVE ( 'NONE', #6392, #11688, #29086, .T. ) ;
#19187 = EDGE_CURVE ( 'NONE', #16332, #12633, #17234, .T. ) ;
#19188 = CARTESIAN_POINT ( 'NONE',  ( 8.999999999770000869, 21.64982007969998890, -44.65000838630700031 ) ) ;
#19189 = CIRCLE ( 'NONE', #17160, 27.50000000000000000 ) ;
#19190 = ORIENTED_EDGE ( 'NONE', *, *, #13303, .T. ) ;
#19191 = CARTESIAN_POINT ( 'NONE',  ( 4.262644516445695864, -31.82750668785732628, -80.46259461425745485 ) ) ;
#19192 = CARTESIAN_POINT ( 'NONE',  ( -10.99999999999209344, -15.94902145826098483, -35.53273252503156243 ) ) ;
#19193 = CARTESIAN_POINT ( 'NONE',  ( 0.6633312702179999798, 20.00000000000000000, 230.6999999999999886 ) ) ;
#19194 = ORIENTED_EDGE ( 'NONE', *, *, #20932, .F. ) ;
#19195 = CARTESIAN_POINT ( 'NONE',  ( 24.32472894995379420, -13.45989151107506387, 3.899998581000013509 ) ) ;
#19196 = CARTESIAN_POINT ( 'NONE',  ( 4.531630834892029114, -0.6723478992683162847, -46.53818262062500111 ) ) ;
#19197 = ORIENTED_EDGE ( 'NONE', *, *, #16712, .F. ) ;
#19198 = EDGE_CURVE ( 'NONE', #19698, #10023, #10143, .T. ) ;
#19199 = ORIENTED_EDGE ( 'NONE', *, *, #9606, .T. ) ;
#19200 = ORIENTED_EDGE ( 'NONE', *, *, #19773, .F. ) ;
#19201 = LINE ( 'NONE', #4884, #2442 ) ;
#19202 = ORIENTED_EDGE ( 'NONE', *, *, #18978, .F. ) ;
#19203 = CARTESIAN_POINT ( 'NONE',  ( -27.50000000000000000, 3.367667473009999970E-15, 230.0000000000000000 ) ) ;
#19204 = LINE ( 'NONE', #14493, #20295 ) ;
#19205 = CYLINDRICAL_SURFACE ( 'NONE', #16484, 1.100000000000002309 ) ;
#19206 = CARTESIAN_POINT ( 'NONE',  ( 0.3588211391109571990, 4.320110723951459342, -35.69999999999998863 ) ) ;
#19207 = CARTESIAN_POINT ( 'NONE',  ( 18.61284099291034266, 19.99999152564625859, -0.6181686921151241521 ) ) ;
#19208 = AXIS2_PLACEMENT_3D ( 'NONE', #29372, #3250, #2946 ) ;
#19209 = CARTESIAN_POINT ( 'NONE',  ( -24.74993094845043018, 14.13250375615880117, 6.042507811999997536 ) ) ;
#19210 = LINE ( 'NONE', #23636, #29697 ) ;
#19211 = AXIS2_PLACEMENT_3D ( 'NONE', #21156, #2117, #9182 ) ;
#19212 = CARTESIAN_POINT ( 'NONE',  ( 1.679300368525225240, -1.290548112687445181, 226.6412452697799438 ) ) ;
#19213 = EDGE_CURVE ( 'NONE', #18136, #20876, #11818, .T. ) ;
#19214 = CARTESIAN_POINT ( 'NONE',  ( 3.486358836775546699, -2.566383416802847872, -9.472776792900003073 ) ) ;
#19215 = CARTESIAN_POINT ( 'NONE',  ( 0.6138679561251692007, 4.311712124478117580, -29.00600711720001357 ) ) ;
#19216 = CARTESIAN_POINT ( 'NONE',  ( 11.69999999989999928, 19.99999999999999645, -1.399999999299995856 ) ) ;
#19217 = EDGE_CURVE ( 'NONE', #16204, #25641, #2840, .T. ) ;
#19218 = DIRECTION ( 'NONE',  ( 0.000000000000000000, 0.3420201433259318358, -0.9396926207858125046 ) ) ;
#19219 = CARTESIAN_POINT ( 'NONE',  ( 19.90458219140913343, 19.99999992531521187, 0.04954396799999871703 ) ) ;
#19220 = CARTESIAN_POINT ( 'NONE',  ( 12.41421356240000051, 25.87105682045942245, -59.46203493729375822 ) ) ;
#19221 = CARTESIAN_POINT ( 'NONE',  ( 2.521631941452523229, 3.946033397249450125, -5.200967428500000267 ) ) ;
#19222 = CARTESIAN_POINT ( 'NONE',  ( 23.99475407440551322, -14.04003783131165228, 5.886818977337623160 ) ) ;
#19223 = APPLICATION_CONTEXT ( 'automotive_design' ) ;
#19224 = CARTESIAN_POINT ( 'NONE',  ( -23.83639842770461570, -14.30623133119355828, 3.899998581000013509 ) ) ;
#19225 = DIRECTION ( 'NONE',  ( -1.000000000000000000, 0.000000000000000000, -2.257144471330000330E-12 ) ) ;
#19226 = AXIS2_PLACEMENT_3D ( 'NONE', #8106, #15832, #6222 ) ;
#19227 = ORIENTED_EDGE ( 'NONE', *, *, #12412, .T. ) ;
#19228 = CARTESIAN_POINT ( 'NONE',  ( -7.999999999668361284, -14.95611408987656965, -40.37595097054163773 ) ) ;
#19229 = CARTESIAN_POINT ( 'NONE',  ( -12.34127026248727077, -32.00000000000001421, -29.28730138128909033 ) ) ;
#19230 = EDGE_LOOP ( 'NONE', ( #9790, #9630 ) ) ;
#19231 = CARTESIAN_POINT ( 'NONE',  ( 24.87112161019999945, -13.91739822849999975, 226.0424756639999941 ) ) ;
#19232 = CARTESIAN_POINT ( 'NONE',  ( -23.20948082139999968, -13.40000000000000036, 226.0999999999999943 ) ) ;
#19234 = ORIENTED_EDGE ( 'NONE', *, *, #10210, .T. ) ;
#19233 = CIRCLE ( 'NONE', #11189, 1.656072167390155281 ) ;
#19235 = ORIENTED_EDGE ( 'NONE', *, *, #13840, .T. ) ;
#19236 = EDGE_CURVE ( 'NONE', #5207, #15698, #21195, .T. ) ;
#19237 = ORIENTED_EDGE ( 'NONE', *, *, #23697, .F. ) ;
#19238 =( NAMED_UNIT ( * ) SI_UNIT ( $, .STERADIAN. ) SOLID_ANGLE_UNIT ( ) );
#19239 = EDGE_LOOP ( 'NONE', ( #24811, #23231, #25867, #9359, #16371, #20003 ) ) ;
#19240 = CARTESIAN_POINT ( 'NONE',  ( -23.24663841809999809, -14.69162354060000020, 5.000000000000000000 ) ) ;
#19241 = FACE_OUTER_BOUND ( 'NONE', #27277, .T. ) ;
#19242 = CARTESIAN_POINT ( 'NONE',  ( -10.69999999999999929, -24.87868251500000127, -30.52131748510000264 ) ) ;
#19243 = ORIENTED_EDGE ( 'NONE', *, *, #31101, .T. ) ;
#19244 = CARTESIAN_POINT ( 'NONE',  ( 10.69999999999999929, -130.0000000000000000, -42.39999999999999858 ) ) ;
#19245 = LINE ( 'NONE', #28533, #20702 ) ;
#19246 = CARTESIAN_POINT ( 'NONE',  ( 19.06888577842656574, 19.69230313816537148, 0.2004941630000256492 ) ) ;
#19247 = FACE_OUTER_BOUND ( 'NONE', #7620, .T. ) ;
#19248 = EDGE_CURVE ( 'NONE', #10592, #5736, #21237, .T. ) ;
#19249 = CARTESIAN_POINT ( 'NONE',  ( 2.917755696240735386, -4.045878105792589885, -0.6999995769812824564 ) ) ;
#19250 = ORIENTED_EDGE ( 'NONE', *, *, #5031, .T. ) ;
#19251 = LINE ( 'NONE', #15411, #28060 ) ;
#19252 = EDGE_CURVE ( 'NONE', #28706, #14673, #15647, .T. ) ;
#19253 = CARTESIAN_POINT ( 'NONE',  ( -2.345194346458623347, -4.011532291445385923, -15.18182079290000530 ) ) ;
#19254 = CARTESIAN_POINT ( 'NONE',  ( -7.999999999651103977, -16.53431405373043717, -37.98000797241422788 ) ) ;
#19255 = DIRECTION ( 'NONE',  ( 0.9880370573969196046, -0.1542166437529879364, -8.326672684677467298E-17 ) ) ;
#19256 = VECTOR ( 'NONE', #7675, 1000.000000000000000 ) ;
#19257 = EDGE_LOOP ( 'NONE', ( #29024, #11342, #29359, #12221 ) ) ;
#19258 = CARTESIAN_POINT ( 'NONE',  ( 16.06937396351131397, 10.83602254743009219, -0.6999999999999784173 ) ) ;
#19259 = FACE_OUTER_BOUND ( 'NONE', #3752, .T. ) ;
#19260 = CARTESIAN_POINT ( 'NONE',  ( -13.99999999969999820, 21.69999999929999390, -67.09999999999999432 ) ) ;
#19261 = ADVANCED_FACE ( 'NONE', ( #3533 ), #19497, .T. ) ;
#19262 = CARTESIAN_POINT ( 'NONE',  ( 0.000000000000000000, 0.000000000000000000, 230.6412452697800006 ) ) ;
#19263 = CARTESIAN_POINT ( 'NONE',  ( 7.908785388650001025, 16.35326433119999834, 230.0000000000000000 ) ) ;
#19264 = CARTESIAN_POINT ( 'NONE',  ( 12.63375938795768150, 20.99999999997314148, -55.99857472579974882 ) ) ;
#19265 = CARTESIAN_POINT ( 'NONE',  ( -5.114260856059999583, -17.43050419540000107, 230.6999999999999886 ) ) ;
#19266 = EDGE_LOOP ( 'NONE', ( #14297, #538, #28785, #680 ) ) ;
#19267 = CARTESIAN_POINT ( 'NONE',  ( -9.999999999979998222, -27.00000000000000000, -31.39999999999999858 ) ) ;
#19268 = CYLINDRICAL_SURFACE ( 'NONE', #2573, 2.000000000000002665 ) ;
#19269 = CARTESIAN_POINT ( 'NONE',  ( -1.864922697349092662, -4.767250968724650484, -68.10000000002503384 ) ) ;
#19270 = EDGE_CURVE ( 'NONE', #21606, #4812, #9186, .T. ) ;
#19271 = CARTESIAN_POINT ( 'NONE',  ( -1.421085471519999843E-14, -3.552713678799999608E-15, 136.3944487250000179 ) ) ;
#19272 = ORIENTED_EDGE ( 'NONE', *, *, #29945, .T. ) ;
#19273 = AXIS2_PLACEMENT_3D ( 'NONE', #15568, #3611, #22980 ) ;
#19274 = CARTESIAN_POINT ( 'NONE',  ( -1.111846212942793288, 3.388043077328151131, -88.52261276238974119 ) ) ;
#19275 = STYLED_ITEM ( 'NONE', ( #7953 ), #25297 ) ;
#19276 = ORIENTED_EDGE ( 'NONE', *, *, #21630, .F. ) ;
#19277 = DIRECTION ( 'NONE',  ( 0.000000000000000000, 0.000000000000000000, -1.000000000000000000 ) ) ;
#19278 = CARTESIAN_POINT ( 'NONE',  ( 0.5057536231481327693, -27.79562098839016571, 3.899998581000013509 ) ) ;
#19279 = ORIENTED_EDGE ( 'NONE', *, *, #9204, .F. ) ;
#19280 = CARTESIAN_POINT ( 'NONE',  ( -3.878879136156900387, -1.961445906012333928, -28.46472909259999895 ) ) ;
#19281 = EDGE_CURVE ( 'NONE', #3507, #29499, #3555, .T. ) ;
#19282 = CARTESIAN_POINT ( 'NONE',  ( -1.680165883105034119, -1.289604809122433915, 226.6412452697800859 ) ) ;
#19283 = B_SPLINE_CURVE_WITH_KNOTS ( 'NONE', 3,
 ( #20254, #15532, #25137, #3573, #13167, #26885, #14928, #25462, #30006, #6716, #13807, #20572 ),
 .UNSPECIFIED., .F., .F.,
 ( 4, 2, 2, 2, 2, 4 ),
 ( 0.000000000000000000, 0.2500000000000104916, 0.5000000000000210942, 0.6250000000000264233, 0.7500000000000319744, 1.000000000000000000 ),
 .UNSPECIFIED. ) ;
#19284 = B_SPLINE_CURVE_WITH_KNOTS ( 'NONE', 5,
 ( #24152, #14562, #21643, #26365, #23853, #7320, #91, #9670, #16903 ),
 .UNSPECIFIED., .F., .F.,
 ( 6, 3, 6 ),
 ( 0.000000000000000000, 18.05539734199999913, 32.16884876519999636 ),
 .UNSPECIFIED. ) ;
#19285 = CARTESIAN_POINT ( 'NONE',  ( 2.833778097863427714, 3.583098331959792660, -63.63768011632500787 ) ) ;
#19286 = LINE ( 'NONE', #7328, #4004 ) ;
#19287 = CARTESIAN_POINT ( 'NONE',  ( -3.458129700889219116, 0.5397582531354577773, 226.6412452697749984 ) ) ;
#19288 = CARTESIAN_POINT ( 'NONE',  ( 24.09856112909999837, -15.21545593799999985, 225.0000014190000002 ) ) ;
#19289 = FACE_OUTER_BOUND ( 'NONE', #11918, .T. ) ;
#19290 = VECTOR ( 'NONE', #2778, 1000.000000000000114 ) ;
#19291 = DIRECTION ( 'NONE',  ( 0.2815395311429191860, 0.9595496299847263710, 0.000000000000000000 ) ) ;
#19292 = ORIENTED_EDGE ( 'NONE', *, *, #16313, .T. ) ;
#19293 = FACE_OUTER_BOUND ( 'NONE', #27239, .T. ) ;
#19294 = FACE_OUTER_BOUND ( 'NONE', #3192, .T. ) ;
#19295 = TOROIDAL_SURFACE ( 'NONE', #23323, 30.50000000000000000, 3.000000000000000000 ) ;
#19296 = CARTESIAN_POINT ( 'NONE',  ( -4.841056642969999935, -11.34399063919999939, 232.6627643349999914 ) ) ;
#19297 = DIRECTION ( 'NONE',  ( 0.000000000000000000, 0.000000000000000000, 1.000000000000000000 ) ) ;
#19298 = DIRECTION ( 'NONE',  ( -1.000000000000000000, 0.000000000000000000, 0.000000000000000000 ) ) ;
#19299 = FACE_OUTER_BOUND ( 'NONE', #13666, .T. ) ;
#19300 = VECTOR ( 'NONE', #16841, 1000.000000000000000 ) ;
#19301 = CARTESIAN_POINT ( 'NONE',  ( 24.53642653790638661, -13.06930425982346300, 224.4416957644422155 ) ) ;
#19302 = CARTESIAN_POINT ( 'NONE',  ( -1.018916986751970954, -26.78112380549244520, 225.4205820666702493 ) ) ;
#19303 = DIRECTION ( 'NONE',  ( 1.000000000000000000, -1.843431230208684678E-12, 2.650498504958264790E-12 ) ) ;
#19304 = CARTESIAN_POINT ( 'NONE',  ( -5.061979081340524544, -17.25235576957286909, 230.0000000000073896 ) ) ;
#19305 = B_SPLINE_SURFACE_WITH_KNOTS ( 'NONE', 5, 1, ( 
 ( #495, #17606 ),
 ( #20136, #27214 ),
 ( #5187, #15406 ),
 ( #5809, #8008 ),
 ( #19976, #29111 ),
 ( #22501, #951 ) ),
 .UNSPECIFIED., .F., .F., .F.,
 ( 6, 6 ),
 ( 2, 2 ),
 ( 0.000000000000000000, 7.118118795469999149 ),
 ( -0.7000000095410000567, 0.0003774847559270000114 ),
 .UNSPECIFIED. ) ;
#19306 = CARTESIAN_POINT ( 'NONE',  ( 11.07235364852552628, -4.885731121097938612, 232.0000002394077114 ) ) ;
#19307 = CARTESIAN_POINT ( 'NONE',  ( 7.638687372290002386, 3.765626869274008026, -39.31578811164669673 ) ) ;
#19308 = DIRECTION ( 'NONE',  ( -1.553791817432423893E-12, -0.7253743710120292842, 0.6883545756940262494 ) ) ;
#19309 = EDGE_CURVE ( 'NONE', #25785, #1607, #1971, .T. ) ;
#19310 = ORIENTED_EDGE ( 'NONE', *, *, #19309, .F. ) ;
#19311 = CARTESIAN_POINT ( 'NONE',  ( -15.86808677770000209, 10.47263190749999495, -1.399999999599998990 ) ) ;
#19312 = EDGE_CURVE ( 'NONE', #26555, #1709, #16432, .T. ) ;
#19313 = ORIENTED_EDGE ( 'NONE', *, *, #17508, .F. ) ;
#19314 = EDGE_CURVE ( 'NONE', #2111, #6473, #5200, .T. ) ;
#19315 = CARTESIAN_POINT ( 'NONE',  ( 24.50046877880000196, -13.13673243530000079, 225.6806823370000075 ) ) ;
#19316 = CIRCLE ( 'NONE', #22324, 1.656072167390155281 ) ;
#19317 = CARTESIAN_POINT ( 'NONE',  ( -5.545418199629476241, -2.237997381628727300, -59.86491726642499600 ) ) ;
#19318 = AXIS2_PLACEMENT_3D ( 'NONE', #23692, #16897, #26198 ) ;
#19319 = ORIENTED_EDGE ( 'NONE', *, *, #8289, .T. ) ;
#19320 = CIRCLE ( 'NONE', #17742, 8.134694044909998922 ) ;
#19321 = VECTOR ( 'NONE', #16617, 1000.000000000000000 ) ;
#19322 = AXIS2_PLACEMENT_3D ( 'NONE', #15494, #29965, #3531 ) ;
#19323 = EDGE_LOOP ( 'NONE', ( #29340, #12920, #2445, #25906, #14287, #20627, #4677, #29561 ) ) ;
#19324 = CARTESIAN_POINT ( 'NONE',  ( -17.48914026050863768, -24.78381054247710225, -23.90601488817711839 ) ) ;
#19325 = VERTEX_POINT ( 'NONE', #10092 ) ;
#19326 = CARTESIAN_POINT ( 'NONE',  ( 8.000000000252409649, -24.26136093482662304, -29.62468611105709471 ) ) ;
#19327 = CARTESIAN_POINT ( 'NONE',  ( -16.14314806291716664, -9.868837085557133904, -0.6999999999999784173 ) ) ;
#19328 = CARTESIAN_POINT ( 'NONE',  ( 11.26446710299999943, -4.925455829439999711, 232.6627648150000027 ) ) ;
#19329 = DIRECTION ( 'NONE',  ( -0.9831920802501790124, -0.1715636151751586680, -0.06244404920691486172 ) ) ;
#19330 = CARTESIAN_POINT ( 'NONE',  ( -4.484282906631567478, 1.269983465873030015, -7.310827254900003069 ) ) ;
#19331 =( GEOMETRIC_REPRESENTATION_CONTEXT ( 3 ) GLOBAL_UNCERTAINTY_ASSIGNED_CONTEXT ( ( #20063 ) ) GLOBAL_UNIT_ASSIGNED_CONTEXT ( ( #5410, #24925, #27279 ) ) REPRESENTATION_CONTEXT ( 'NONE', 'WORKASPACE' ) );
#19332 = CARTESIAN_POINT ( 'NONE',  ( 27.79539923781684507, 0.5057481689249235801, 8.000000000000007105 ) ) ;
#19333 = ORIENTED_EDGE ( 'NONE', *, *, #13396, .T. ) ;
#19334 = CARTESIAN_POINT ( 'NONE',  ( -9.000000000000000000, 19.99999999999999645, -43.39999999999999858 ) ) ;
#19335 = CARTESIAN_POINT ( 'NONE',  ( 11.26738311299999928, 4.321519186770000687, 231.9999991140000191 ) ) ;
#19336 = CARTESIAN_POINT ( 'NONE',  ( 0.5300456733980305479, -4.293941145674102344, -18.87054674910000074 ) ) ;
#19337 = CARTESIAN_POINT ( 'NONE',  ( -0.9795220552175427642, 3.499999999999998668, 230.7589734104489594 ) ) ;
#19338 = LINE ( 'NONE', #19493, #31095 ) ;
#19339 = B_SPLINE_SURFACE_WITH_KNOTS ( 'NONE', 5, 5, ( 
 ( #3816, #29771, #8203, #17650, #20489, #27414, #3490, #24751, #996 ),
 ( #25059, #30089, #15456, #17953, #8055, #15607, #20180, #6009, #13403 ),
 ( #8358, #1303, #18276, #8675, #10435, #10897, #27263, #3187, #15307 ),
 ( #5700, #13087, #27563, #25213, #25379, #12944, #8515, #23017, #18116 ),
 ( #3644, #27885, #5852, #27719, #6164, #10586, #22697, #843, #12789 ),
 ( #13240, #15150, #15765, #1463, #22857, #1140, #10733, #11055, #30244 ) ),
 .UNSPECIFIED., .F., .F., .F.,
 ( 6, 6 ),
 ( 6, 3, 6 ),
 ( 64.89339659389999326, 88.69760957229999576 ),
 ( 8.011061266649999624, 9.372199858680000162, 10.73333845069999981 ),
 .UNSPECIFIED. ) ;
#19340 = VECTOR ( 'NONE', #3976, 1000.000000000000000 ) ;
#19341 = CARTESIAN_POINT ( 'NONE',  ( 3.389121577140000063, 11.55088360979999962, 230.6412452697800006 ) ) ;
#19342 = VECTOR ( 'NONE', #8525, 1000.000000000000114 ) ;
#19343 = CARTESIAN_POINT ( 'NONE',  ( 11.69999999989999928, 19.99999999999999645, -0.6999999999999992895 ) ) ;
#19344 = DIRECTION ( 'NONE',  ( 0.000000000000000000, 0.000000000000000000, 1.000000000000000000 ) ) ;
#19345 = FACE_OUTER_BOUND ( 'NONE', #21253, .T. ) ;
#19346 = DIRECTION ( 'NONE',  ( 0.000000000000000000, -1.000000000000000000, 0.000000000000000000 ) ) ;
#19347 = CARTESIAN_POINT ( 'NONE',  ( -24.83401023410007724, -13.98326748972919553, 5.760125276000005456 ) ) ;
#19348 = CARTESIAN_POINT ( 'NONE',  ( 1.841797396446237967, -26.73663745407121795, 20.00000000000000355 ) ) ;
#19349 = ORIENTED_EDGE ( 'NONE', *, *, #21334, .F. ) ;
#19350 = CARTESIAN_POINT ( 'NONE',  ( 1.602200344400662058, -4.514849430718075318, -31.19382401680000072 ) ) ;
#19351 = EDGE_CURVE ( 'NONE', #29142, #4930, #9037, .T. ) ;
#19352 = VECTOR ( 'NONE', #18628, 1000.000000000000000 ) ;
#19353 = CARTESIAN_POINT ( 'NONE',  ( -7.999999999650885485, -14.58667674272277104, -37.64499445460491245 ) ) ;
#19354 = VERTEX_POINT ( 'NONE', #2846 ) ;
#19355 = CARTESIAN_POINT ( 'NONE',  ( 25.46368747440213198, -12.80129684534102807, 4.895780544000027490 ) ) ;
#19356 = CARTESIAN_POINT ( 'NONE',  ( 3.054834669310706907, -5.027794097514915350, -47.36669147672500202 ) ) ;
#19357 = VERTEX_POINT ( 'NONE', #2692 ) ;
#19358 = ORIENTED_EDGE ( 'NONE', *, *, #15634, .F. ) ;
#19359 = DIRECTION ( 'NONE',  ( 1.000000000000000000, 0.000000000000000000, 0.000000000000000000 ) ) ;
#19360 = ORIENTED_EDGE ( 'NONE', *, *, #12124, .F. ) ;
#19361 = CARTESIAN_POINT ( 'NONE',  ( -7.999999999730243339, -27.87661103596576595, -25.52343706782910360 ) ) ;
#19362 = ORIENTED_EDGE ( 'NONE', *, *, #29676, .F. ) ;
#19364 = DIRECTION ( 'NONE',  ( 0.000000000000000000, 0.000000000000000000, -1.000000000000000000 ) ) ;
#19363 = AXIS2_PLACEMENT_3D ( 'NONE', #16556, #14674, #2404 ) ;
#19365 = DIRECTION ( 'NONE',  ( -0.8329895880221871440, 0.5532886644841251700, 0.000000000000000000 ) ) ;
#19366 = CYLINDRICAL_SURFACE ( 'NONE', #2924, 3.000000000000002220 ) ;
#19367 = CARTESIAN_POINT ( 'NONE',  ( 0.5587536515777949964, 4.694595604172856262, -35.69999999999999574 ) ) ;
#19368 = CARTESIAN_POINT ( 'NONE',  ( 20.30396079695160694, 19.99999999996773425, 0.7422851442966436064 ) ) ;
#19369 = CARTESIAN_POINT ( 'NONE',  ( 9.499999999960662578, -14.04604638041797138, -36.91140261562396319 ) ) ;
#19370 = DIRECTION ( 'NONE',  ( 0.8775825618903722036, 0.4794255386042040601, 0.000000000000000000 ) ) ;
#19371 = CARTESIAN_POINT ( 'NONE',  ( -24.07583586439999834, -13.90018868249999962, 223.9000014189999774 ) ) ;
#19372 = ORIENTED_EDGE ( 'NONE', *, *, #2583, .T. ) ;
#19373 = B_SPLINE_CURVE_WITH_KNOTS ( 'NONE', 5,
 ( #11520, #8677, #25536, #3972, #4904, #23959, #19065, #509, #11834, #21434, #2546, #6950, #11980, #28662, #31026, #7108, #19221, #7414, #28803, #19382, #21906, #28505, #26765, #24106, #22058, #352, #9463, #191, #12294, #26613, #21592, #9620, #17013, #12132, #12438, #18907, #19539, #21739, #28971, #14816, #29122, #16693, #26305, #9781, #2847, #16545, #16856, #5054, #7566, #14361, #5201, #2393, #4755, #40, #9935, #17158, #14663, #7266, #26462, #24249, #24414, #26154, #2693, #4586, #14510, #14194, #23797, #2244, #7865, #3607, #27382, #5512, #27526, #10245, #5821, #17468, #29896, #22661, #22202, #17917, #15419, #8021, #19687, #24874, #13203, #22815, #10697, #3303, #20148, #5973, #20292, #658, #29272, #19849, #10093, #8166, #12748, #27075, #15117, #15566, #29430, #24714, #3003, #12595, #3453, #1105, #25021, #29586 ),
 .UNSPECIFIED., .F., .F.,
 ( 6, 3, 3, 3, 3, 3, 3, 3, 3, 3, 3, 3, 3, 3, 3, 3, 3, 3, 3, 3, 3, 3, 3, 3, 3, 3, 3, 3, 3, 3, 3, 3, 3, 3, 3, 6 ),
 ( 8.193316113689999014, 11.38862009670000042, 23.17260734260000277, 34.79167593860000096, 46.25425528950000853, 57.87229377410000097, 69.67120816000000616, 81.20502170430000888, 92.80704244429999505, 104.1208912059999960, 115.9269080290000034, 127.3307717769999812, 139.1306782750000082, 150.7654282180000109, 162.2434640489999822, 173.6637378899999931, 185.2020570420000070, 194.1769840819999899, 203.3038760180000111, 212.5853790139999830, 224.1393301889999918, 235.6932813650000469, 246.8715721779999797, 258.4996770380000157, 270.1277818960000445, 281.7035649139999691, 293.2822232819999613, 304.6732510989999696, 316.1434960830000023, 327.6894369340000139, 339.2353777880000507, 350.7813186390000055, 362.5843219139999860, 374.0573691039999744, 385.8560256170000002, 394.7457478480000077 ),
 .UNSPECIFIED. ) ;
#19374 = CARTESIAN_POINT ( 'NONE',  ( 0.2392016894930265591, 6.101552847015987879, -7.937690181100006903 ) ) ;
#19375 = CARTESIAN_POINT ( 'NONE',  ( 3.166603938121563377, 4.517215167231739770, -28.21106724380000585 ) ) ;
#19376 = CARTESIAN_POINT ( 'NONE',  ( 7.707106781468556100, -5.692566302608600637, -27.29492475672613594 ) ) ;
#19377 = AXIS2_PLACEMENT_3D ( 'NONE', #16674, #14173, #12268 ) ;
#19378 = LINE ( 'NONE', #24410, #23238 ) ;
#19379 = CARTESIAN_POINT ( 'NONE',  ( 24.25742563242670613, 13.58028021435546684, 5.680679506000013923 ) ) ;
#19380 = CARTESIAN_POINT ( 'NONE',  ( -2.947640775130000104E-14, -27.50000000000000000, 115.0000000000000000 ) ) ;
#19381 = CARTESIAN_POINT ( 'NONE',  ( 3.163284386374760171, -27.32243547426061170, 20.04829674322551725 ) ) ;
#19382 = CARTESIAN_POINT ( 'NONE',  ( 1.604951280288043014, -4.392199147046020435, -6.260585232200001293 ) ) ;
#19383 = ADVANCED_FACE ( 'NONE', ( #28231 ), #22017, .T. ) ;
#19384 = CARTESIAN_POINT ( 'NONE',  ( 1.592882851206511186, -27.75460863273100998, 5.208113774000016960 ) ) ;
#19385 = DIRECTION ( 'NONE',  ( 0.000000000000000000, 0.000000000000000000, 1.000000000000000000 ) ) ;
#19386 = CARTESIAN_POINT ( 'NONE',  ( -0.3140692933582686641, -3.500175508915968070, 230.8361203540576128 ) ) ;
#19387 = VERTEX_POINT ( 'NONE', #15418 ) ;
#19388 = CARTESIAN_POINT ( 'NONE',  ( 8.000000000365092845, -24.33763746989997401, -26.96262797881743367 ) ) ;
#19389 = CARTESIAN_POINT ( 'NONE',  ( -12.40011512277772354, -32.00000000000000000, -27.11758776248545999 ) ) ;
#19390 = B_SPLINE_CURVE_WITH_KNOTS ( 'NONE', 1,
 ( #15519, #18188 ),
 .UNSPECIFIED., .F., .F.,
 ( 2, 2 ),
 ( -2.555885125540000124E-06, 0.7000000000009999335 ),
 .UNSPECIFIED. ) ;
#19391 = ORIENTED_EDGE ( 'NONE', *, *, #20119, .F. ) ;
#19392 = CARTESIAN_POINT ( 'NONE',  ( 24.71695093370000151, -14.18891100779999981, 226.0986570600000221 ) ) ;
#19393 = DIRECTION ( 'NONE',  ( -1.000000000000000000, 0.000000000000000000, 0.000000000000000000 ) ) ;
#19394 = ORIENTED_EDGE ( 'NONE', *, *, #29212, .T. ) ;
#19395 = ORIENTED_EDGE ( 'NONE', *, *, #29536, .F. ) ;
#19396 = EDGE_LOOP ( 'NONE', ( #9089, #21405, #20616, #7966 ) ) ;
#19397 = ORIENTED_EDGE ( 'NONE', *, *, #4045, .T. ) ;
#19398 = CARTESIAN_POINT ( 'NONE',  ( -17.49999999969999820, -24.00000000000000000, -28.40000000020000215 ) ) ;
#19399 = EDGE_CURVE ( 'NONE', #19859, #16829, #13312, .T. ) ;
#19400 = CARTESIAN_POINT ( 'NONE',  ( -8.699999999650268379, -15.05691612485074948, -37.86814428179198444 ) ) ;
#19401 = CARTESIAN_POINT ( 'NONE',  ( -7.999999999669004325, -18.23122067930106027, -34.51216076568240965 ) ) ;
#19402 = VERTEX_POINT ( 'NONE', #10865 ) ;
#19403 = CARTESIAN_POINT ( 'NONE',  ( -25.41286868645085661, 12.90211872727317655, 5.507123707999994622 ) ) ;
#19404 = B_SPLINE_CURVE_WITH_KNOTS ( 'NONE', 3,
 ( #1075, #12562, #17731, #10519, #29550, #8444, #7984, #29856, #17584, #22321, #30011, #27194, #22168, #27345, #5790, #10665, #5631, #20419, #20117, #20260, #5476, #10209, #24985, #24837, #19809, #8291, #3268, #27040, #13171, #29395, #7832, #24681, #12875, #17886, #5938, #12712, #22478, #1232, #15537, #25142, #3577, #22781, #1390, #30500, #30173, #22946, #28278, #6259 ),
 .UNSPECIFIED., .F., .F.,
 ( 4, 2, 2, 1, 2, 2, 2, 2, 1, 1, 2, 2, 2, 2, 1, 1, 1, 2, 2, 2, 2, 1, 1, 2, 2, 2, 2, 4 ),
 ( 0.000000000000000000, 0.06249999999991126542, 0.09374999999986689814, 0.1093749999998447076, 0.1171874999998356592, 0.1249999999998266109, 0.1874999999997725986, 0.2187499999997477573, 0.2343749999997364886, 0.2421874999997342404, 0.2460937499997351285, 0.2499999999997360445, 0.3749999999997508104, 0.4374999999997613020, 0.4687499999997650213, 0.4843749999997585820, 0.4921874999997553624, 0.4960937499997537525, 0.4999999999997520872, 0.6249999999996466160, 0.6874999999996009858, 0.7187499999995782263, 0.7343749999995679012, 0.7421874999995748956, 0.7499999999995818900, 0.8124999999996801447, 0.8749999999997782885, 1.000000000000000000 ),
 .UNSPECIFIED. ) ;
#19405 = LINE ( 'NONE', #23978, #2484 ) ;
#19406 = CARTESIAN_POINT ( 'NONE',  ( -17.37426278433457583, -31.99976580709003926, -29.84888108430074638 ) ) ;
#19407 = CARTESIAN_POINT ( 'NONE',  ( 7.638687372243862406, -6.912605514289321462, -37.44547201132905911 ) ) ;
#19408 = EDGE_LOOP ( 'NONE', ( #26097, #14996, #21541, #13251 ) ) ;
#19409 = CARTESIAN_POINT ( 'NONE',  ( -23.55444264242456498, 16.04540112444970390, 8.000000000000007105 ) ) ;
#19410 = CARTESIAN_POINT ( 'NONE',  ( -5.853056545089267537, 1.703994407032248581, -16.30443125759999745 ) ) ;
#19411 = CARTESIAN_POINT ( 'NONE',  ( 27.79999999999999716, -2.355626804729999831E-11, 222.0000000000000000 ) ) ;
#19412 = PLANE ( 'NONE',  #23597 ) ;
#19413 = CARTESIAN_POINT ( 'NONE',  ( 8.000000000241653808, -24.19750966826863348, -27.32947504231146851 ) ) ;
#19414 = CARTESIAN_POINT ( 'NONE',  ( 0.5401834767574382745, -27.79499634052776358, 3.899998581000013509 ) ) ;
#19415 = CARTESIAN_POINT ( 'NONE',  ( 23.09885119083424598, -13.58970609041621636, 6.087620938929605430 ) ) ;
#19416 = EDGE_CURVE ( 'NONE', #1204, #25525, #8065, .T. ) ;
#19417 = DIRECTION ( 'NONE',  ( -1.000000000000000000, 4.306888218146944883E-11, 0.000000000000000000 ) ) ;
#19418 = FACE_OUTER_BOUND ( 'NONE', #10066, .T. ) ;
#19419 = CARTESIAN_POINT ( 'NONE',  ( 24.80722736699999942, 13.77662336740000093, 229.2930739560000006 ) ) ;
#19420 = CARTESIAN_POINT ( 'NONE',  ( 0.1718132402369999812, 18.28024009670000183, 230.6999999999999886 ) ) ;
#19421 = ORIENTED_EDGE ( 'NONE', *, *, #17436, .T. ) ;
#19422 = CARTESIAN_POINT ( 'NONE',  ( 19.80538212960000166, 19.50875458629999670, 229.0000000010000178 ) ) ;
#19423 = FACE_OUTER_BOUND ( 'NONE', #27361, .T. ) ;
#19424 = CARTESIAN_POINT ( 'NONE',  ( -4.862250760564064578, -0.002988278297125585882, -68.10000000002500542 ) ) ;
#19425 = EDGE_CURVE ( 'NONE', #8976, #18133, #6973, .T. ) ;
#19426 = ORIENTED_EDGE ( 'NONE', *, *, #19093, .T. ) ;
#19427 = EDGE_CURVE ( 'NONE', #22839, #2756, #10696, .T. ) ;
#19428 = FACE_OUTER_BOUND ( 'NONE', #21659, .T. ) ;
#19429 = FILL_AREA_STYLE_COLOUR ( '', #2732 ) ;
#19430 = ORIENTED_EDGE ( 'NONE', *, *, #28939, .F. ) ;
#19431 = CARTESIAN_POINT ( 'NONE',  ( 8.000000000236575204, -29.80249033211431708, -29.47052495773638370 ) ) ;
#19432 = CARTESIAN_POINT ( 'NONE',  ( 0.5746121234323043891, -27.79431838510023667, 3.901346086000012647 ) ) ;
#19433 = ORIENTED_EDGE ( 'NONE', *, *, #11521, .F. ) ;
#19434 = CARTESIAN_POINT ( 'NONE',  ( 4.370697773661015972, 1.580342671372847230, -27.01249766020000109 ) ) ;
#19435 = CARTESIAN_POINT ( 'NONE',  ( -4.861312627816292142, -17.80543024185618606, -28.79488058873301171 ) ) ;
#19436 = ADVANCED_FACE ( 'NONE', ( #3148 ), #20147, .F. ) ;
#19437 = CARTESIAN_POINT ( 'NONE',  ( -3.250950776947245213, -3.159825117472807143, -47.20083066912499703 ) ) ;
#19438 = CARTESIAN_POINT ( 'NONE',  ( -2.947640775130000104E-14, -27.50000000000000000, 20.00000000000000355 ) ) ;
#19439 = FILL_AREA_STYLE_COLOUR ( '', #14438 ) ;
#19440 = CARTESIAN_POINT ( 'NONE',  ( -16.06710956638348620, 11.80217809800966222, -1.400000000000001910 ) ) ;
#19441 = PRODUCT_DEFINITION_CONTEXT ( 'detailed design', #29691, 'design' ) ;
#19442 = B_SPLINE_CURVE_WITH_KNOTS ( 'NONE', 3,
 ( #20009, #29607, #8038, #10571, #20166, #13222 ),
 .UNSPECIFIED., .F., .F.,
 ( 4, 2, 4 ),
 ( 0.000000000000000000, 0.5000000000000000000, 1.000000000000000000 ),
 .UNSPECIFIED. ) ;
#19443 = CARTESIAN_POINT ( 'NONE',  ( 3.388885134111758735, 1.130278766698372905, 230.7950857227842505 ) ) ;
#19444 = EDGE_CURVE ( 'NONE', #27730, #30584, #3606, .T. ) ;
#19445 = FACE_OUTER_BOUND ( 'NONE', #15777, .T. ) ;
#19446 = VERTEX_POINT ( 'NONE', #7864 ) ;
#19447 = CARTESIAN_POINT ( 'NONE',  ( -15.94164157046648533, 10.34011310946611495, -1.384526174263989415E-13 ) ) ;
#19448 = CARTESIAN_POINT ( 'NONE',  ( -24.97472003774791816, -13.73006752753317450, 5.208359076000035337 ) ) ;
#19449 = CARTESIAN_POINT ( 'NONE',  ( 0.1323034786299999988, -11.99927027549999892, 231.9999989789999972 ) ) ;
#19450 = CARTESIAN_POINT ( 'NONE',  ( -27.79999999999999716, -2.359492241240000038E-11, 227.5999999999999943 ) ) ;
#19451 = CARTESIAN_POINT ( 'NONE',  ( -24.25792036986074507, -13.57958751026097310, 4.317733944950783886 ) ) ;
#19452 = DIRECTION ( 'NONE',  ( 5.962915006522623408E-16, 0.4383711467890811231, 0.8987940462991652613 ) ) ;
#19453 = CARTESIAN_POINT ( 'NONE',  ( 24.60666973300000038, -12.93650480179999995, 225.0000014190000002 ) ) ;
#19454 = CARTESIAN_POINT ( 'NONE',  ( -20.67339670645382199, -21.57700477944339923, 0.2374258030000131470 ) ) ;
#19455 = CARTESIAN_POINT ( 'NONE',  ( -0.2196051059861325316, -26.79904497468144342, 226.0876209393746592 ) ) ;
#19456 = CARTESIAN_POINT ( 'NONE',  ( 24.06826093661917554, -20.50742065831276051, 8.000000000000007105 ) ) ;
#19457 = CARTESIAN_POINT ( 'NONE',  ( 1.947945353336631769, 0.5234957687185587405, 227.6412452701542009 ) ) ;
#19458 = EDGE_CURVE ( 'NONE', #6463, #16100, #22357, .T. ) ;
#19459 = VECTOR ( 'NONE', #23977, 1000.000000000000000 ) ;
#19460 = AXIS2_PLACEMENT_3D ( 'NONE', #27633, #25610, #16148 ) ;
#19461 = CARTESIAN_POINT ( 'NONE',  ( 10.69999999930000101, -29.12132034360000077, -30.52132034359999935 ) ) ;
#19462 = DIRECTION ( 'NONE',  ( 1.000000000000000000, -1.843431230208684274E-12, 2.650498504958264790E-12 ) ) ;
#19463 = CARTESIAN_POINT ( 'NONE',  ( 24.98081130624543889, 13.71897605842228529, 5.104178997000024864 ) ) ;
#19464 = STYLED_ITEM ( 'NONE', ( #24934 ), #890 ) ;
#19465 = EDGE_LOOP ( 'NONE', ( #30451, #2980, #10844, #26733, #19588, #4095, #3432, #12975, #21678, #14753, #19733, #28743, #6017, #30503, #18498, #4879, #17820, #2056, #24079, #5227 ) ) ;
#19466 = CARTESIAN_POINT ( 'NONE',  ( 20.30396079662882158, 20.00000000004802203, 3.000000000000002665 ) ) ;
#19467 = VERTEX_POINT ( 'NONE', #27381 ) ;
#19468 = CARTESIAN_POINT ( 'NONE',  ( 24.68173674080000168, -14.25001227039999918, 223.9000014189999774 ) ) ;
#19469 = ADVANCED_FACE ( 'NONE', ( #27680 ), #22660, .T. ) ;
#19470 = CARTESIAN_POINT ( 'NONE',  ( 3.567773119718944397, 3.614166260817118559, -58.45805965152499084 ) ) ;
#19471 = VERTEX_POINT ( 'NONE', #5972 ) ;
#19472 = ORIENTED_EDGE ( 'NONE', *, *, #15359, .T. ) ;
#19473 = CIRCLE ( 'NONE', #397, 2.500000000105230491 ) ;
#19474 = CARTESIAN_POINT ( 'NONE',  ( 8.700000000232448016, -27.70277699884391964, -25.45709603910293595 ) ) ;
#19475 = ORIENTED_EDGE ( 'NONE', *, *, #27917, .F. ) ;
#19476 = ORIENTED_EDGE ( 'NONE', *, *, #25238, .F. ) ;
#19477 = CARTESIAN_POINT ( 'NONE',  ( 2.100000000239999665, 0.1392085007613527159, 226.6412452697800006 ) ) ;
#19478 = CARTESIAN_POINT ( 'NONE',  ( -23.88992818679365371, 14.21747995069046588, 4.319167817000008291 ) ) ;
#19479 = SURFACE_SIDE_STYLE ('',( #28919 ) ) ;
#19480 = AXIS2_PLACEMENT_3D ( 'NONE', #12735, #18693, #13354 ) ;
#19481 = VECTOR ( 'NONE', #2483, 1000.000000000000000 ) ;
#19482 = CARTESIAN_POINT ( 'NONE',  ( 10.85065064720000017, 5.281366379100000508, 231.9999991140000191 ) ) ;
#19483 = EDGE_CURVE ( 'NONE', #18533, #20783, #24873, .T. ) ;
#19484 = CARTESIAN_POINT ( 'NONE',  ( -19.80535357377644701, 19.50875577052588739, 2.600000085000026218 ) ) ;
#19485 = CARTESIAN_POINT ( 'NONE',  ( 6.034652528523337445, 2.501332855249893683, -11.49261350020000449 ) ) ;
#19486 = DIRECTION ( 'NONE',  ( 0.000000000000000000, -0.9128796883888949942, 0.4082287037029534438 ) ) ;
#19487 = ORIENTED_EDGE ( 'NONE', *, *, #16873, .T. ) ;
#19488 = CARTESIAN_POINT ( 'NONE',  ( 1.408406170841865812, -4.736705221900152196, -44.10000000002499831 ) ) ;
#19489 = CYLINDRICAL_SURFACE ( 'NONE', #7261, 2.500000000000000888 ) ;
#19490 = ADVANCED_FACE ( 'NONE', ( #8479 ), #29030, .F. ) ;
#19491 = CARTESIAN_POINT ( 'NONE',  ( 6.096654317658788180, 0.1519075334363156893, -21.27661200060000724 ) ) ;
#19492 = CARTESIAN_POINT ( 'NONE',  ( 23.55411374389282386, 16.04538543799059980, 8.000000000000007105 ) ) ;
#19493 = CARTESIAN_POINT ( 'NONE',  ( -7.707106781077335711, -60.46534760592810898, -2.801202534621561657 ) ) ;
#19494 = DIRECTION ( 'NONE',  ( 0.000000000000000000, 0.3420201433259318358, -0.9396926207858125046 ) ) ;
#19495 = CARTESIAN_POINT ( 'NONE',  ( 27.50000000000000000, -3.367667472999999580E-15, 193.2809019210000088 ) ) ;
#19496 = CARTESIAN_POINT ( 'NONE',  ( 24.07552309629999954, -13.90001137839999856, 223.9000014189999774 ) ) ;
#19497 = B_SPLINE_SURFACE_WITH_KNOTS ( 'NONE', 5, 5, ( 
 ( #10622, #8719, #18159, #8396, #1504, #25258, #11096, #1342, #17995 ),
 ( #8559, #20691, #1033, #20217, #3690, #27764, #13129, #23214, #15496 ),
 ( #22737, #5889, #29809, #30288, #6050, #30130, #6208, #1184, #13291 ),
 ( #8244, #25733, #17843, #25575, #13761, #22902, #18326, #10779, #27930 ),
 ( #11248, #4169, #15968, #18480, #20376, #4011, #10936, #13608, #27607 ),
 ( #1657, #15816, #30455, #8877, #28079, #25424, #27448, #25100, #29967 ) ),
 .UNSPECIFIED., .F., .F., .F.,
 ( 6, 6 ),
 ( 6, 3, 6 ),
 ( 65.40639850639999509, 88.32365686489998780 ),
 ( 8.011061266649999624, 8.811526687440000671, 9.611992108220000830 ),
 .UNSPECIFIED. ) ;
#19498 = STYLED_ITEM ( 'NONE', ( #9429 ), #11447 ) ;
#19499 = CARTESIAN_POINT ( 'NONE',  ( 10.69999999999945040, -25.27195344073095029, -25.92068947042448457 ) ) ;
#19500 = CARTESIAN_POINT ( 'NONE',  ( 10.69999999999999929, -29.12132034360000077, -30.52132034359999935 ) ) ;
#19501 = CARTESIAN_POINT ( 'NONE',  ( -24.43659368756648576, -14.66646236829179450, 6.099998581000020792 ) ) ;
#19502 = CARTESIAN_POINT ( 'NONE',  ( -1.280497936623963495, -1.670464374936807328, 226.6412452697800290 ) ) ;
#19503 = AXIS2_PLACEMENT_3D ( 'NONE', #1161, #3206, #3511 ) ;
#19504 = CARTESIAN_POINT ( 'NONE',  ( -1.100000000000000089, -17.25771824079999917, 225.0000000000000000 ) ) ;
#19505 = VERTEX_POINT ( 'NONE', #6127 ) ;
#19506 = CARTESIAN_POINT ( 'NONE',  ( 0.8594151385421661127, 6.036396974313712249, -29.60600711720000433 ) ) ;
#19507 = VECTOR ( 'NONE', #29007, 1000.000000000000114 ) ;
#19508 = CARTESIAN_POINT ( 'NONE',  ( -7.999999999652088967, -14.16511107073194076, -37.30738323264701251 ) ) ;
#19509 = EDGE_LOOP ( 'NONE', ( #441, #8814, #27305, #28727 ) ) ;
#19510 = DIRECTION ( 'NONE',  ( -1.000000000000000000, 0.000000000000000000, 0.000000000000000000 ) ) ;
#19511 = CARTESIAN_POINT ( 'NONE',  ( 5.925978784015399903, -0.8792241758803844842, -46.13818262062499542 ) ) ;
#19512 = VERTEX_POINT ( 'NONE', #23455 ) ;
#19513 = ORIENTED_EDGE ( 'NONE', *, *, #12034, .T. ) ;
#19514 = DIRECTION ( 'NONE',  ( 0.9873505073845697533, 0.1585527532634883052, 0.000000000000000000 ) ) ;
#19515 = ORIENTED_EDGE ( 'NONE', *, *, #9865, .F. ) ;
#19516 = CARTESIAN_POINT ( 'NONE',  ( 8.198872691879999995E-10, -3.797984149399999816E-10, 229.6412452697800006 ) ) ;
#19517 = ORIENTED_EDGE ( 'NONE', *, *, #2143, .T. ) ;
#19518 = CYLINDRICAL_SURFACE ( 'NONE', #2013, 1.099999999999999867 ) ;
#19519 = FACE_OUTER_BOUND ( 'NONE', #16522, .T. ) ;
#19520 = LINE ( 'NONE', #24234, #20513 ) ;
#19521 = CARTESIAN_POINT ( 'NONE',  ( 1.171347117349504252, 4.722363560431488416, -35.69999999999999574 ) ) ;
#19522 = AXIS2_PLACEMENT_3D ( 'NONE', #24052, #5143, #2340 ) ;
#19523 = CARTESIAN_POINT ( 'NONE',  ( -12.59914306489253200, -31.53608658979329604, -25.24540812198844364 ) ) ;
#19524 = CARTESIAN_POINT ( 'NONE',  ( -3.779681388771212180, -0.7623632300730877054, -0.6999999999999992895 ) ) ;
#19525 = LINE ( 'NONE', #29113, #18646 ) ;
#19526 = CARTESIAN_POINT ( 'NONE',  ( 13.12132034340000075, 20.99999999999999645, -69.22132034359999864 ) ) ;
#19527 = ORIENTED_EDGE ( 'NONE', *, *, #167, .F. ) ;
#19528 = CARTESIAN_POINT ( 'NONE',  ( 3.619519562537643065, 2.908736503316577959, -8.354586408000006514 ) ) ;
#19529 = CARTESIAN_POINT ( 'NONE',  ( -1.266353310550808464, -4.943458602710906646, -26.61132611460000064 ) ) ;
#19530 = CARTESIAN_POINT ( 'NONE',  ( 2.611298560087381038, -2.373819477306434500, 0.000000000000000000 ) ) ;
#19531 = EDGE_CURVE ( 'NONE', #15161, #10063, #11097, .T. ) ;
#19532 = VECTOR ( 'NONE', #3364, 1000.000000000000114 ) ;
#19533 = EDGE_CURVE ( 'NONE', #7386, #11151, #5612, .T. ) ;
#19534 = FACE_OUTER_BOUND ( 'NONE', #30771, .T. ) ;
#19535 = B_SPLINE_CURVE_WITH_KNOTS ( 'NONE', 3,
 ( #20004, #11343, #23774, #20939, #8813, #25670 ),
 .UNSPECIFIED., .F., .F.,
 ( 4, 2, 4 ),
 ( 0.000000000000000000, 0.5000000000000000000, 1.000000000000000000 ),
 .UNSPECIFIED. ) ;
#19536 = PLANE ( 'NONE',  #24351 ) ;
#19537 = LINE ( 'NONE', #11979, #29719 ) ;
#19538 = CARTESIAN_POINT ( 'NONE',  ( 4.195523629574170243, -27.17925737118813956, 20.25802325405198800 ) ) ;
#19539 = CARTESIAN_POINT ( 'NONE',  ( 2.536150288113637963, -3.576595042060325635, -12.12388893670000201 ) ) ;
#19540 = CARTESIAN_POINT ( 'NONE',  ( 16.21960138463431278, 10.42209091437901414, -1.400000000000001910 ) ) ;
#19541 = CARTESIAN_POINT ( 'NONE',  ( 14.79116926529892417, -25.37390977572334450, -23.56557456066964917 ) ) ;
#19542 = CARTESIAN_POINT ( 'NONE',  ( 0.8681810495234366654, -3.499839992693361435, 230.7751077600164251 ) ) ;
#19543 = VERTEX_POINT ( 'NONE', #2357 ) ;
#19544 = VECTOR ( 'NONE', #4968, 1000.000000000000114 ) ;
#19545 = CARTESIAN_POINT ( 'NONE',  ( 1.413941964909729787, -28.46527362969750996, 4.319830470999985295 ) ) ;
#19546 = CARTESIAN_POINT ( 'NONE',  ( 11.20000000009999930, -32.00000000000000000, -25.51324865394999719 ) ) ;
#19547 = EDGE_LOOP ( 'NONE', ( #1702, #394, #8646, #24729 ) ) ;
#19548 = CARTESIAN_POINT ( 'NONE',  ( 0.000000000000000000, 0.000000000000000000, 138.3395398250000028 ) ) ;
#19549 = CARTESIAN_POINT ( 'NONE',  ( 7.999999999489548763, -115.5267901939644446, 21.04701626999689168 ) ) ;
#19550 = ORIENTED_EDGE ( 'NONE', *, *, #19593, .T. ) ;
#19551 = CARTESIAN_POINT ( 'NONE',  ( -3.229037295491567150, -3.989637411031741632, -44.10000000002499121 ) ) ;
#19552 = ORIENTED_EDGE ( 'NONE', *, *, #11697, .F. ) ;
#19553 = ORIENTED_EDGE ( 'NONE', *, *, #15294, .F. ) ;
#19554 = ORIENTED_EDGE ( 'NONE', *, *, #19968, .T. ) ;
#19555 = CYLINDRICAL_SURFACE ( 'NONE', #17972, 5.000000000000001776 ) ;
#19556 = AXIS2_PLACEMENT_3D ( 'NONE', #16966, #7978, #14620 ) ;
#19557 = CARTESIAN_POINT ( 'NONE',  ( -8.903108651239966420, -22.82508830966961000, 190.0000000000000000 ) ) ;
#19558 = DIRECTION ( 'NONE',  ( 0.7071067811865475727, 0.7071067811865475727, 0.000000000000000000 ) ) ;
#19559 = EDGE_CURVE ( 'NONE', #23263, #21137, #29475, .T. ) ;
#19560 = ORIENTED_EDGE ( 'NONE', *, *, #4018, .T. ) ;
#19561 = DIRECTION ( 'NONE',  ( 1.595945597898660305E-12, 0.7071067811865475727, 0.7071067811865475727 ) ) ;
#19562 = CARTESIAN_POINT ( 'NONE',  ( 1.346291201779999946, -3.434453875705480108, -72.25672407562892374 ) ) ;
#19563 = CARTESIAN_POINT ( 'NONE',  ( -13.99999999967382180, 20.99999999990389554, -67.49269908163661569 ) ) ;
#19564 = CARTESIAN_POINT ( 'NONE',  ( 10.69999999996386286, -29.23055083351040295, -26.39047791497910112 ) ) ;
#19565 = ORIENTED_EDGE ( 'NONE', *, *, #28647, .F. ) ;
#19566 = VECTOR ( 'NONE', #11242, 1000.000000000000000 ) ;
#19567 = CARTESIAN_POINT ( 'NONE',  ( -2.579713781069702616, -4.412685520613435664, -14.74432079290000175 ) ) ;
#19568 = DIRECTION ( 'NONE',  ( 0.000000000000000000, 1.000000000000000000, 0.000000000000000000 ) ) ;
#19569 = CARTESIAN_POINT ( 'NONE',  ( -13.00000000000000000, 25.22617105830878614, -61.82510970417090590 ) ) ;
#19570 = CARTESIAN_POINT ( 'NONE',  ( -12.41634270791311323, -28.29799050060249854, -33.42410161962300208 ) ) ;
#19571 = DIRECTION ( 'NONE',  ( -1.180736691910036071E-13, -0.9986295347540310452, -0.05233595625330160483 ) ) ;
#19572 = CARTESIAN_POINT ( 'NONE',  ( -2.073454313851443853, -2.615810859411399569, -36.20335296946307579 ) ) ;
#19573 = VECTOR ( 'NONE', #9533, 1000.000000000000114 ) ;
#19574 = CARTESIAN_POINT ( 'NONE',  ( -4.276011752264103016, -42.94729992905724458, -9.547410993472153606 ) ) ;
#19575 = CARTESIAN_POINT ( 'NONE',  ( -10.69999999999999929, -25.17332254459999774, -30.78523849680000168 ) ) ;
#19576 = CARTESIAN_POINT ( 'NONE',  ( 21.78117249990000204, 17.46412353909999737, 229.7313245359999883 ) ) ;
#19577 = LINE ( 'NONE', #5400, #20823 ) ;
#19578 = ORIENTED_EDGE ( 'NONE', *, *, #9259, .T. ) ;
#19579 = CARTESIAN_POINT ( 'NONE',  ( -1.293561172433232986, -6.216321778783836294, -52.92706695232499925 ) ) ;
#19580 = CYLINDRICAL_SURFACE ( 'NONE', #24372, 2.500000000000000888 ) ;
#19581 = CARTESIAN_POINT ( 'NONE',  ( -24.45655680962239842, 13.35232502611413707, 0.08279996400001321533 ) ) ;
#19582 = CARTESIAN_POINT ( 'NONE',  ( 9.999999999925533345, -25.12044511670515590, -9.805662262714768929 ) ) ;
#19583 = ADVANCED_FACE ( 'NONE', ( #7376, #16968, #14771 ), #4867, .F. ) ;
#19584 = ORIENTED_EDGE ( 'NONE', *, *, #2695, .T. ) ;
#19585 = ADVANCED_FACE ( 'NONE', ( #9893 ), #4117, .F. ) ;
#19586 = CARTESIAN_POINT ( 'NONE',  ( -3.359412450346234369, 1.172221127227247806, -91.35798291625272327 ) ) ;
#19587 =( NAMED_UNIT ( * ) SI_UNIT ( $, .STERADIAN. ) SOLID_ANGLE_UNIT ( ) );
#19588 = ORIENTED_EDGE ( 'NONE', *, *, #11376, .F. ) ;
#19589 = CARTESIAN_POINT ( 'NONE',  ( 8.903108651239925564, -22.82508830966962421, 90.00000000000000000 ) ) ;
#19590 = CARTESIAN_POINT ( 'NONE',  ( -3.447099378712505935, 3.428612291819206792, -69.69322600202499984 ) ) ;
#19591 = ORIENTED_EDGE ( 'NONE', *, *, #23249, .F. ) ;
#19592 = CARTESIAN_POINT ( 'NONE',  ( -5.902313038799129608, -1.548398769286710053, -25.64656121680000567 ) ) ;
#19593 = EDGE_CURVE ( 'NONE', #28672, #5339, #20445, .T. ) ;
#19594 = LINE ( 'NONE', #99, #18937 ) ;
#19595 = B_SPLINE_SURFACE_WITH_KNOTS ( 'NONE', 5, 5, ( 
 ( #26351, #4172, #4799, #13764, #14396, #83, #23996, #9661, #1820 ),
 ( #11409, #21012, #12480, #26806, #10439, #22094, #16894, #15008, #5550 ),
 ( #392, #10287, #29309, #7606, #24291, #12631, #551, #14551, #24143 ),
 ( #15153, #9977, #17053, #7756, #21782, #19731, #19419, #12172, #17510 ),
 ( #24453, #10132, #17358, #29009, #19576, #24755, #2887, #235, #3190 ),
 ( #22242, #26963, #2739, #20032, #5399, #14702, #24606, #17199, #12335 ) ),
 .UNSPECIFIED., .F., .F., .F.,
 ( 6, 6 ),
 ( 6, 3, 6 ),
 ( 0.000000000000000000, 23.43826350880000220 ),
 ( 8.011061266649999624, 8.811739692309998873, 9.612418117960000785 ),
 .UNSPECIFIED. ) ;
#19596 = CARTESIAN_POINT ( 'NONE',  ( -4.150389416700803302, 1.923785201099231790, -65.77526299422500244 ) ) ;
#19597 = CARTESIAN_POINT ( 'NONE',  ( -24.25955693048148731, -12.95188430978291905, 4.357489519555787005 ) ) ;
#19598 = CARTESIAN_POINT ( 'NONE',  ( 0.6750190879921618148, -27.49190635773182834, 224.1195089973785741 ) ) ;
#19599 = CARTESIAN_POINT ( 'NONE',  ( -7.999999999628841785, -14.30188212870945286, -40.14546951504663497 ) ) ;
#19600 = CARTESIAN_POINT ( 'NONE',  ( -7.999999999683302221, -15.48251719072922050, -33.06200388856654371 ) ) ;
#19601 = CARTESIAN_POINT ( 'NONE',  ( -17.41896590621361085, -22.00022434743734578, -29.54135749160853663 ) ) ;
#19602 = ORIENTED_EDGE ( 'NONE', *, *, #16949, .T. ) ;
#19603 = CARTESIAN_POINT ( 'NONE',  ( 14.72975346148569287, -31.99973334780656486, -26.94935724806895294 ) ) ;
#19604 = EDGE_CURVE ( 'NONE', #18684, #453, #16708, .T. ) ;
#19605 = CARTESIAN_POINT ( 'NONE',  ( 23.52368442168704021, -12.84078897116981466, 224.0862411973129724 ) ) ;
#19606 = CARTESIAN_POINT ( 'NONE',  ( -23.47637529058820860, -14.89020704899713365, 5.901296963999991263 ) ) ;
#19607 = CYLINDRICAL_SURFACE ( 'NONE', #6724, 26.80000000000000071 ) ;
#19608 = CARTESIAN_POINT ( 'NONE',  ( -24.15671119056922933, -13.75882116471486682, 4.114296042299178779 ) ) ;
#19609 = CARTESIAN_POINT ( 'NONE',  ( 3.481616536885269841, -21.27731158793656263, -30.43933673404125173 ) ) ;
#19610 = CARTESIAN_POINT ( 'NONE',  ( 3.339648724517960687, -2.614705901102248209, -0.6999999999999992895 ) ) ;
#19611 = CARTESIAN_POINT ( 'NONE',  ( -24.93121705008275413, -14.89716849126640952, -0.5592437529999827461 ) ) ;
#19612 = CARTESIAN_POINT ( 'NONE',  ( 7.312007425309010600, -7.897185061697537201, -36.96526048002264986 ) ) ;
#19613 = CARTESIAN_POINT ( 'NONE',  ( 28.50000000000000000, -1.776356839399999804E-15, 229.0000000000000000 ) ) ;
#19614 =( GEOMETRIC_REPRESENTATION_CONTEXT ( 3 ) GLOBAL_UNCERTAINTY_ASSIGNED_CONTEXT ( ( #24511 ) ) GLOBAL_UNIT_ASSIGNED_CONTEXT ( ( #572, #8230, #13117 ) ) REPRESENTATION_CONTEXT ( 'NONE', 'WORKASPACE' ) );
#19615 = B_SPLINE_CURVE_WITH_KNOTS ( 'NONE', 3,
 ( #17317, #27380, #12746, #24872, #20449, #7863, #25333, #17466, #15564, #3775, #15264 ),
 .UNSPECIFIED., .F., .F.,
 ( 4, 1, 1, 1, 2, 2, 4 ),
 ( 0.000000000000000000, 0.2499999999999816258, 0.3749999999999713562, 0.4374999999999661937, 0.4687499999999662492, 0.4999999999999663602, 1.000000000000000000 ),
 .UNSPECIFIED. ) ;
#19616 = CARTESIAN_POINT ( 'NONE',  ( -24.08956650204662608, -13.26503430059684518, 5.959546603950007793 ) ) ;
#19617 = CARTESIAN_POINT ( 'NONE',  ( 24.54452541844319668, 14.48555669908156851, 6.079852602000002548 ) ) ;
#19618 = ORIENTED_EDGE ( 'NONE', *, *, #4950, .T. ) ;
#19619 = FACE_OUTER_BOUND ( 'NONE', #31038, .T. ) ;
#19620 = CARTESIAN_POINT ( 'NONE',  ( -24.71725143720000162, -14.18911829940000047, 223.9013449680000178 ) ) ;
#19621 = SHAPE_REPRESENTATION ( 'Cradle Body', ( #17722 ), #28868 ) ;
#19622 = CARTESIAN_POINT ( 'NONE',  ( 25.22625794089999829, -13.26224522399999906, 225.0000014190000002 ) ) ;
#19623 = CARTESIAN_POINT ( 'NONE',  ( -2.158984558600606007, 5.217364672555318883, -57.62652090042499964 ) ) ;
#19624 = EDGE_LOOP ( 'NONE', ( #28050, #15940, #13507, #13385 ) ) ;
#19625 = ADVANCED_FACE ( 'NONE', ( #5016 ), #7222, .F. ) ;
#19626 = EDGE_LOOP ( 'NONE', ( #14561, #15492 ) ) ;
#19627 = DIRECTION ( 'NONE',  ( 0.000000000000000000, 1.000000000000000000, 0.000000000000000000 ) ) ;
#19628 = ORIENTED_EDGE ( 'NONE', *, *, #21019, .T. ) ;
#19629 = ORIENTED_EDGE ( 'NONE', *, *, #24734, .F. ) ;
#19630 = DIRECTION ( 'NONE',  ( 0.000000000000000000, 0.000000000000000000, 1.000000000000000000 ) ) ;
#19631 = CARTESIAN_POINT ( 'NONE',  ( -24.60726957497166367, 14.37955347300500364, 4.098597478000010064 ) ) ;
#19632 = CARTESIAN_POINT ( 'NONE',  ( -1.421085471519999843E-14, -3.552713678799999608E-15, 187.9396849849999853 ) ) ;
#19633 = CARTESIAN_POINT ( 'NONE',  ( 9.816202962829999379, 7.095738861030000066, 231.9999991140000191 ) ) ;
#19634 =( REPRESENTATION_RELATIONSHIP ('NONE','NONE', #2712, #527 ) REPRESENTATION_RELATIONSHIP_WITH_TRANSFORMATION ( #29522 )SHAPE_REPRESENTATION_RELATIONSHIP( ) );
#19635 = CARTESIAN_POINT ( 'NONE',  ( -20.30403093128963476, 20.00000000003735323, 2.600000085000026218 ) ) ;
#19636 = CARTESIAN_POINT ( 'NONE',  ( 3.486358836775546699, -2.566383416802847872, -8.472776792899997744 ) ) ;
#19637 = CARTESIAN_POINT ( 'NONE',  ( 1.057488903014505443E-10, -43.23306002164246564, -10.18642677532906049 ) ) ;
#19638 = ORIENTED_EDGE ( 'NONE', *, *, #157, .T. ) ;
#19639 = CARTESIAN_POINT ( 'NONE',  ( 1.764726261278249497, -3.747269161217322786, -44.10000000002499831 ) ) ;
#19640 = EDGE_CURVE ( 'NONE', #11113, #8540, #25742, .T. ) ;
#19641 = CARTESIAN_POINT ( 'NONE',  ( 0.000000000000000000, 0.000000000000000000, 193.6055512739999926 ) ) ;
#19642 = EDGE_CURVE ( 'NONE', #2704, #10752, #18945, .T. ) ;
#19643 = AXIS2_PLACEMENT_3D ( 'NONE', #4175, #1824, #11412 ) ;
#19644 = CARTESIAN_POINT ( 'NONE',  ( 5.503465972402116435, -2.627571514392686769, -21.48180150030000490 ) ) ;
#19645 = CARTESIAN_POINT ( 'NONE',  ( -12.42573721507907081, -25.75488492242208594, -33.45436474419933148 ) ) ;
#19646 = CARTESIAN_POINT ( 'NONE',  ( 1.100000000000000311, -27.47799119300000470, 225.0964597111326952 ) ) ;
#19647 = ADVANCED_FACE ( 'NONE', ( #14320 ), #21702, .T. ) ;
#19648 = DIRECTION ( 'NONE',  ( 0.000000000000000000, -0.000000000000000000, 1.000000000000000000 ) ) ;
#19649 = DIRECTION ( 'NONE',  ( 0.000000000000000000, 0.000000000000000000, 1.000000000000000000 ) ) ;
#19650 = CARTESIAN_POINT ( 'NONE',  ( -1.460566089872937789, -4.291843709425559261, -46.59520033292501040 ) ) ;
#19651 = EDGE_CURVE ( 'NONE', #15698, #10713, #14685, .T. ) ;
#19652 = CARTESIAN_POINT ( 'NONE',  ( 10.45000000009999930, -27.00000000000000000, -28.39999999989999679 ) ) ;
#19653 = CARTESIAN_POINT ( 'NONE',  ( 3.653275382406361071, -2.426579979385206531, -0.6999999999999992895 ) ) ;
#19654 = DIRECTION ( 'NONE',  ( 0.000000000000000000, 0.000000000000000000, 1.000000000000000000 ) ) ;
#19655 = CARTESIAN_POINT ( 'NONE',  ( -26.55289168650000065, 9.284439999669999111, 229.7313259189999712 ) ) ;
#19656 = CYLINDRICAL_SURFACE ( 'NONE', #5714, 1.099999999999999867 ) ;
#19657 = ORIENTED_EDGE ( 'NONE', *, *, #16171, .T. ) ;
#19658 = CARTESIAN_POINT ( 'NONE',  ( 2.039164074698236906, -5.746172002732055084, -30.85632401679999504 ) ) ;
#19659 = EDGE_CURVE ( 'NONE', #26174, #25831, #22716, .T. ) ;
#19660 = ORIENTED_EDGE ( 'NONE', *, *, #26750, .F. ) ;
#19661 = CARTESIAN_POINT ( 'NONE',  ( 25.16696686177720821, -13.37570800343109312, 3.997190761000024573 ) ) ;
#19662 = CARTESIAN_POINT ( 'NONE',  ( -0.5163256777700186984, 4.538631023554793309, -48.66410749632500199 ) ) ;
#19663 = VERTEX_POINT ( 'NONE', #14155 ) ;
#19664 = VERTEX_POINT ( 'NONE', #7980 ) ;
#19665 = CARTESIAN_POINT ( 'NONE',  ( 0.000000000000000000, 0.000000000000000000, 0.000000000000000000 ) ) ;
#19666 = PRESENTATION_LAYER_ASSIGNMENT (  '', '', ( #2084 ) ) ;
#19667 = ORIENTED_EDGE ( 'NONE', *, *, #13702, .F. ) ;
#19668 = CARTESIAN_POINT ( 'NONE',  ( -7.999999999727707589, -25.79195116312516589, -25.65395878494778259 ) ) ;
#19669 = ORIENTED_EDGE ( 'NONE', *, *, #16138, .T. ) ;
#19670 = CARTESIAN_POINT ( 'NONE',  ( -10.40384843829999895, -24.69832375660000423, -1.291913792900001301 ) ) ;
#19671 = CARTESIAN_POINT ( 'NONE',  ( 2.656656946665528540, 2.398535190088667335, 227.6918569120566360 ) ) ;
#19672 = EDGE_CURVE ( 'NONE', #25555, #90, #4301, .T. ) ;
#19673 = CYLINDRICAL_SURFACE ( 'NONE', #6946, 3.000000000000003997 ) ;
#19674 = DIRECTION ( 'NONE',  ( -1.000000000000000000, 0.000000000000000000, -6.771000000000000128E-12 ) ) ;
#19675 = B_SPLINE_CURVE_WITH_KNOTS ( 'NONE', 3,
 ( #15858, #13967, #13488, #23578, #11294, #13650, #25775, #23104, #10827, #16009, #20414, #11136, #18522, #27645, #6088, #25622, #25300, #28124 ),
 .UNSPECIFIED., .F., .F.,
 ( 4, 2, 2, 2, 2, 2, 2, 2, 4 ),
 ( 0.000000000000000000, 0.1250000000000000000, 0.2500000000000000000, 0.3750000000000000000, 0.5000000000000000000, 0.6250000000000000000, 0.7500000000000000000, 0.8750000000000000000, 1.000000000000000000 ),
 .UNSPECIFIED. ) ;
#19676 = DIRECTION ( 'NONE',  ( 0.000000000000000000, 0.000000000000000000, 1.000000000000000000 ) ) ;
#19677 = CARTESIAN_POINT ( 'NONE',  ( 9.499999999815022633, -16.67216299285837522, -37.76860186073199799 ) ) ;
#19678 = CARTESIAN_POINT ( 'NONE',  ( 3.112737406813101515, -4.802415649948616583, -0.1659393883000001568 ) ) ;
#19679 = CARTESIAN_POINT ( 'NONE',  ( 14.40197535836999876, -32.00000000000000000, -31.28675134584999640 ) ) ;
#19680 = CARTESIAN_POINT ( 'NONE',  ( 0.3986823046148949556, -5.109930552333694642, -10.33088421180000083 ) ) ;
#19681 = CARTESIAN_POINT ( 'NONE',  ( 2.039164074698236906, -5.746172002732055084, -30.25632401680000783 ) ) ;
#19682 = CARTESIAN_POINT ( 'NONE',  ( -1.776356839399999804E-15, -1.776356839399999804E-15, 229.6412452697800006 ) ) ;
#19683 = CARTESIAN_POINT ( 'NONE',  ( 24.81746042555073117, -14.01353061617342455, 6.079865098000015067 ) ) ;
#19684 = CARTESIAN_POINT ( 'NONE',  ( -8.699999998951904345, -14.92844969908904851, -33.25053330396269047 ) ) ;
#19685 = CARTESIAN_POINT ( 'NONE',  ( 6.000000000000000000, -29.96004123392021157, -79.78289277550334191 ) ) ;
#19686 = CARTESIAN_POINT ( 'NONE',  ( 1.127732790480000080, -28.47784299079999926, 225.1040528159999781 ) ) ;
#19687 = CARTESIAN_POINT ( 'NONE',  ( -1.151230282303593366, -4.494053275198268693, -27.54882611460000774 ) ) ;
#19688 = B_SPLINE_SURFACE_WITH_KNOTS ( 'NONE', 5, 5, ( 
 ( #14300, #28755, #7208, #28452, #301, #21217 ),
 ( #4539, #4854, #14453, #9879, #26708, #30973 ),
 ( #5144, #14758, #2032, #24053, #30817, #12081 ),
 ( #21689, #18855, #26102, #14142, #11776, #21382 ),
 ( #7659, #24509, #24357, #5767, #20240, #29689 ),
 ( #10648, #14915, #22000, #756, #29838, #7968 ) ),
 .UNSPECIFIED., .F., .F., .F.,
 ( 6, 6 ),
 ( 6, 6 ),
 ( 0.000000000000000000, 22.42544452799999988 ),
 ( -3.500000000000000000, 3.500000000000000000 ),
 .UNSPECIFIED. ) ;
#19689 = AXIS2_PLACEMENT_3D ( 'NONE', #28891, #16926, #26535 ) ;
#19690 = CARTESIAN_POINT ( 'NONE',  ( 16.07052902885122592, 10.82847174432581028, -1.400000000000001910 ) ) ;
#19691 = DIRECTION ( 'NONE',  ( -4.428977494234582379E-12, -0.8987940462991651502, 0.4383711467890810676 ) ) ;
#19692 = CARTESIAN_POINT ( 'NONE',  ( -0.9592076359448037381, -3.499847752372934995, 230.7617868067715960 ) ) ;
#19693 = ORIENTED_EDGE ( 'NONE', *, *, #11718, .T. ) ;
#19694 = CIRCLE ( 'NONE', #10146, 3.200000004570001888 ) ;
#19695 = VECTOR ( 'NONE', #4612, 1000.000000000000114 ) ;
#19696 = DIRECTION ( 'NONE',  ( 0.000000000000000000, 0.3420201433259318358, -0.9396926207858125046 ) ) ;
#19697 = CARTESIAN_POINT ( 'NONE',  ( -12.40388755362273798, -32.00000000000000000, -27.09135028366836906 ) ) ;
#19698 = VERTEX_POINT ( 'NONE', #5324 ) ;
#19699 = LINE ( 'NONE', #2705, #8792 ) ;
#19700 = CARTESIAN_POINT ( 'NONE',  ( -1.127665019380000189, -28.47796022459999676, 225.0000014190000002 ) ) ;
#19701 = EDGE_CURVE ( 'NONE', #29499, #16422, #3110, .T. ) ;
#19702 = ORIENTED_EDGE ( 'NONE', *, *, #10698, .T. ) ;
#19703 = CARTESIAN_POINT ( 'NONE',  ( -4.469433717901757142, 1.081650411600142414, -44.10000000002499831 ) ) ;
#19704 = VERTEX_POINT ( 'NONE', #22316 ) ;
#19705 = ORIENTED_EDGE ( 'NONE', *, *, #23945, .T. ) ;
#19706 = EDGE_CURVE ( 'NONE', #28783, #21131, #11667, .T. ) ;
#19707 =( NAMED_UNIT ( * ) SI_UNIT ( $, .STERADIAN. ) SOLID_ANGLE_UNIT ( ) );
#19708 = ORIENTED_EDGE ( 'NONE', *, *, #4608, .F. ) ;
#19709 = CARTESIAN_POINT ( 'NONE',  ( 27.29823224880000154, 3.129650177539999281E-14, 230.6577119970000069 ) ) ;
#19710 = ADVANCED_FACE ( 'NONE', ( #1071 ), #24980, .F. ) ;
#19711 = EDGE_CURVE ( 'NONE', #23898, #55, #8795, .T. ) ;
#19712 = CIRCLE ( 'NONE', #23737, 2.999999999999999556 ) ;
#19713 = CARTESIAN_POINT ( 'NONE',  ( 23.81569860410000317, -13.75000000000000000, 3.900000000369999942 ) ) ;
#19714 = CARTESIAN_POINT ( 'NONE',  ( -7.707106507371444870, -5.692566414263196428, -27.29492500646317765 ) ) ;
#19715 = ORIENTED_EDGE ( 'NONE', *, *, #30240, .T. ) ;
#19716 = CARTESIAN_POINT ( 'NONE',  ( -24.54884434681058991, 13.04717673392247690, 6.002806401000010617 ) ) ;
#19717 = AXIS2_PLACEMENT_3D ( 'NONE', #8286, #17881, #27486 ) ;
#19718 = PLANE ( 'NONE',  #24096 ) ;
#19719 = DIRECTION ( 'NONE',  ( 0.7198537139083028835, -0.6941258031311204890, 0.000000000000000000 ) ) ;
#19720 = CARTESIAN_POINT ( 'NONE',  ( 10.69999999999999929, -30.49251257979999963, -21.04205368479999905 ) ) ;
#19721 = VERTEX_POINT ( 'NONE', #12870 ) ;
#19722 = CARTESIAN_POINT ( 'NONE',  ( 7.638687372243864182, -5.597492073922072819, -34.74908987243156133 ) ) ;
#19723 = CARTESIAN_POINT ( 'NONE',  ( 1.403799475828179766, 5.569137675590418723, -17.05080441500000177 ) ) ;
#19724 = DIRECTION ( 'NONE',  ( 1.000000000000000000, 0.000000000000000000, 0.000000000000000000 ) ) ;
#19725 = CARTESIAN_POINT ( 'NONE',  ( -8.699999999724179034, -29.73863906514459643, -27.17531388891805477 ) ) ;
#19726 = DIRECTION ( 'NONE',  ( 0.000000000000000000, -2.257145581549999994E-12, -1.000000000000000000 ) ) ;
#19727 = CARTESIAN_POINT ( 'NONE',  ( 0.5890437901233029905, -28.49417040867363227, 3.901346086000012647 ) ) ;
#19728 = CARTESIAN_POINT ( 'NONE',  ( -10.99999999969999998, 20.99999999999999645, -70.09999999999999432 ) ) ;
#19729 = CARTESIAN_POINT ( 'NONE',  ( -10.69999999989999928, -45.00000000000000000, -7.274962170800002070 ) ) ;
#19730 = DIRECTION ( 'NONE',  ( 0.000000000000000000, 0.000000000000000000, 1.000000000000000000 ) ) ;
#19731 = CARTESIAN_POINT ( 'NONE',  ( 24.75549318700000256, 13.74789704510000021, 229.4485677049999879 ) ) ;
#19732 = CARTESIAN_POINT ( 'NONE',  ( -7.747012534260000471, -16.51919209409999922, 230.6999999999999886 ) ) ;
#19733 = ORIENTED_EDGE ( 'NONE', *, *, #1809, .F. ) ;
#19734 = CARTESIAN_POINT ( 'NONE',  ( -4.890954027197769172, -0.1236851485019374169, -52.80673954922500712 ) ) ;
#19735 = AXIS2_PLACEMENT_3D ( 'NONE', #14230, #21468, #9341 ) ;
#19736 = LINE ( 'NONE', #27120, #5759 ) ;
#19737 = B_SPLINE_CURVE_WITH_KNOTS ( 'NONE', 3,
 ( #22525, #3617, #18085, #6136, #29746, #8174, #13211, #15732, #25346, #3786, #6763, #1743, #15898, #9270 ),
 .UNSPECIFIED., .F., .F.,
 ( 4, 2, 2, 1, 1, 2, 2, 4 ),
 ( 0.000000000000000000, 0.2500000000000099365, 0.3750000000000136002, 0.4375000000000135447, 0.4687500000000111022, 0.4843750000000072164, 0.5000000000000033307, 1.000000000000000000 ),
 .UNSPECIFIED. ) ;
#19738 = CARTESIAN_POINT ( 'NONE',  ( -18.50495978135909425, 20.74626080782525506, 0.9999999989999952543 ) ) ;
#19739 = CARTESIAN_POINT ( 'NONE',  ( -4.773704105810320897, 0.4428995197802990669, -68.10000000002500542 ) ) ;
#19740 = VERTEX_POINT ( 'NONE', #1226 ) ;
#19741 = CARTESIAN_POINT ( 'NONE',  ( 3.542914729026319876, 0.003443490030938245461, -88.52261276241732446 ) ) ;
#19742 = APPLICATION_PROTOCOL_DEFINITION ( 'draft international standard', 'automotive_design', 1998, #28456 ) ;
#19743 = ORIENTED_EDGE ( 'NONE', *, *, #5377, .F. ) ;
#19744 = CARTESIAN_POINT ( 'NONE',  ( 23.90286779624927149, 15.52112777353848294, 5.560535498006014876 ) ) ;
#19745 = CARTESIAN_POINT ( 'NONE',  ( -3.040504021322313122, -1.733590290792417887, -0.5999999999999894307 ) ) ;
#19746 = ORIENTED_EDGE ( 'NONE', *, *, #23671, .T. ) ;
#19747 = CARTESIAN_POINT ( 'NONE',  ( -4.555585884337687297, -4.059738318096004939, -25.44101932449999026 ) ) ;
#19748 = CARTESIAN_POINT ( 'NONE',  ( 10.69999999999999929, -27.00000000000000000, -28.40000000000000213 ) ) ;
#19749 = CARTESIAN_POINT ( 'NONE',  ( -26.19983009839024035, 8.854867600185624354, -0.6999999999999784173 ) ) ;
#19750 = CARTESIAN_POINT ( 'NONE',  ( -23.86403265525339634, -13.66628296766671546, 3.900000000001122569 ) ) ;
#19751 = AXIS2_PLACEMENT_3D ( 'NONE', #2616, #12208, #19145 ) ;
#19752 = LINE ( 'NONE', #22264, #15433 ) ;
#19753 = CARTESIAN_POINT ( 'NONE',  ( -7.999999999668208517, -9.149979920084513552, -35.02638174925785819 ) ) ;
#19754 = VERTEX_POINT ( 'NONE', #15227 ) ;
#19755 = UNCERTAINTY_MEASURE_WITH_UNIT (LENGTH_MEASURE( 1.000000000000000082E-05 ), #17783, 'distance_accuracy_value', 'NONE');
#19756 = CARTESIAN_POINT ( 'NONE',  ( -10.69999999999999929, -24.87867968679999819, -26.27867968680000033 ) ) ;
#19757 = LINE ( 'NONE', #31097, #20054 ) ;
#19758 = VERTEX_POINT ( 'NONE', #27340 ) ;
#19759 = CARTESIAN_POINT ( 'NONE',  ( -27.92857142860000152, 3.552713678799999608E-15, 87.93968498540000667 ) ) ;
#19760 = ADVANCED_FACE ( 'NONE', ( #24832, #2963 ), #12556, .T. ) ;
#19761 = DIRECTION ( 'NONE',  ( 1.000000000000000000, 1.601966730286663379E-12, 3.582312748438143944E-12 ) ) ;
#19762 = CARTESIAN_POINT ( 'NONE',  ( -12.18429361160000113, -1.640523776660000044, 232.6627643349999914 ) ) ;
#19763 = CARTESIAN_POINT ( 'NONE',  ( -3.873164306258084277, -2.119290473559455101, -95.69213427732501032 ) ) ;
#19764 = CARTESIAN_POINT ( 'NONE',  ( 0.000000000000000000, 0.000000000000000000, 42.06031501460000044 ) ) ;
#19765 = CARTESIAN_POINT ( 'NONE',  ( 10.69999999999035722, -129.5232638600235759, -38.12979645447560983 ) ) ;
#19766 = CARTESIAN_POINT ( 'NONE',  ( 3.164224794202841640, -2.738734268234706448, -0.6999999999999992895 ) ) ;
#19767 = CARTESIAN_POINT ( 'NONE',  ( 13.99313239240532525, -26.86047011600456713, -0.6577119969999878357 ) ) ;
#19768 = CARTESIAN_POINT ( 'NONE',  ( 0.8790546033401771542, -27.48597397634632955, 4.334666192900195725 ) ) ;
#19769 = VECTOR ( 'NONE', #3169, 1000.000000000000000 ) ;
#19770 = CARTESIAN_POINT ( 'NONE',  ( -9.707106781189999367, -55.00000000000000000, -43.10710678118599759 ) ) ;
#19771 = CARTESIAN_POINT ( 'NONE',  ( -7.999999999681125296, -14.69158818474954487, -33.36927661519188604 ) ) ;
#19773 = EDGE_CURVE ( 'NONE', #16461, #11358, #17275, .T. ) ;
#19772 = CIRCLE ( 'NONE', #22769, 28.50000000000000000 ) ;
#19774 = CARTESIAN_POINT ( 'NONE',  ( -9.339631244007748023, -25.12005762863060454, 25.40686791475853568 ) ) ;
#19775 = CARTESIAN_POINT ( 'NONE',  ( -0.3682501489410162088, -27.79783598715885518, 5.680150179000031940 ) ) ;
#19776 = AXIS2_PLACEMENT_3D ( 'NONE', #12503, #20061, #870 ) ;
#19777 = VERTEX_POINT ( 'NONE', #8128 ) ;
#19778 = CARTESIAN_POINT ( 'NONE',  ( 11.04680313989999796, -24.61949705740000027, -1.636966775500001248 ) ) ;
#19779 = CARTESIAN_POINT ( 'NONE',  ( 24.12694114270000156, -13.81062811039999971, 226.0959682270000144 ) ) ;
#19780 = CARTESIAN_POINT ( 'NONE',  ( -4.880917369133354278, -2.481566535878938495, -63.16424626872499459 ) ) ;
#19781 = VERTEX_POINT ( 'NONE', #10205 ) ;
#19782 = ORIENTED_EDGE ( 'NONE', *, *, #28090, .F. ) ;
#19783 = CARTESIAN_POINT ( 'NONE',  ( 8.999999999799999983, 21.34999999950001026, -70.09999999999999432 ) ) ;
#19784 = ORIENTED_EDGE ( 'NONE', *, *, #25062, .T. ) ;
#19785 = EDGE_CURVE ( 'NONE', #4261, #6141, #17430, .T. ) ;
#19786 = ORIENTED_EDGE ( 'NONE', *, *, #24765, .T. ) ;
#19787 = CIRCLE ( 'NONE', #14754, 28.50000000000000000 ) ;
#19788 = CARTESIAN_POINT ( 'NONE',  ( -0.5667420186473062227, 2.989789856359415410, -42.27519293845822546 ) ) ;
#19789 = AXIS2_PLACEMENT_3D ( 'NONE', #14198, #28040, #18909 ) ;
#19790 = CARTESIAN_POINT ( 'NONE',  ( -24.74993094845043018, 14.13250375615880117, 3.957489350000009676 ) ) ;
#19791 = CARTESIAN_POINT ( 'NONE',  ( -28.55928429112321609, 2.998940805198770043, 8.000000000000007105 ) ) ;
#19792 = AXIS2_PLACEMENT_3D ( 'NONE', #15829, #9049, #30300 ) ;
#19793 = CARTESIAN_POINT ( 'NONE',  ( 11.05690487959999935, -4.834698001819999647, 231.9999991140000191 ) ) ;
#19794 = CARTESIAN_POINT ( 'NONE',  ( 10.69999999996684004, -29.94035316038524641, -27.70911855536421697 ) ) ;
#19795 = CARTESIAN_POINT ( 'NONE',  ( -4.184186767956295405, -1.312611723764782523, -10.02323088899999881 ) ) ;
#19796 = LINE ( 'NONE', #9724, #21568 ) ;
#19797 = VERTEX_POINT ( 'NONE', #17726 ) ;
#19798 = CARTESIAN_POINT ( 'NONE',  ( 2.710954907126704061, -3.448654721267146783, -44.10000000002499831 ) ) ;
#19799 = CARTESIAN_POINT ( 'NONE',  ( 24.98081130624543889, 13.71897605842228529, 4.895818164000031558 ) ) ;
#19800 = CARTESIAN_POINT ( 'NONE',  ( -5.611385130160316592, 1.726552310816597435, -23.32289663400000990 ) ) ;
#19801 = CARTESIAN_POINT ( 'NONE',  ( -24.07583586439999834, -13.90018868249999962, 226.1000014189999945 ) ) ;
#19802 = CARTESIAN_POINT ( 'NONE',  ( 2.131628207279999844E-14, 1.421085471519999843E-14, 231.6999999999999886 ) ) ;
#19803 = CARTESIAN_POINT ( 'NONE',  ( 26.80000000069999899, -3.281945028320000125E-15, 18.39142920540000148 ) ) ;
#19804 = CARTESIAN_POINT ( 'NONE',  ( 4.531630834892029114, -0.6723478992683162847, -45.73818262062500395 ) ) ;
#19805 = ADVANCED_FACE ( 'NONE', ( #15381 ), #7636, .F. ) ;
#19806 = SHAPE_REPRESENTATION ( 'Catch Spring', ( #17722 ), #23393 ) ;
#19807 = CARTESIAN_POINT ( 'NONE',  ( -10.69999999999999929, -122.9701038226999827, -31.65529867039999701 ) ) ;
#19808 = CARTESIAN_POINT ( 'NONE',  ( -26.80000000069999899, 3.281945028329999726E-15, 142.8898184869999852 ) ) ;
#19809 = CARTESIAN_POINT ( 'NONE',  ( -19.28886814869914801, 20.00013610278432807, 230.3850219899306921 ) ) ;
#19810 = DIRECTION ( 'NONE',  ( -0.000000000000000000, 0.000000000000000000, -1.000000000000000000 ) ) ;
#19811 = AXIS2_PLACEMENT_3D ( 'NONE', #22440, #5894, #12984 ) ;
#19812 = VECTOR ( 'NONE', #588, 1000.000000000000000 ) ;
#19813 = AXIS2_PLACEMENT_3D ( 'NONE', #22211, #15123, #29437 ) ;
#19814 = CARTESIAN_POINT ( 'NONE',  ( 4.421808970600630495, -26.43392618132180871, 20.40072977778958219 ) ) ;
#19815 = ORIENTED_EDGE ( 'NONE', *, *, #23724, .F. ) ;
#19816 = AXIS2_PLACEMENT_3D ( 'NONE', #19641, #10199, #24206 ) ;
#19817 = CARTESIAN_POINT ( 'NONE',  ( -5.305719984766040120, 1.510612064730647131, -32.30158078970000446 ) ) ;
#19818 = VERTEX_POINT ( 'NONE', #7672 ) ;
#19819 = EDGE_CURVE ( 'NONE', #29443, #27611, #19283, .T. ) ;
#19820 = CARTESIAN_POINT ( 'NONE',  ( 25.46368747440213198, -12.80129684534102807, 4.999998581000003384 ) ) ;
#19821 = CARTESIAN_POINT ( 'NONE',  ( -3.250950776947245213, -3.159825117472807143, -47.20083066912499703 ) ) ;
#19822 = ORIENTED_EDGE ( 'NONE', *, *, #1016, .T. ) ;
#19823 = ORIENTED_EDGE ( 'NONE', *, *, #27247, .T. ) ;
#19824 = EDGE_CURVE ( 'NONE', #18702, #14604, #9922, .T. ) ;
#19825 = DIRECTION ( 'NONE',  ( 0.2384969955249491846, -0.4130889137015296142, -0.8789065550457922926 ) ) ;
#19826 = ORIENTED_EDGE ( 'NONE', *, *, #9649, .T. ) ;
#19827 = ORIENTED_EDGE ( 'NONE', *, *, #18864, .T. ) ;
#19828 = MECHANICAL_DESIGN_GEOMETRIC_PRESENTATION_REPRESENTATION (  '', ( #30882 ), #4761 ) ;
#19829 = PLANE ( 'NONE',  #30654 ) ;
#19830 = EDGE_CURVE ( 'NONE', #2860, #21717, #16207, .T. ) ;
#19831 = CARTESIAN_POINT ( 'NONE',  ( 25.80996960090668679, 10.85703805089278617, 1.000000000000000888 ) ) ;
#19832 = CARTESIAN_POINT ( 'NONE',  ( -2.664535259099999568E-14, -26.80000000000000071, 115.0000000000000000 ) ) ;
#19833 = ADVANCED_FACE ( 'NONE', ( #8439 ), #8922, .T. ) ;
#19834 = CARTESIAN_POINT ( 'NONE',  ( -3.552713678799999608E-15, 0.000000000000000000, 93.21714158839999698 ) ) ;
#19835 = CARTESIAN_POINT ( 'NONE',  ( -4.364338366759058729, 2.011379601984358612, -0.6999999999999991784 ) ) ;
#19836 = DIRECTION ( 'NONE',  ( 0.000000000000000000, 0.000000000000000000, 1.000000000000000000 ) ) ;
#19837 = AXIS2_PLACEMENT_3D ( 'NONE', #16819, #19654, #26580 ) ;
#19838 = CARTESIAN_POINT ( 'NONE',  ( -23.73536387410678117, -14.47423183427071258, 224.1131743014709627 ) ) ;
#19839 = AXIS2_PLACEMENT_3D ( 'NONE', #28044, #16089, #25701 ) ;
#19840 = CARTESIAN_POINT ( 'NONE',  ( 3.981471518793421538, 3.199610153647690414, -9.292086407999997633 ) ) ;
#19841 = CARTESIAN_POINT ( 'NONE',  ( 2.022420680230010870, -3.847796821814265300, -32.70721934060000535 ) ) ;
#19842 = AXIS2_PLACEMENT_3D ( 'NONE', #4286, #21271, #1613 ) ;
#19843 = LINE ( 'NONE', #23098, #17310 ) ;
#19844 = ADVANCED_FACE ( 'NONE', ( #1696, #27808 ), #15686, .T. ) ;
#19845 = CARTESIAN_POINT ( 'NONE',  ( 24.37165445055180157, -14.77472140295711434, 5.104215870000011535 ) ) ;
#19846 = CARTESIAN_POINT ( 'NONE',  ( 18.31101511981528773, 19.88193408480103486, 0.02162463700000616385 ) ) ;
#19847 = CARTESIAN_POINT ( 'NONE',  ( -23.81569860410000317, -13.75000000000000000, 3.900000000369999942 ) ) ;
#19848 = CARTESIAN_POINT ( 'NONE',  ( -8.000000000050450311, -115.5267901941129907, 21.04701626955636939 ) ) ;
#19849 = CARTESIAN_POINT ( 'NONE',  ( -4.188726303739433554, 1.192588472141202560, -31.30158078970000801 ) ) ;
#19850 = CARTESIAN_POINT ( 'NONE',  ( 9.999999999967510433, -24.00000000000000355, -28.00651183392525567 ) ) ;
#19851 = CARTESIAN_POINT ( 'NONE',  ( 14.83319110805087071, -24.98846848000023613, -23.78818000047916925 ) ) ;
#19852 = FACE_OUTER_BOUND ( 'NONE', #29603, .T. ) ;
#19853 = AXIS2_PLACEMENT_3D ( 'NONE', #19133, #7174, #16919 ) ;
#19854 = EDGE_LOOP ( 'NONE', ( #3962, #4256, #27172, #4770, #14523 ) ) ;
#19855 = COLOUR_RGB ( '', 0.72549020, 0.75294118, 0.79215686) ;
#19856 = EDGE_CURVE ( 'NONE', #26528, #16525, #19675, .T. ) ;
#19857 = CARTESIAN_POINT ( 'NONE',  ( -17.93324555120827668, 10.97998838178171432, -1.000005633855494125E-09 ) ) ;
#19858 = CARTESIAN_POINT ( 'NONE',  ( -3.982632971385688947, -19.71206033698065596, -27.86495495700036784 ) ) ;
#19859 = VERTEX_POINT ( 'NONE', #3734 ) ;
#19860 = B_SPLINE_CURVE_WITH_KNOTS ( 'NONE', 5,
 ( #17803, #3815, #1612, #13402, #27262, #17952, #3489, #13085, #3969, #5851, #6328, #18115, #994, #11202, #25058 ),
 .UNSPECIFIED., .F., .F.,
 ( 6, 3, 3, 3, 6 ),
 ( 0.000000000000000000, 0.1000000000005725753, 0.4000000000022904123, 0.6999999999994271915, 1.000000000000000000 ),
 .UNSPECIFIED. ) ;
#19861 = CARTESIAN_POINT ( 'NONE',  ( 2.220446049249999755E-16, 2.100000000000000089, 226.6412452697800006 ) ) ;
#19862 = CARTESIAN_POINT ( 'NONE',  ( -8.699999999693382335, -26.29778505801089850, -31.34318562240535044 ) ) ;
#19863 = ORIENTED_EDGE ( 'NONE', *, *, #12289, .F. ) ;
#19864 = CARTESIAN_POINT ( 'NONE',  ( 7.217190561760000733, 9.649559097600000968, 230.6412452697800006 ) ) ;
#19865 = AXIS2_PLACEMENT_3D ( 'NONE', #15621, #28206, #23187 ) ;
#19866 = ORIENTED_EDGE ( 'NONE', *, *, #27460, .F. ) ;
#19867 = ORIENTED_EDGE ( 'NONE', *, *, #23852, .T. ) ;
#19868 = ORIENTED_EDGE ( 'NONE', *, *, #13147, .T. ) ;
#19869 = CARTESIAN_POINT ( 'NONE',  ( 28.45771199710000232, 4.805544668949999654, 229.4982322489999831 ) ) ;
#19870 = CARTESIAN_POINT ( 'NONE',  ( -17.78435532386814799, -9.571375077557558342, -0.6999999999999785283 ) ) ;
#19871 = CARTESIAN_POINT ( 'NONE',  ( -10.69999999999999929, -24.95051674469999980, -26.20881489450000146 ) ) ;
#19872 = VERTEX_POINT ( 'NONE', #20733 ) ;
#19873 = CARTESIAN_POINT ( 'NONE',  ( 17.93011078763067090, 11.79183908526299085, -0.6999999989999727834 ) ) ;
#19874 = CARTESIAN_POINT ( 'NONE',  ( -28.49528339128749366, -0.5184828350247797646, 1.000000000000000888 ) ) ;
#19875 = DIRECTION ( 'NONE',  ( -3.582312748438143944E-12, 0.000000000000000000, 1.000000000000000000 ) ) ;
#19876 = AXIS2_PLACEMENT_3D ( 'NONE', #28950, #330, #14641 ) ;
#19877 = CARTESIAN_POINT ( 'NONE',  ( 24.04107748430000058, -13.95955969929999974, 223.9013459049999994 ) ) ;
#19878 = CARTESIAN_POINT ( 'NONE',  ( -3.665401116828205463, 4.874126016103034864, -19.63064294430000345 ) ) ;
#19879 = CARTESIAN_POINT ( 'NONE',  ( -21.30888436558563370, -16.34772642260384146, 193.2171415879999756 ) ) ;
#19880 = ADVANCED_FACE ( 'NONE', ( #30334 ), #20898, .F. ) ;
#19881 = CARTESIAN_POINT ( 'NONE',  ( -8.699999999703425857, -29.80249410822303346, -29.47052640025896508 ) ) ;
#19882 = B_SPLINE_CURVE_WITH_KNOTS ( 'NONE', 3,
 ( #18374, #13492, #23109, #18526, #20900, #25777, #1548, #30499, #27969, #11453 ),
 .UNSPECIFIED., .F., .F.,
 ( 4, 2, 2, 2, 4 ),
 ( 0.000000000000000000, 0.2500000000000000000, 0.5000000000000000000, 0.7500000000000000000, 1.000000000000000000 ),
 .UNSPECIFIED. ) ;
#19883 = DIRECTION ( 'NONE',  ( 0.000000000000000000, -1.000000000000000000, 2.257145581549999994E-12 ) ) ;
#19884 = DIRECTION ( 'NONE',  ( 0.000000000000000000, 0.000000000000000000, 1.000000000000000000 ) ) ;
#19885 = CARTESIAN_POINT ( 'NONE',  ( 8.999999999770000869, 20.87254207907673731, -44.59478429471910488 ) ) ;
#19886 = ADVANCED_FACE ( 'NONE', ( #27967 ), #13333, .T. ) ;
#19887 = EDGE_CURVE ( 'NONE', #11806, #15540, #5786, .T. ) ;
#19888 = CARTESIAN_POINT ( 'NONE',  ( 8.999999999770000869, 21.35000000040000145, -51.10000000000000142 ) ) ;
#19889 = CARTESIAN_POINT ( 'NONE',  ( -11.62710820939999934, -24.17108566160000294, -1.401657795899999392 ) ) ;
#19890 = CARTESIAN_POINT ( 'NONE',  ( -7.999999999711121745, -29.94262568603332042, -29.10368078042601780 ) ) ;
#19891 = ORIENTED_EDGE ( 'NONE', *, *, #30162, .T. ) ;
#19892 = CARTESIAN_POINT ( 'NONE',  ( -1.650988191866312516, 3.989749455477759721, -56.74652090042498997 ) ) ;
#19893 = CARTESIAN_POINT ( 'NONE',  ( -12.30800288698999978, -24.60220466956999985, -24.01086508779000184 ) ) ;
#19894 = CARTESIAN_POINT ( 'NONE',  ( -4.012761316119771493, 1.782282071307969673, -38.34844621931605957 ) ) ;
#19895 = CARTESIAN_POINT ( 'NONE',  ( -4.269058662706476603, 1.003599612145581021, -68.10000000002500542 ) ) ;
#19896 = ORIENTED_EDGE ( 'NONE', *, *, #1563, .T. ) ;
#19897 = CARTESIAN_POINT ( 'NONE',  ( -2.299520702359473923, 1.810397285033877646, -95.04696119083976669 ) ) ;
#19898 = B_SPLINE_CURVE_WITH_KNOTS ( 'NONE', 3,
 ( #26106, #26257, #4695, #17264, #26871, #10503 ),
 .UNSPECIFIED., .F., .F.,
 ( 4, 2, 4 ),
 ( 0.000000000000000000, 0.5000000000000000000, 1.000000000000000000 ),
 .UNSPECIFIED. ) ;
#19899 = ORIENTED_EDGE ( 'NONE', *, *, #20258, .T. ) ;
#19900 = PLANE ( 'NONE',  #11463 ) ;
#19901 = CARTESIAN_POINT ( 'NONE',  ( -8.000000000022961189, -117.2164086036294890, 17.00415548048141545 ) ) ;
#19902 = EDGE_LOOP ( 'NONE', ( #26701, #5680, #6512, #5482 ) ) ;
#19903 = CARTESIAN_POINT ( 'NONE',  ( 1.094823181362614140, 5.872682718251108547, -63.42744533522500205 ) ) ;
#19904 = CARTESIAN_POINT ( 'NONE',  ( -26.94142135619999934, 1.207922650790000128E-13, 230.0000000000000000 ) ) ;
#19905 = CARTESIAN_POINT ( 'NONE',  ( 0.4446548587409490660, -4.237356817840251644, -67.77495035202500162 ) ) ;
#19906 = CARTESIAN_POINT ( 'NONE',  ( 17.16657240420000008, 12.09999999999999964, -1.452769935612311825 ) ) ;
#19907 = CARTESIAN_POINT ( 'NONE',  ( -27.07233446881492611, 8.380004974212880597, 1.000000000000000888 ) ) ;
#19908 = ORIENTED_EDGE ( 'NONE', *, *, #28548, .T. ) ;
#19909 = CARTESIAN_POINT ( 'NONE',  ( 17.00259495252183228, -7.902801559240212548, -4.336808689942018722E-16 ) ) ;
#19910 = B_SPLINE_CURVE_WITH_KNOTS ( 'NONE', 3,
 ( #10619, #6367, #25729, #6047, #1501, #3530 ),
 .UNSPECIFIED., .F., .F.,
 ( 4, 2, 4 ),
 ( 0.000000000000000000, 0.5000000000000000000, 1.000000000000000000 ),
 .UNSPECIFIED. ) ;
#19911 = DIRECTION ( 'NONE',  ( 1.000000000000000000, -9.219999999999999084E-13, 4.710999999999999616E-12 ) ) ;
#19912 = ORIENTED_EDGE ( 'NONE', *, *, #4741, .T. ) ;
#19913 = CARTESIAN_POINT ( 'NONE',  ( 3.455669901342143024, 1.014542102255497902, 227.7047085156410162 ) ) ;
#19914 = FACE_OUTER_BOUND ( 'NONE', #29565, .T. ) ;
#19915 = FACE_OUTER_BOUND ( 'NONE', #7001, .T. ) ;
#19917 = EDGE_CURVE ( 'NONE', #25371, #25254, #9080, .T. ) ;
#19916 = CARTESIAN_POINT ( 'NONE',  ( -1.823119173631714274, -0.2505752385364682366, -97.85464525912570366 ) ) ;
#19918 = CARTESIAN_POINT ( 'NONE',  ( 23.51325844009999955, -14.83130343779999905, 224.7916311099999973 ) ) ;
#19919 = CARTESIAN_POINT ( 'NONE',  ( -8.699999999737658030, -25.77531388886905006, -25.66136093486021608 ) ) ;
#19920 = CARTESIAN_POINT ( 'NONE',  ( 1.035314575941623572, -3.725342087822672621, -0.6999999999999994005 ) ) ;
#19921 = DIRECTION ( 'NONE',  ( 1.000000000000000000, 0.000000000000000000, 0.000000000000000000 ) ) ;
#19923 = EDGE_CURVE ( 'NONE', #29481, #11688, #17050, .T. ) ;
#19922 = CARTESIAN_POINT ( 'NONE',  ( -3.982632971385688947, -19.71206033680530822, -27.86495495664085098 ) ) ;
#19924 = CYLINDRICAL_SURFACE ( 'NONE', #18796, 2.000000000000002665 ) ;
#19925 = CARTESIAN_POINT ( 'NONE',  ( 17.70297572282393617, 11.97108418938390884, 1.385610376436474414E-13 ) ) ;
#19926 = CARTESIAN_POINT ( 'NONE',  ( -25.04491701902130174, -9.543388590360494916, 93.21714158838632613 ) ) ;
#19927 = CARTESIAN_POINT ( 'NONE',  ( -0.3000709590196222187, -27.79870762326714484, 5.759626916000016195 ) ) ;
#19928 = VERTEX_POINT ( 'NONE', #7346 ) ;
#19929 = DIRECTION ( 'NONE',  ( 1.000000000000000000, 0.000000000000000000, 0.000000000000000000 ) ) ;
#19930 = CARTESIAN_POINT ( 'NONE',  ( 11.69999999989999928, -2.055600358200002198, -0.6999999999999992895 ) ) ;
#19931 = CARTESIAN_POINT ( 'NONE',  ( 1.494712469390715892, 4.699749685697345747, -61.21492395752499505 ) ) ;
#19932 = ORIENTED_EDGE ( 'NONE', *, *, #5449, .T. ) ;
#19933 = ORIENTED_EDGE ( 'NONE', *, *, #8806, .F. ) ;
#19934 = CARTESIAN_POINT ( 'NONE',  ( 8.700000000290945223, -18.27255887617201324, -40.96732049143839305 ) ) ;
#19935 = EDGE_LOOP ( 'NONE', ( #16216, #29472, #14727, #2825 ) ) ;
#19936 = ORIENTED_EDGE ( 'NONE', *, *, #16949, .F. ) ;
#19937 = DIRECTION ( 'NONE',  ( 0.000000000000000000, 0.000000000000000000, 1.000000000000000000 ) ) ;
#19938 = EDGE_CURVE ( 'NONE', #11502, #4065, #26083, .T. ) ;
#19939 = CARTESIAN_POINT ( 'NONE',  ( 28.50000000000000000, 1.065814103639999922E-14, 229.0000000000000000 ) ) ;
#19940 = CARTESIAN_POINT ( 'NONE',  ( -25.01590170629258481, -13.65607539363486822, 224.1109849693008584 ) ) ;
#19941 = FACE_OUTER_BOUND ( 'NONE', #11152, .T. ) ;
#19942 = DIRECTION ( 'NONE',  ( 1.000000000000000000, -1.224606353819999829E-16, 0.000000000000000000 ) ) ;
#19943 = CARTESIAN_POINT ( 'NONE',  ( -25.14597776469364732, -15.02549348228339454, 8.000000000000007105 ) ) ;
#19944 = ORIENTED_EDGE ( 'NONE', *, *, #30631, .T. ) ;
#19945 = CARTESIAN_POINT ( 'NONE',  ( 2.852669508774048790, -3.465077913054150471, -44.10000000002499121 ) ) ;
#19946 = CARTESIAN_POINT ( 'NONE',  ( 8.350000000049549342, -115.5267901939647857, 21.04701626999854369 ) ) ;
#19947 = AXIS2_PLACEMENT_3D ( 'NONE', #411, #21958, #4817 ) ;
#19948 = CARTESIAN_POINT ( 'NONE',  ( -2.554946692801202346, -3.999086378171832212, -22.64641267860000085 ) ) ;
#19949 = CARTESIAN_POINT ( 'NONE',  ( -12.40047914202865620, -23.38968038405745276, -32.08884053860782615 ) ) ;
#19950 = CARTESIAN_POINT ( 'NONE',  ( 13.99999999979999821, 21.69999999929999390, -67.09999999999999432 ) ) ;
#19951 = VECTOR ( 'NONE', #15173, 1000.000000000000000 ) ;
#19952 = CARTESIAN_POINT ( 'NONE',  ( 9.999999999966984632, -29.92191803010020834, -29.18524365260708819 ) ) ;
#19953 = CARTESIAN_POINT ( 'NONE',  ( 8.700000000272730460, -17.14815999457695028, -33.31467482405556524 ) ) ;
#19954 = CARTESIAN_POINT ( 'NONE',  ( 3.314820598666778917, -5.455691467570147779, -46.08669147682499556 ) ) ;
#19955 = FACE_OUTER_BOUND ( 'NONE', #11645, .T. ) ;
#19956 = CARTESIAN_POINT ( 'NONE',  ( -1.289604807081810911, 1.680165884098436591, 226.6412452697800006 ) ) ;
#19957 = FACE_OUTER_BOUND ( 'NONE', #26971, .T. ) ;
#19958 = DIRECTION ( 'NONE',  ( 0.000000000000000000, -1.000000000000000000, 0.000000000000000000 ) ) ;
#19959 = CARTESIAN_POINT ( 'NONE',  ( 24.25955693124982915, -12.95188430838311078, 225.6425104787478517 ) ) ;
#19960 = ORIENTED_EDGE ( 'NONE', *, *, #6352, .T. ) ;
#19961 = PRODUCT_DEFINITION_SHAPE ( 'NONE', 'NONE',  #31123 ) ;
#19962 = CARTESIAN_POINT ( 'NONE',  ( 1.456545767631101107, -4.104408573385627257, -30.25632401680000783 ) ) ;
#19963 = ORIENTED_EDGE ( 'NONE', *, *, #1348, .F. ) ;
#19964 = CARTESIAN_POINT ( 'NONE',  ( -8.699999999681903518, -14.92844969908904851, -33.25053330396269047 ) ) ;
#19965 = CARTESIAN_POINT ( 'NONE',  ( -0.9106536557335528359, 5.366613064751446949, -52.05792092402499804 ) ) ;
#19966 = ORIENTED_EDGE ( 'NONE', *, *, #11254, .T. ) ;
#19967 = EDGE_LOOP ( 'NONE', ( #24224, #19746, #27659, #23270, #10452, #28762 ) ) ;
#19968 = EDGE_CURVE ( 'NONE', #26590, #18614, #16266, .T. ) ;
#19969 = COLOUR_RGB ( '', 0.72549020, 0.75294118, 0.79215686) ;
#19970 = VERTEX_POINT ( 'NONE', #18833 ) ;
#19971 = EDGE_LOOP ( 'NONE', ( #26904, #19358, #4567, #12152, #1280, #7128, #29017, #13498 ) ) ;
#19972 = CARTESIAN_POINT ( 'NONE',  ( -11.51411769270000107, -24.20066399839999960, -0.7084723282999999538 ) ) ;
#19973 = CARTESIAN_POINT ( 'NONE',  ( -17.78435532361610782, 10.42862492215759573, -0.6999999999999785283 ) ) ;
#19974 = ADVANCED_FACE ( 'NONE', ( #14592 ), #14279, .F. ) ;
#19975 = CARTESIAN_POINT ( 'NONE',  ( 8.699999999525887873, -28.22468611110281245, -31.13863906511161517 ) ) ;
#19976 = CARTESIAN_POINT ( 'NONE',  ( -22.97691952320000297, 16.89267704250000079, 223.0000000000000000 ) ) ;
#19977 = CARTESIAN_POINT ( 'NONE',  ( -3.925832445961813910, 0.9642144021018008715, -0.6999999999999992895 ) ) ;
#19978 = DIRECTION ( 'NONE',  ( -0.000000000000000000, 1.000000000000000000, -2.257145581549999994E-12 ) ) ;
#19979 = CARTESIAN_POINT ( 'NONE',  ( -10.69999999996385398, -38.97187125431320709, -26.38763492401018596 ) ) ;
#19980 = DIRECTION ( 'NONE',  ( -1.000000000000000000, 1.224606353819999829E-16, 0.000000000000000000 ) ) ;
#19981 = ORIENTED_EDGE ( 'NONE', *, *, #17330, .T. ) ;
#19982 = CARTESIAN_POINT ( 'NONE',  ( 2.618538529469180531, 3.470429992801026042, -14.22796858840000311 ) ) ;
#19983 = CARTESIAN_POINT ( 'NONE',  ( 4.420334067734101424, -4.199682076162645217, -29.45126389020000346 ) ) ;
#19984 = CARTESIAN_POINT ( 'NONE',  ( 3.486379379821376467, -2.190177001292808789, -69.67548878520450728 ) ) ;
#19985 = FACE_OUTER_BOUND ( 'NONE', #1038, .T. ) ;
#19986 = EDGE_CURVE ( 'NONE', #27200, #17105, #9550, .T. ) ;
#19987 = DIRECTION ( 'NONE',  ( 0.000000000000000000, -1.000000000000000000, 0.000000000000000000 ) ) ;
#19988 = CARTESIAN_POINT ( 'NONE',  ( -28.50000000000000000, -5.684341886079999373E-14, 229.0000000000000000 ) ) ;
#19989 = DIRECTION ( 'NONE',  ( -5.551115123047629543E-18, 6.252214723449840749E-31, -1.000000000000000000 ) ) ;
#19990 = AXIS2_PLACEMENT_3D ( 'NONE', #4775, #17029, #7432 ) ;
#19991 = EDGE_CURVE ( 'NONE', #30789, #2523, #27667, .T. ) ;
#19992 = CARTESIAN_POINT ( 'NONE',  ( -20.30403093138962234, 20.00000000003553424, 1.000000000000000888 ) ) ;
#19993 = CARTESIAN_POINT ( 'NONE',  ( -17.04621913067799710, -27.00000000000000355, -34.17350269210000135 ) ) ;
#19994 = CARTESIAN_POINT ( 'NONE',  ( -7.999999999945165641, -111.9817663798748981, 5.760339591700875950 ) ) ;
#19995 = CIRCLE ( 'NONE', #6426, 4.000000004070001225 ) ;
#19996 = VERTEX_POINT ( 'NONE', #4835 ) ;
#19997 = CYLINDRICAL_SURFACE ( 'NONE', #11260, 1.099999999999999201 ) ;
#19998 = DIRECTION ( 'NONE',  ( 1.224606353819999829E-16, 1.000000000000000000, 0.000000000000000000 ) ) ;
#19999 = EDGE_LOOP ( 'NONE', ( #21883, #22376, #5068, #1010 ) ) ;
#20000 = B_SPLINE_CURVE_WITH_KNOTS ( 'NONE', 5,
 ( #19341, #5159, #9583, #21396, #9892, #26721, #28931, #17274, #313, #29231, #30987, #2810, #11939, #26266, #7375, #7221, #12093, #23920, #4705, #16967, #4553, #14468, #19180, #26574 ),
 .UNSPECIFIED., .F., .F.,
 ( 6, 3, 3, 3, 3, 3, 3, 6 ),
 ( 0.000000000000000000, 8.467772783510000068, 16.93507402379999860, 25.40292880670000031, 33.87083985900000016, 42.33863182010000514, 50.80649256519998858, 53.82812356579999857 ),
 .UNSPECIFIED. ) ;
#20001 = CARTESIAN_POINT ( 'NONE',  ( 13.00000000000000000, 22.06507305262541863, -61.91147751336289673 ) ) ;
#20002 = DIRECTION ( 'NONE',  ( -5.962915006522622422E-16, -0.4383711467890810676, -0.8987940462991651502 ) ) ;
#20003 = ORIENTED_EDGE ( 'NONE', *, *, #8806, .T. ) ;
#20004 = CARTESIAN_POINT ( 'NONE',  ( -10.00000000000000000, -130.0000000000000000, -41.24671599790000442 ) ) ;
#20005 = EDGE_LOOP ( 'NONE', ( #29566, #21265, #19866, #25388, #21105, #1713 ) ) ;
#20006 = ORIENTED_EDGE ( 'NONE', *, *, #2792, .F. ) ;
#20007 = AXIS2_PLACEMENT_3D ( 'NONE', #6076, #27789, #8747 ) ;
#20008 = EDGE_LOOP ( 'NONE', ( #16992, #21115, #9903, #6428 ) ) ;
#20009 = CARTESIAN_POINT ( 'NONE',  ( 17.18658402241074867, -10.09981795543446736, -1.000005633855494125E-09 ) ) ;
#20010 = ADVANCED_FACE ( 'NONE', ( #19147 ), #16470, .F. ) ;
#20011 = CARTESIAN_POINT ( 'NONE',  ( 8.700000000248609311, -25.56262797786018837, -31.06236252946161969 ) ) ;
#20012 = CARTESIAN_POINT ( 'NONE',  ( -7.999999999683915952, -16.84112630284391443, -33.19732204833458411 ) ) ;
#20013 = DIRECTION ( 'NONE',  ( 1.000000000000000000, 0.000000000000000000, 0.000000000000000000 ) ) ;
#20014 = EDGE_CURVE ( 'NONE', #29946, #2944, #3165, .T. ) ;
#20015 = DIRECTION ( 'NONE',  ( 0.4999999999969509945, 0.4151946956549595336, 0.7600087925169251024 ) ) ;
#20016 = DIRECTION ( 'NONE',  ( -1.000000000000000000, 0.000000000000000000, 0.000000000000000000 ) ) ;
#20017 = AXIS2_PLACEMENT_3D ( 'NONE', #27218, #4931, #20140 ) ;
#20018 = CARTESIAN_POINT ( 'NONE',  ( 6.112033042629987811, -26.81582465834874540, 208.9768085133924558 ) ) ;
#20019 = CARTESIAN_POINT ( 'NONE',  ( 23.52644129050000288, -14.81042608839999808, 224.6894478949999723 ) ) ;
#20020 = EDGE_CURVE ( 'NONE', #21103, #24608, #11906, .T. ) ;
#20021 = CARTESIAN_POINT ( 'NONE',  ( -3.175770273322759518, 4.553269643686719270, -2.627651354100001946 ) ) ;
#20022 = CARTESIAN_POINT ( 'NONE',  ( -3.117834729128555971, -4.866792379758847709, -18.70544088820000184 ) ) ;
#20023 = LINE ( 'NONE', #13083, #25402 ) ;
#20024 = DIRECTION ( 'NONE',  ( 2.257144471330000330E-12, -0.000000000000000000, -1.000000000000000000 ) ) ;
#20025 = CARTESIAN_POINT ( 'NONE',  ( 8.000000000050000892, -13.30122639390952877, -75.84793558053411289 ) ) ;
#20026 = ADVANCED_FACE ( 'NONE', ( #12212 ), #21824, .F. ) ;
#20027 = DIRECTION ( 'NONE',  ( 0.000000000000000000, 0.3420201433259318358, -0.9396926207858125046 ) ) ;
#20028 = CARTESIAN_POINT ( 'NONE',  ( -23.36339467993373376, -14.50559736726076387, 224.3250316505409501 ) ) ;
#20029 = AXIS2_PLACEMENT_3D ( 'NONE', #21216, #16489, #4538 ) ;
#20030 = CARTESIAN_POINT ( 'NONE',  ( -2.484315071469220815, 2.507604248379868839, -0.6999999999999783062 ) ) ;
#20031 = EDGE_CURVE ( 'NONE', #6095, #8808, #7086, .T. ) ;
#20032 = CARTESIAN_POINT ( 'NONE',  ( 18.13791608029999836, 20.33475167760000346, 229.9172020889999999 ) ) ;
#20033 = PLANE ( 'NONE',  #10769 ) ;
#20034 = ORIENTED_EDGE ( 'NONE', *, *, #21231, .T. ) ;
#20035 = CARTESIAN_POINT ( 'NONE',  ( -4.072259770650454413, 2.021700601781299511, -56.79877225282499609 ) ) ;
#20036 = CARTESIAN_POINT ( 'NONE',  ( -12.36045835447018248, -25.34141119637459738, -23.58428766072654525 ) ) ;
#20037 = PRODUCT_RELATED_PRODUCT_CATEGORY ( 'part', '', ( #1288 ) ) ;
#20038 = CARTESIAN_POINT ( 'NONE',  ( -3.010188847176034521, -5.300177380992629139, -6.685065142700001850 ) ) ;
#20039 = CARTESIAN_POINT ( 'NONE',  ( -27.39085626545857721, 6.366048368229709098, 8.000000000000007105 ) ) ;
#20040 = AXIS2_PLACEMENT_3D ( 'NONE', #16007, #6086, #8284 ) ;
#20041 = CARTESIAN_POINT ( 'NONE',  ( -4.241725247297924994, 0.8684248349431030745, -68.10000000002500542 ) ) ;
#20042 = VERTEX_POINT ( 'NONE', #14898 ) ;
#20043 = VERTEX_POINT ( 'NONE', #24336 ) ;
#20044 = CARTESIAN_POINT ( 'NONE',  ( 0.5703379768913079406, 3.654048244701747272, -92.17990007830465515 ) ) ;
#20045 = B_SPLINE_CURVE_WITH_KNOTS ( 'NONE', 5,
 ( #12739, #5658, #24240, #12122, #7403, #9926 ),
 .UNSPECIFIED., .F., .F.,
 ( 6, 6 ),
 ( 0.000000000000000000, 24.33438218110000051 ),
 .UNSPECIFIED. ) ;
#20046 = FILL_AREA_STYLE ('',( #27128 ) ) ;
#20047 = VERTEX_POINT ( 'NONE', #3077 ) ;
#20048 = CYLINDRICAL_SURFACE ( 'NONE', #9961, 18.00000000000000000 ) ;
#20049 = ADVANCED_FACE ( 'NONE', ( #29355 ), #24671, .F. ) ;
#20050 = CARTESIAN_POINT ( 'NONE',  ( -12.75378086759999796, -32.00000000058999916, -25.51324865459000080 ) ) ;
#20051 = EDGE_LOOP ( 'NONE', ( #5300, #25203, #9803, #18090 ) ) ;
#20052 = CARTESIAN_POINT ( 'NONE',  ( 3.705709820302785396, 4.685590126413917034, -63.63768011632500787 ) ) ;
#20053 = CARTESIAN_POINT ( 'NONE',  ( 1.490216763352725904, -28.46131404266857601, 5.560567654947754512 ) ) ;
#20054 = VECTOR ( 'NONE', #17386, 1000.000000000000000 ) ;
#20055 = EDGE_CURVE ( 'NONE', #27919, #23263, #22600, .T. ) ;
#20056 = CARTESIAN_POINT ( 'NONE',  ( 2.708949881112997282, 3.684664522020660193, -66.64226422532500749 ) ) ;
#20057 = ADVANCED_BREP_SHAPE_REPRESENTATION ( '', ( #688, #17722 ), #28868 ) ;
#20058 = CARTESIAN_POINT ( 'NONE',  ( -16.83342759582943060, -8.999999999996580513, -0.6999999999999784173 ) ) ;
#20059 = SURFACE_STYLE_FILL_AREA ( #17222 ) ;
#20060 = ADVANCED_FACE ( 'NONE', ( #589 ), #2061, .T. ) ;
#20061 = DIRECTION ( 'NONE',  ( -0.5882352941176968164, 0.000000000000000000, -0.8086898285215826654 ) ) ;
#20062 = EDGE_LOOP ( 'NONE', ( #2981, #4100, #19591, #25362 ) ) ;
#20063 = UNCERTAINTY_MEASURE_WITH_UNIT (LENGTH_MEASURE( 1.000000000000000082E-05 ), #5410, 'distance_accuracy_value', 'NONE');
#20064 = AXIS2_PLACEMENT_3D ( 'NONE', #18775, #28382, #19719 ) ;
#20065 = CARTESIAN_POINT ( 'NONE',  ( 24.90302311548996883, -13.86047864964742793, 3.901342110999989288 ) ) ;
#20066 = B_SPLINE_CURVE_WITH_KNOTS ( 'NONE', 3,
 ( #11302, #16477, #9866, #16940 ),
 .UNSPECIFIED., .F., .F.,
 ( 4, 4 ),
 ( 0.000000000000000000, 1.000000000000000000 ),
 .UNSPECIFIED. ) ;
#20067 = LINE ( 'NONE', #3528, #2957 ) ;
#20068 = VECTOR ( 'NONE', #14846, 1000.000000000000000 ) ;
#20069 = ORIENTED_EDGE ( 'NONE', *, *, #18186, .T. ) ;
#20070 = CARTESIAN_POINT ( 'NONE',  ( -16.04158851046123502, 10.23646161653652875, 0.000000000000000000 ) ) ;
#20071 = CARTESIAN_POINT ( 'NONE',  ( -23.83639842780459972, -14.30623133119537727, 6.099998581000020792 ) ) ;
#20072 = FACE_OUTER_BOUND ( 'NONE', #27539, .T. ) ;
#20073 = CARTESIAN_POINT ( 'NONE',  ( -24.34973987568254472, -13.41386311733433878, 4.711897478746439383 ) ) ;
#20074 = LINE ( 'NONE', #27449, #7985 ) ;
#20075 = CYLINDRICAL_SURFACE ( 'NONE', #4651, 1.000000000000000666 ) ;
#20076 = CARTESIAN_POINT ( 'NONE',  ( 13.86097538755027969, -26.60678858114344436, -0.6999999999999784173 ) ) ;
#20077 = CARTESIAN_POINT ( 'NONE',  ( 22.65536946399887341, -14.31703147657543695, 224.7121835352572532 ) ) ;
#20078 = ORIENTED_EDGE ( 'NONE', *, *, #6373, .F. ) ;
#20079 = CARTESIAN_POINT ( 'NONE',  ( 24.37165445055180157, -14.77472140295711434, 4.895781291000017355 ) ) ;
#20080 = CARTESIAN_POINT ( 'NONE',  ( 27.50000000000000000, -3.367667472999999580E-15, 211.8027756369999679 ) ) ;
#20081 = CARTESIAN_POINT ( 'NONE',  ( -26.93395403039999891, 3.298349123919999922E-15, 87.75675929320000535 ) ) ;
#20082 = CARTESIAN_POINT ( 'NONE',  ( -0.1501630636364793547, -28.50011693320649542, 5.900904413000008120 ) ) ;
#20083 = ORIENTED_EDGE ( 'NONE', *, *, #6910, .T. ) ;
#20084 = CARTESIAN_POINT ( 'NONE',  ( 10.93755790620000035, -24.69832375569999883, -1.748184582200003279 ) ) ;
#20085 = AXIS2_PLACEMENT_3D ( 'NONE', #15517, #19937, #25122 ) ;
#20086 = AXIS2_PLACEMENT_3D ( 'NONE', #26597, #26746, #21889 ) ;
#20087 = CARTESIAN_POINT ( 'NONE',  ( 6.379024725906915272, -4.237078256518207908, -68.10000000002500542 ) ) ;
#20088 = CARTESIAN_POINT ( 'NONE',  ( -3.441895295100000141, -11.73074823080000151, 232.6627637660000119 ) ) ;
#20089 = EDGE_CURVE ( 'NONE', #15501, #29138, #11109, .T. ) ;
#20090 = CARTESIAN_POINT ( 'NONE',  ( -4.361670840543652616, -2.217570095850531775, -63.11424626872499744 ) ) ;
#20091 = ORIENTED_EDGE ( 'NONE', *, *, #4892, .F. ) ;
#20092 = CONTEXT_DEPENDENT_SHAPE_REPRESENTATION ( #3542, #21534 ) ;
#20093 = B_SPLINE_CURVE_WITH_KNOTS ( 'NONE', 3,
 ( #697, #10285, #19885, #15767, #20963, #16083 ),
 .UNSPECIFIED., .F., .F.,
 ( 4, 2, 4 ),
 ( 0.000000000000000000, 0.5000000000000000000, 1.000000000000000000 ),
 .UNSPECIFIED. ) ;
#20094 = ORIENTED_EDGE ( 'NONE', *, *, #27097, .F. ) ;
#20095 = EDGE_CURVE ( 'NONE', #23829, #29063, #1285, .T. ) ;
#20096 = CARTESIAN_POINT ( 'NONE',  ( 26.93696268452645626, 0.4901285798022146367, 0.000000000000000000 ) ) ;
#20097 = EDGE_CURVE ( 'NONE', #23233, #16332, #2402, .T. ) ;
#20098 = EDGE_LOOP ( 'NONE', ( #20625, #16290, #2726, #30277 ) ) ;
#20099 = VERTEX_POINT ( 'NONE', #1040 ) ;
#20100 = CARTESIAN_POINT ( 'NONE',  ( 16.47629287105559115, 11.86883708612923982, -0.6999999999999784173 ) ) ;
#20101 = CARTESIAN_POINT ( 'NONE',  ( -12.29999999985416892, -27.78524365307783839, -31.32191803020494802 ) ) ;
#20102 = CARTESIAN_POINT ( 'NONE',  ( -9.500000000000000000, 20.99999999999999645, -64.10000000019999788 ) ) ;
#20103 = CARTESIAN_POINT ( 'NONE',  ( 18.18153821496158074, 11.44785871222162754, -1.400000000000001910 ) ) ;
#20104 = CARTESIAN_POINT ( 'NONE',  ( -12.29999999970000069, -23.80000000074999988, -28.40000000001083791 ) ) ;
#20105 = DIRECTION ( 'NONE',  ( -0.000000000000000000, 1.000000000000000000, -2.257145581549999994E-12 ) ) ;
#20106 = EDGE_LOOP ( 'NONE', ( #20585, #20746, #21993, #30505 ) ) ;
#20107 = CARTESIAN_POINT ( 'NONE',  ( 2.012151113573330985, -3.669704564848118800, -44.10000000002499831 ) ) ;
#20108 = CARTESIAN_POINT ( 'NONE',  ( 24.43659368183839931, 14.66646236428692340, 3.899998581000013509 ) ) ;
#20109 = CARTESIAN_POINT ( 'NONE',  ( -3.679974273075534708, -2.251605409995533602, -22.40799200640001132 ) ) ;
#20110 = CARTESIAN_POINT ( 'NONE',  ( -12.52275726677833134, -26.20837313925740730, -33.71604460516739010 ) ) ;
#20111 = CARTESIAN_POINT ( 'NONE',  ( -23.73992238019999945, -12.43607998449999918, 225.0000000000000000 ) ) ;
#20112 = CARTESIAN_POINT ( 'NONE',  ( 24.08872333959831380, -11.87645233066226069, 86.78285841130833944 ) ) ;
#20113 = CARTESIAN_POINT ( 'NONE',  ( 8.700000000272682499, -17.42905530085155519, -33.49137094649729107 ) ) ;
#20114 = CARTESIAN_POINT ( 'NONE',  ( -2.393684743089937061, 3.904820337558664978, -45.05531229042499319 ) ) ;
#20115 = DIRECTION ( 'NONE',  ( 1.000000000000000000, 0.000000000000000000, 0.000000000000000000 ) ) ;
#20116 = DIRECTION ( 'NONE',  ( -5.551115123049999208E-18, 0.000000000000000000, -1.000000000000000000 ) ) ;
#20117 = CARTESIAN_POINT ( 'NONE',  ( -18.63818496132067182, 19.99999332500478388, 230.6124940282188902 ) ) ;
#20118 = CARTESIAN_POINT ( 'NONE',  ( 304364.2709390003583, 396649.6701459999895, -28.39999793263759997 ) ) ;
#20119 = EDGE_CURVE ( 'NONE', #27091, #5518, #15051, .T. ) ;
#20120 = EDGE_CURVE ( 'NONE', #7730, #27863, #29801, .T. ) ;
#20121 = CARTESIAN_POINT ( 'NONE',  ( -17.49331448452011628, -9.891786026572814805, -0.6999999999999784173 ) ) ;
#20122 = ORIENTED_EDGE ( 'NONE', *, *, #7700, .F. ) ;
#20123 = CARTESIAN_POINT ( 'NONE',  ( 4.904813032679735230, 3.691647504909488564, -32.36032172560000930 ) ) ;
#20124 = ORIENTED_EDGE ( 'NONE', *, *, #1016, .F. ) ;
#20125 = DIRECTION ( 'NONE',  ( -6.181427515845962162E-12, 0.4082287037029531107, 0.9128796883888953273 ) ) ;
#20126 = CARTESIAN_POINT ( 'NONE',  ( -3.108138112192390778, -3.359256988581870385, -50.19612412472499585 ) ) ;
#20127 = ORIENTED_EDGE ( 'NONE', *, *, #26593, .F. ) ;
#20128 = ORIENTED_EDGE ( 'NONE', *, *, #13231, .T. ) ;
#20129 = DIRECTION ( 'NONE',  ( 0.4540090097027652538, -0.7863666718988218118, -0.4189311118017917668 ) ) ;
#20130 = EDGE_LOOP ( 'NONE', ( #9864, #638, #8929, #11346 ) ) ;
#20131 = ORIENTED_EDGE ( 'NONE', *, *, #29489, .T. ) ;
#20132 = FACE_OUTER_BOUND ( 'NONE', #30509, .T. ) ;
#20133 = CARTESIAN_POINT ( 'NONE',  ( -0.5944614571882205212, -27.79380703160649446, 4.999998581000003384 ) ) ;
#20134 = DIRECTION ( 'NONE',  ( 0.000000000000000000, -0.3420201433259318913, 0.9396926207858126157 ) ) ;
#20135 = CARTESIAN_POINT ( 'NONE',  ( 8.000000000287716517, -16.96959321760095563, -37.81493174583665251 ) ) ;
#20136 = CARTESIAN_POINT ( 'NONE',  ( -21.02335142420000125, 19.26967309480000168, 226.0000000000000000 ) ) ;
#20137 = CARTESIAN_POINT ( 'NONE',  ( -3.745245862513339574, 2.150978246590952825, -0.6999999999999991784 ) ) ;
#20138 = CARTESIAN_POINT ( 'NONE',  ( 6.000000000000000000, -17.05999687705277879, -77.21601615383784178 ) ) ;
#20139 = CARTESIAN_POINT ( 'NONE',  ( 0.2650424577970988960, 2.000000000000000000, 230.8412452700000301 ) ) ;
#20140 = DIRECTION ( 'NONE',  ( 0.3633921898465273803, -0.9316362575375355393, 0.000000000000000000 ) ) ;
#20141 = CARTESIAN_POINT ( 'NONE',  ( 1.348918213770415653, 4.124136235849971577, -11.07047964830000453 ) ) ;
#20142 = CARTESIAN_POINT ( 'NONE',  ( 3.853781668572211938, 2.900580182403568408, -31.42282172560000575 ) ) ;
#20143 = DIRECTION ( 'NONE',  ( 0.000000000000000000, 0.000000000000000000, 1.000000000000000000 ) ) ;
#20144 = ADVANCED_FACE ( 'NONE', ( #10332 ), #7948, .T. ) ;
#20145 = DIRECTION ( 'NONE',  ( 1.000000000000000000, -1.843431230200657634E-12, 2.650498504950726461E-12 ) ) ;
#20146 = CARTESIAN_POINT ( 'NONE',  ( 28.49528339128749366, 0.5184828350247822071, 1.000000000000000888 ) ) ;
#20147 = CYLINDRICAL_SURFACE ( 'NONE', #11150, 1.100000000000002309 ) ;
#20148 = CARTESIAN_POINT ( 'NONE',  ( 4.634019325638262465, 0.4639887426745106791, -29.63116556699998938 ) ) ;
#20149 = DIRECTION ( 'NONE',  ( -0.6941258031311203780, -0.7198537139083029945, 0.000000000000000000 ) ) ;
#20150 = DIRECTION ( 'NONE',  ( -1.000000000000000000, 0.000000000000000000, 0.000000000000000000 ) ) ;
#20151 = CARTESIAN_POINT ( 'NONE',  ( 18.95046173579999760, -18.95046173579999760, 115.0000000000000000 ) ) ;
#20152 = ORIENTED_EDGE ( 'NONE', *, *, #18165, .F. ) ;
#20153 = ADVANCED_FACE ( 'NONE', ( #12841 ), #12453, .F. ) ;
#20154 = CARTESIAN_POINT ( 'NONE',  ( 24.36375418468539067, 14.78716628296302282, 6.095965061000018892 ) ) ;
#20155 = DIRECTION ( 'NONE',  ( -1.000000000000000000, 5.665498452320000818E-16, 0.000000000000000000 ) ) ;
#20156 = AXIS2_PLACEMENT_3D ( 'NONE', #16898, #16442, #6840 ) ;
#20157 = ORIENTED_EDGE ( 'NONE', *, *, #2843, .F. ) ;
#20158 = CARTESIAN_POINT ( 'NONE',  ( -8.000000000457589522, -24.26136093481186862, -29.62468611113247263 ) ) ;
#20159 = CARTESIAN_POINT ( 'NONE',  ( 1.776356839399999804E-15, -5.329070518200000398E-15, 227.7662452697800006 ) ) ;
#20160 = ORIENTED_EDGE ( 'NONE', *, *, #28825, .F. ) ;
#20161 = DIRECTION ( 'NONE',  ( 0.000000000000000000, 0.000000000000000000, -1.000000000000000000 ) ) ;
#20162 = EDGE_LOOP ( 'NONE', ( #24254, #6338, #17739, #22006 ) ) ;
#20163 = ORIENTED_EDGE ( 'NONE', *, *, #18082, .F. ) ;
#20164 = B_SPLINE_CURVE_WITH_KNOTS ( 'NONE', 5,
 ( #15552, #14953, #25161, #24550, #12579, #22186 ),
 .UNSPECIFIED., .F., .F.,
 ( 6, 6 ),
 ( 0.000000000000000000, 2.300779731210000012 ),
 .UNSPECIFIED. ) ;
#20165 = ORIENTED_EDGE ( 'NONE', *, *, #26364, .T. ) ;
#20166 = CARTESIAN_POINT ( 'NONE',  ( 16.50835677101655108, -9.893373635889151529, 0.000000000000000000 ) ) ;
#20167 = CARTESIAN_POINT ( 'NONE',  ( -10.69999999999999929, -55.00000000000000000, -42.39999999999999858 ) ) ;
#20168 = CARTESIAN_POINT ( 'NONE',  ( 10.69999999930000101, -24.87867965640000278, -30.52132034359999935 ) ) ;
#20169 = ORIENTED_EDGE ( 'NONE', *, *, #19416, .F. ) ;
#20170 = CARTESIAN_POINT ( 'NONE',  ( -0.1501630636364793547, -28.50011693320649542, 5.900904413000008120 ) ) ;
#20171 = LINE ( 'NONE', #8505, #5498 ) ;
#20172 = EDGE_CURVE ( 'NONE', #22078, #8738, #19148, .T. ) ;
#20173 = CARTESIAN_POINT ( 'NONE',  ( 24.10531740749999940, -15.20475527630000023, 224.7916311099999973 ) ) ;
#20174 = CIRCLE ( 'NONE', #30213, 2.999999999999999112 ) ;
#20175 = CARTESIAN_POINT ( 'NONE',  ( -4.325159770583743679, -1.744232581393518666, -1.497197434500001867 ) ) ;
#20176 = CARTESIAN_POINT ( 'NONE',  ( 1.771049722044198971, -6.234229536879996481, -20.69535708930001050 ) ) ;
#20177 = CARTESIAN_POINT ( 'NONE',  ( 8.999999999770000869, 20.99999999999999645, -64.10000000000000853 ) ) ;
#20178 = PLANE ( 'NONE',  #14031 ) ;
#20179 = CARTESIAN_POINT ( 'NONE',  ( 2.141179080681045122, -2.824862300867048148, -90.52455892065360388 ) ) ;
#20180 = CARTESIAN_POINT ( 'NONE',  ( -22.52001623379999984, 18.04628797879999880, 229.4982322489999831 ) ) ;
#20181 = CARTESIAN_POINT ( 'NONE',  ( 10.69999999996291429, -37.77882377713213913, -25.96954458904216878 ) ) ;
#20182 = CARTESIAN_POINT ( 'NONE',  ( 0.5184513693225318853, -28.49550581263314086, 3.899998581000013509 ) ) ;
#20183 = CARTESIAN_POINT ( 'NONE',  ( 17.67198583300000081, 4.679695666559999800, 230.6999999999999886 ) ) ;
#20184 = CARTESIAN_POINT ( 'NONE',  ( 10.94971450390000101, -24.68950648870000109, -1.737779124299995814 ) ) ;
#20185 = ORIENTED_EDGE ( 'NONE', *, *, #14778, .F. ) ;
#20186 = CARTESIAN_POINT ( 'NONE',  ( -1.256295066205788347, -5.815478746186413694, -55.93033560642499680 ) ) ;
#20187 = CARTESIAN_POINT ( 'NONE',  ( 25.72310959295360533, 9.312057329555777585, 0.000000000000000000 ) ) ;
#20188 = ADVANCED_FACE ( 'NONE', ( #6215 ), #14722, .T. ) ;
#20189 = CARTESIAN_POINT ( 'NONE',  ( -4.663991843195165465, -3.413757688390889555, -18.87254627010000263 ) ) ;
#20190 = CARTESIAN_POINT ( 'NONE',  ( 26.79556473285982321, 0.4875557887249851730, -0.6999999999999784173 ) ) ;
#20191 = CARTESIAN_POINT ( 'NONE',  ( -4.770183054246150967, 0.4556413907088688875, -68.10000000002500542 ) ) ;
#20192 = VERTEX_POINT ( 'NONE', #27937 ) ;
#20193 = VERTEX_POINT ( 'NONE', #15975 ) ;
#20194 = CARTESIAN_POINT ( 'NONE',  ( 2.091444806099476583, 2.888061030883168456, -88.52261276238974119 ) ) ;
#20195 = VECTOR ( 'NONE', #20857, 1000.000000000000114 ) ;
#20196 = FILL_AREA_STYLE ('',( #3353 ) ) ;
#20197 = EDGE_LOOP ( 'NONE', ( #19243, #11879, #13539, #28836 ) ) ;
#20198 = CARTESIAN_POINT ( 'NONE',  ( -24.60726957497166367, 14.37955347300500364, 4.098597478000010064 ) ) ;
#20199 = DIRECTION ( 'NONE',  ( -1.000000000000000000, 0.000000000000000000, -6.771000000000000128E-12 ) ) ;
#20200 = EDGE_CURVE ( 'NONE', #22866, #3218, #21180, .T. ) ;
#20201 = CARTESIAN_POINT ( 'NONE',  ( 1.082264403401735020, -4.420062499635217357, -64.70397119102501904 ) ) ;
#20202 = CARTESIAN_POINT ( 'NONE',  ( -27.53132593009999951, 1.223554590980000005E-11, 229.7313259299999686 ) ) ;
#20203 = EDGE_CURVE ( 'NONE', #12111, #23341, #8405, .T. ) ;
#20204 = CARTESIAN_POINT ( 'NONE',  ( -21.88061800209681707, 17.41725036080275046, -0.5592437529999827461 ) ) ;
#20205 = FACE_OUTER_BOUND ( 'NONE', #24541, .T. ) ;
#20206 = SURFACE_STYLE_USAGE ( .BOTH. , #12969 ) ;
#20207 = CARTESIAN_POINT ( 'NONE',  ( -8.699999999888484936, -60.34578018689309431, -2.533826264316873189 ) ) ;
#20208 = ORIENTED_EDGE ( 'NONE', *, *, #13481, .T. ) ;
#20209 = EDGE_CURVE ( 'NONE', #30177, #3946, #20785, .T. ) ;
#20210 = CARTESIAN_POINT ( 'NONE',  ( 19.80526555962148549, 19.50877392102342256, 1.000000000000000888 ) ) ;
#20211 = FACE_OUTER_BOUND ( 'NONE', #28676, .T. ) ;
#20212 = AXIS2_PLACEMENT_3D ( 'NONE', #29734, #20143, #5969 ) ;
#20213 = EDGE_LOOP ( 'NONE', ( #25477, #3319, #17177, #15089, #3618 ) ) ;
#20214 = CARTESIAN_POINT ( 'NONE',  ( -10.69999999999999929, -27.00000000000000000, -28.40000000000000213 ) ) ;
#20215 = CARTESIAN_POINT ( 'NONE',  ( -24.66346748865669625, -14.28208995890502564, 6.002748559000014694 ) ) ;
#20216 = CARTESIAN_POINT ( 'NONE',  ( -14.09657507470000226, -28.30410041510000241, 229.0000000000000000 ) ) ;
#20217 = CARTESIAN_POINT ( 'NONE',  ( 21.48906533508084138, 17.34561098343697338, 0.08279780700001793114 ) ) ;
#20218 = DIRECTION ( 'NONE',  ( -1.000000000000000000, 1.843431230205392516E-12, -2.650498504954667282E-12 ) ) ;
#20219 = CARTESIAN_POINT ( 'NONE',  ( 3.600464914056809018, -2.449529153870059872, -0.6999999999999992895 ) ) ;
#20220 = EDGE_CURVE ( 'NONE', #24391, #8508, #13623, .T. ) ;
#20221 = CARTESIAN_POINT ( 'NONE',  ( 10.35000000039999968, -130.0000000000000000, -41.24671599790000442 ) ) ;
#20222 = DIRECTION ( 'NONE',  ( 0.000000000000000000, 0.000000000000000000, -1.000000000000000000 ) ) ;
#20223 = VERTEX_POINT ( 'NONE', #21016 ) ;
#20225 = CARTESIAN_POINT ( 'NONE',  ( -24.90462872294776986, -9.900530325344881533, 93.21714158839293418 ) ) ;
#20224 = APPLICATION_CONTEXT ( 'automotive_design' ) ;
#20226 = FACE_OUTER_BOUND ( 'NONE', #21949, .T. ) ;
#20227 = ADVANCED_FACE ( 'NONE', ( #18642 ), #28558, .F. ) ;
#20228 = CARTESIAN_POINT ( 'NONE',  ( 1.850829058368555380, -3.273367579610636291, -37.55154403890418990 ) ) ;
#20229 = DIRECTION ( 'NONE',  ( 0.000000000000000000, 0.000000000000000000, 1.000000000000000000 ) ) ;
#20230 = CARTESIAN_POINT ( 'NONE',  ( -25.87421760616039279, 7.312998917024513545, -0.6999999999999991784 ) ) ;
#20231 = VECTOR ( 'NONE', #21315, 1000.000000000000000 ) ;
#20232 = CARTESIAN_POINT ( 'NONE',  ( -4.300317018729668206, 2.364939115720630980, -59.81908057272499946 ) ) ;
#20233 = ORIENTED_EDGE ( 'NONE', *, *, #7472, .T. ) ;
#20234 = CARTESIAN_POINT ( 'NONE',  ( 19.44955349022768942, 20.00000275008948591, 230.2981396233025464 ) ) ;
#20235 = VERTEX_POINT ( 'NONE', #4804 ) ;
#20236 = CARTESIAN_POINT ( 'NONE',  ( -4.653831783691562585, -30.83989042116281709, 0.5514251240000267451 ) ) ;
#20237 = ORIENTED_EDGE ( 'NONE', *, *, #4777, .F. ) ;
#20238 = DIRECTION ( 'NONE',  ( -6.181333986565961785E-12, 0.4082287037029530552, 0.9128796883888953273 ) ) ;
#20239 = CARTESIAN_POINT ( 'NONE',  ( -12.29999999994666382, -25.48914305888729714, -31.02135916526277271 ) ) ;
#20240 = CARTESIAN_POINT ( 'NONE',  ( -22.90527192528401201, 16.36193184990112570, 6.600000000000022737 ) ) ;
#20241 = CARTESIAN_POINT ( 'NONE',  ( -17.38249745079132680, -25.71151397014635975, -33.42959493591655473 ) ) ;
#20242 = CARTESIAN_POINT ( 'NONE',  ( 24.50348397774029152, -13.13223627703424690, 6.042507865999996675 ) ) ;
#20243 = DIRECTION ( 'NONE',  ( 5.962915006522623408E-16, 0.4383711467890811231, 0.8987940462991652613 ) ) ;
#20244 = ORIENTED_EDGE ( 'NONE', *, *, #20097, .F. ) ;
#20245 = CARTESIAN_POINT ( 'NONE',  ( 1.952025570637784035, -4.468452838841612262, -44.10000000002499831 ) ) ;
#20246 = CARTESIAN_POINT ( 'NONE',  ( 27.54391550559999757, -3.373045393719999713E-15, 137.0437466829999948 ) ) ;
#20247 = CARTESIAN_POINT ( 'NONE',  ( 4.266075142677475007, -0.9221078188639888484, -23.79036215650000230 ) ) ;
#20248 = CARTESIAN_POINT ( 'NONE',  ( 23.52681767382016531, -12.83507605025694964, 4.090187774658970987 ) ) ;
#20249 = CARTESIAN_POINT ( 'NONE',  ( 304364.2709390003583, -396703.6701459999895, -28.39999793294318664 ) ) ;
#20250 = EDGE_CURVE ( 'NONE', #13182, #28945, #18150, .T. ) ;
#20251 = VECTOR ( 'NONE', #27647, 1000.000000000000000 ) ;
#20252 = B_SPLINE_CURVE_WITH_KNOTS ( 'NONE', 3,
 ( #30655, #11297, #9081, #28438, #8765, #1853 ),
 .UNSPECIFIED., .F., .F.,
 ( 4, 2, 4 ),
 ( 0.000000000000000000, 0.5000000000000000000, 1.000000000000000000 ),
 .UNSPECIFIED. ) ;
#20253 = CARTESIAN_POINT ( 'NONE',  ( -27.50000000000000000, 3.367667473009999970E-15, 186.3944487260000074 ) ) ;
#20254 = CARTESIAN_POINT ( 'NONE',  ( -1.419173372180000084E-06, -27.80022181310000207, 223.9000014189999774 ) ) ;
#20255 = CARTESIAN_POINT ( 'NONE',  ( -3.250950776947245213, -3.159825117472807143, -47.20083066912499703 ) ) ;
#20256 = EDGE_CURVE ( 'NONE', #27013, #26158, #29414, .T. ) ;
#20257 = DIRECTION ( 'NONE',  ( -0.9880370573969196046, 0.1542166437529879086, 1.480297366166875051E-13 ) ) ;
#20258 = EDGE_CURVE ( 'NONE', #22923, #28198, #16653, .T. ) ;
#20259 = FACE_BOUND ( 'NONE', #11654, .T. ) ;
#20260 = CARTESIAN_POINT ( 'NONE',  ( -18.63933997799378517, 19.99999301019102660, 230.6122333795804025 ) ) ;
#20261 = CARTESIAN_POINT ( 'NONE',  ( -27.24857305730000334, -4.411440552420000435E-12, 229.9172022069999741 ) ) ;
#20262 = B_SPLINE_CURVE_WITH_KNOTS ( 'NONE', 3,
 ( #1806, #11395, #27596, #17984, #4000, #16262, #25880, #3678, #20840, #6511, #30276, #28067, #6037, #13751 ),
 .UNSPECIFIED., .F., .F.,
 ( 4, 2, 2, 2, 2, 2, 4 ),
 ( 0.000000000000000000, 0.2500000000000006106, 0.3750000000000021094, 0.4375000000000021649, 0.5000000000000023315, 0.7500000000000011102, 1.000000000000000000 ),
 .UNSPECIFIED. ) ;
#20263 = CARTESIAN_POINT ( 'NONE',  ( 8.964607010186844249, -25.25702356185616182, 24.41994893493238905 ) ) ;
#20264 = EDGE_LOOP ( 'NONE', ( #16521, #17741, #23891, #19513 ) ) ;
#20265 = CARTESIAN_POINT ( 'NONE',  ( -4.901082056047598279, -4.330235462250267453, -33.83447003409999354 ) ) ;
#20266 = ORIENTED_EDGE ( 'NONE', *, *, #29145, .F. ) ;
#20267 = CARTESIAN_POINT ( 'NONE',  ( -8.000000000035504044, -116.0414483704504676, 19.89613934350951041 ) ) ;
#20268 = CARTESIAN_POINT ( 'NONE',  ( 4.421972129926212247, 1.961202595004083005, -51.87998794302499306 ) ) ;
#20269 = VECTOR ( 'NONE', #12877, 1000.000000000000000 ) ;
#20270 = ORIENTED_EDGE ( 'NONE', *, *, #1514, .T. ) ;
#20271 = ORIENTED_EDGE ( 'NONE', *, *, #3517, .F. ) ;
#20272 = PRODUCT_CONTEXT ( 'NONE', #17015, 'mechanical' ) ;
#20273 = CIRCLE ( 'NONE', #19792, 1.099999999570000497 ) ;
#20274 = ORIENTED_EDGE ( 'NONE', *, *, #14092, .T. ) ;
#20275 = ORIENTED_EDGE ( 'NONE', *, *, #25652, .F. ) ;
#20276 = CARTESIAN_POINT ( 'NONE',  ( -17.93062603642077946, 10.83602254735704484, -0.6999999999999784173 ) ) ;
#20277 = CARTESIAN_POINT ( 'NONE',  ( 17.85846454801659533, 10.13281012205188425, -4.336808689942017736E-16 ) ) ;
#20278 = DIRECTION ( 'NONE',  ( 1.000000000000000000, -1.843431230200084908E-12, 2.650498504963248473E-12 ) ) ;
#20279 = CARTESIAN_POINT ( 'NONE',  ( -13.75032424529999986, -27.60893268180000248, 222.0000000000000000 ) ) ;
#20280 = CARTESIAN_POINT ( 'NONE',  ( -0.9245300002449383658, -27.48475604047732190, 4.402548359813233780 ) ) ;
#20281 = CARTESIAN_POINT ( 'NONE',  ( -3.789431608055533474, 1.866661010915773744, -0.6999999999999994005 ) ) ;
#20282 = CARTESIAN_POINT ( 'NONE',  ( -5.114250173070000294, -17.43050732980000106, 230.0000000000000000 ) ) ;
#20283 = CARTESIAN_POINT ( 'NONE',  ( 1.009922359840511374, -1.745934706676925297, 230.8412452700000301 ) ) ;
#20284 = CARTESIAN_POINT ( 'NONE',  ( -18.04593937785069357, 20.00000752677722815, -0.6992883787361406922 ) ) ;
#20285 = CARTESIAN_POINT ( 'NONE',  ( -1.184025259985578948, -4.532227402022654061, -13.05022317840000312 ) ) ;
#20286 = CARTESIAN_POINT ( 'NONE',  ( 2.561732861596754507, -4.873875974289409108, -32.20721934060000535 ) ) ;
#20287 = AXIS2_PLACEMENT_3D ( 'NONE', #28554, #4333, #2124 ) ;
#20288 = CARTESIAN_POINT ( 'NONE',  ( 1.776356839399999922E-14, 0.000000000000000000, 232.0000000000000000 ) ) ;
#20289 = DIRECTION ( 'NONE',  ( 1.000000000000000000, 0.000000000000000000, 0.000000000000000000 ) ) ;
#20290 = AXIS2_PLACEMENT_3D ( 'NONE', #25183, #25032, #10560 ) ;
#20291 = CARTESIAN_POINT ( 'NONE',  ( -8.000000000050963678, -115.4736671374892722, 21.16580987455534668 ) ) ;
#20292 = CARTESIAN_POINT ( 'NONE',  ( 1.456545767631101107, -4.104408573385627257, -30.25632401680000783 ) ) ;
#20293 = CIRCLE ( 'NONE', #24325, 27.92857142820000149 ) ;
#20294 = CIRCLE ( 'NONE', #20831, 26.80000000000000071 ) ;
#20295 = VECTOR ( 'NONE', #21576, 1000.000000000000000 ) ;
#20296 = CARTESIAN_POINT ( 'NONE',  ( 19.80538173989999962, 19.50875420239999869, 228.1999999569999886 ) ) ;
#20297 = PLANE ( 'NONE',  #17740 ) ;
#20298 = CARTESIAN_POINT ( 'NONE',  ( -27.50000000000000000, 3.367667473009999970E-15, 93.28090191849999258 ) ) ;
#20299 = EDGE_CURVE ( 'NONE', #9121, #24850, #18953, .T. ) ;
#20300 = ORIENTED_EDGE ( 'NONE', *, *, #6056, .F. ) ;
#20301 = EDGE_LOOP ( 'NONE', ( #27398, #11702, #24582, #4514 ) ) ;
#20302 = CARTESIAN_POINT ( 'NONE',  ( 23.69427943123108093, 14.54081805611945910, 6.079851352999988023 ) ) ;
#20303 = CARTESIAN_POINT ( 'NONE',  ( 10.02699808790000091, 19.99999999999999645, -2.016765154599996279 ) ) ;
#20304 = ORIENTED_EDGE ( 'NONE', *, *, #30170, .T. ) ;
#20305 = DIRECTION ( 'NONE',  ( 0.000000000000000000, 0.000000000000000000, 1.000000000000000000 ) ) ;
#20306 = CARTESIAN_POINT ( 'NONE',  ( 8.000000000289732682, -15.05691661385925961, -37.86814300156539304 ) ) ;
#20307 = MECHANICAL_DESIGN_GEOMETRIC_PRESENTATION_REPRESENTATION (  '', ( #10281 ), #3732 ) ;
#20308 = ORIENTED_EDGE ( 'NONE', *, *, #224, .F. ) ;
#20309 = CARTESIAN_POINT ( 'NONE',  ( -2.813083154009999692E-14, -26.79999999949999889, 3.899999999999999911 ) ) ;
#20310 = ORIENTED_EDGE ( 'NONE', *, *, #30649, .T. ) ;
#20311 = ORIENTED_EDGE ( 'NONE', *, *, #30210, .T. ) ;
#20312 = EDGE_LOOP ( 'NONE', ( #20525, #3236, #28639, #10739, #26821, #27017, #26545, #30698, #22990, #24228 ) ) ;
#20313 = CARTESIAN_POINT ( 'NONE',  ( 27.48412515190000249, 9.625371191550000205, 229.2404163060000144 ) ) ;
#20314 = AXIS2_PLACEMENT_3D ( 'NONE', #16511, #4092, #11334 ) ;
#20315 = B_SPLINE_CURVE_WITH_KNOTS ( 'NONE', 1,
 ( #28557, #28853 ),
 .UNSPECIFIED., .F., .F.,
 ( 2, 2 ),
 ( -3.500000000000000000, 3.500000000000000000 ),
 .UNSPECIFIED. ) ;
#20316 = CARTESIAN_POINT ( 'NONE',  ( -17.04621913067799710, -32.00000000000000000, -31.28675134614999820 ) ) ;
#20318 = FACE_OUTER_BOUND ( 'NONE', #2819, .T. ) ;
#20317 = MECHANICAL_DESIGN_GEOMETRIC_PRESENTATION_REPRESENTATION (  '', ( #8240 ), #1733 ) ;
#20319 = AXIS2_PLACEMENT_3D ( 'NONE', #11068, #23032, #4303 ) ;
#20320 = CARTESIAN_POINT ( 'NONE',  ( -14.09657507470000226, -28.30410041510000241, 222.0000000000000000 ) ) ;
#20321 = CARTESIAN_POINT ( 'NONE',  ( 11.69999999989999928, 19.99999999999999645, -0.6999999999999992895 ) ) ;
#20322 = CIRCLE ( 'NONE', #19842, 27.23548387100000312 ) ;
#20323 = CARTESIAN_POINT ( 'NONE',  ( -24.25537239878455509, -13.58380780107177976, 5.677299029929432805 ) ) ;
#20324 = CARTESIAN_POINT ( 'NONE',  ( 9.993285220779432265, -25.61999708228224648, 202.5328830256821391 ) ) ;
#20325 = CARTESIAN_POINT ( 'NONE',  ( -0.1058797546490000130, -28.50006311429999784, 226.0959516479999820 ) ) ;
#20326 = ADVANCED_FACE ( 'NONE', ( #2291 ), #30764, .T. ) ;
#20327 = CARTESIAN_POINT ( 'NONE',  ( -5.440024667461782037, 2.837840394948672351, -1.418764356299999418 ) ) ;
#20328 = CARTESIAN_POINT ( 'NONE',  ( 6.096654317658788180, 0.1519075334363156893, -20.67661200060000226 ) ) ;
#20329 = DIRECTION ( 'NONE',  ( -1.000000000000000000, 0.000000000000000000, 0.000000000000000000 ) ) ;
#20330 = B_SPLINE_CURVE_WITH_KNOTS ( 'NONE', 3,
 ( #13684, #14001, #25656, #6441, #30202, #21085 ),
 .UNSPECIFIED., .F., .F.,
 ( 4, 2, 4 ),
 ( 0.000000000000000000, 0.5000000000000000000, 1.000000000000000000 ),
 .UNSPECIFIED. ) ;
#20331 = DIRECTION ( 'NONE',  ( -1.000000000000000000, 0.000000000000000000, 0.000000000000000000 ) ) ;
#20332 = CARTESIAN_POINT ( 'NONE',  ( 1.111846212943386591, -3.388043077324369268, -88.52261276293990022 ) ) ;
#20333 = CARTESIAN_POINT ( 'NONE',  ( -3.072394438959999974, -1.678456730820000020, 230.8356432492296619 ) ) ;
#20334 = CARTESIAN_POINT ( 'NONE',  ( -2.947640775130000104E-14, -27.50000000000000000, 115.0000000000000000 ) ) ;
#20335 = DIRECTION ( 'NONE',  ( -5.962915006522622422E-16, -0.4383711467890810676, -0.8987940462991651502 ) ) ;
#20336 = CARTESIAN_POINT ( 'NONE',  ( 7.957576824819999395, -16.45835136280000199, 230.6999999999999886 ) ) ;
#20337 = DIRECTION ( 'NONE',  ( 1.000000000000000000, -1.224606353819999829E-16, 0.000000000000000000 ) ) ;
#20338 = VECTOR ( 'NONE', #22212, 1000.000000000000000 ) ;
#20339 = ORIENTED_EDGE ( 'NONE', *, *, #8040, .T. ) ;
#20340 = CARTESIAN_POINT ( 'NONE',  ( -4.180007949804073419, -3.103635835586971758, -55.47895058492500198 ) ) ;
#20341 = CARTESIAN_POINT ( 'NONE',  ( -23.81776757772072983, -15.65134804123479917, 4.999998581000003384 ) ) ;
#20342 = ORIENTED_EDGE ( 'NONE', *, *, #5098, .T. ) ;
#20343 = AXIS2_PLACEMENT_3D ( 'NONE', #24295, #29314, #703 ) ;
#20344 = CARTESIAN_POINT ( 'NONE',  ( 1.086829820489895848, 5.988658659452708477, -14.02400681850000197 ) ) ;
#20345 = ORIENTED_EDGE ( 'NONE', *, *, #3930, .F. ) ;
#20346 = CARTESIAN_POINT ( 'NONE',  ( -25.08454981450000076, -13.52946590100000179, 225.7602695480000250 ) ) ;
#20347 = CARTESIAN_POINT ( 'NONE',  ( -4.229156943520672840, 0.7760457000830683905, -68.10000000002500542 ) ) ;
#20348 = EDGE_CURVE ( 'NONE', #9043, #7844, #11571, .T. ) ;
#20349 = ORIENTED_EDGE ( 'NONE', *, *, #19186, .F. ) ;
#20350 = ORIENTED_EDGE ( 'NONE', *, *, #18472, .T. ) ;
#20351 = EDGE_LOOP ( 'NONE', ( #11872, #23822, #8900, #1843 ) ) ;
#20352 = CARTESIAN_POINT ( 'NONE',  ( -6.999999999265341444, -5.287238791109590608, -26.38853270487952685 ) ) ;
#20353 = AXIS2_PLACEMENT_3D ( 'NONE', #6150, #22539, #15749 ) ;
#20354 = ORIENTED_EDGE ( 'NONE', *, *, #27154, .F. ) ;
#20355 = FACE_OUTER_BOUND ( 'NONE', #22382, .T. ) ;
#20356 = CIRCLE ( 'NONE', #24879, 2.000000000000000000 ) ;
#20357 = AXIS2_PLACEMENT_3D ( 'NONE', #5644, #10532, #19825 ) ;
#20358 = CARTESIAN_POINT ( 'NONE',  ( 23.35655559247464907, 15.07705663187610945, 5.680691777000007825 ) ) ;
#20359 = CARTESIAN_POINT ( 'NONE',  ( 1.082264403396195673, -4.420062499643547582, -64.30397119102499914 ) ) ;
#20360 = ADVANCED_FACE ( 'NONE', ( #9193 ), #19268, .T. ) ;
#20361 = CARTESIAN_POINT ( 'NONE',  ( -27.24857305730000334, 4.416023102750000085E-12, 229.9172022069999741 ) ) ;
#20362 = FACE_OUTER_BOUND ( 'NONE', #12018, .T. ) ;
#20363 = CARTESIAN_POINT ( 'NONE',  ( 10.69999999999999929, 19.99999999999999645, -42.39999999999999858 ) ) ;
#20364 = DIRECTION ( 'NONE',  ( -0.9595496299849965993, 0.2815395311419987001, 0.000000000000000000 ) ) ;
#20365 = EDGE_CURVE ( 'NONE', #29420, #14789, #12029, .T. ) ;
#20366 = CARTESIAN_POINT ( 'NONE',  ( -25.87726812276423516, 7.302694712675908306, -1.399999999999998579 ) ) ;
#20367 = VERTEX_POINT ( 'NONE', #87 ) ;
#20368 = CARTESIAN_POINT ( 'NONE',  ( -4.345037505360560992, 2.733239894040710105, -9.507975902800009038 ) ) ;
#20369 = CARTESIAN_POINT ( 'NONE',  ( 0.1474953932389658495, -26.80000000000002203, 6.100000000000008527 ) ) ;
#20370 = PRODUCT_DEFINITION_SHAPE ( 'NONE', 'NONE',  #21398 ) ;
#20371 = DIRECTION ( 'NONE',  ( 0.000000000000000000, 0.000000000000000000, -1.000000000000000000 ) ) ;
#20372 = ORIENTED_EDGE ( 'NONE', *, *, #939, .F. ) ;
#20373 = CARTESIAN_POINT ( 'NONE',  ( 24.87112161019999945, -13.91739822849999975, 223.9575271749999672 ) ) ;
#20374 = FACE_OUTER_BOUND ( 'NONE', #30445, .T. ) ;
#20375 = CYLINDRICAL_SURFACE ( 'NONE', #3745, 26.80000000000002203 ) ;
#20376 = CARTESIAN_POINT ( 'NONE',  ( 27.44414120988032124, 5.042033447402311630, 0.2686740700000300741 ) ) ;
#20377 = CARTESIAN_POINT ( 'NONE',  ( -27.50000000000000000, 3.367667473009999970E-15, 230.0000000000000000 ) ) ;
#20378 = CARTESIAN_POINT ( 'NONE',  ( -2.744417411265728912, -4.298957096598221561, -44.10000000002499121 ) ) ;
#20379 = CARTESIAN_POINT ( 'NONE',  ( -11.16922181809999870, -24.52928868880000124, -1.544021063100003976 ) ) ;
#20380 = CARTESIAN_POINT ( 'NONE',  ( 5.245096043587340162, -0.2338077457563897399, -35.69999999999999574 ) ) ;
#20381 = PRODUCT_DEFINITION_FORMATION_WITH_SPECIFIED_SOURCE ( 'ANY', '', #4122, .NOT_KNOWN. ) ;
#20382 = VERTEX_POINT ( 'NONE', #9666 ) ;
#20383 = ADVANCED_FACE ( 'NONE', ( #7313 ), #28403, .F. ) ;
#20384 = CARTESIAN_POINT ( 'NONE',  ( 24.20792487550426841, -13.66932880343719781, 3.920132063000014710 ) ) ;
#20385 = CARTESIAN_POINT ( 'NONE',  ( 25.26809617039999978, 12.77001320649999982, 223.3999999999999773 ) ) ;
#20386 = EDGE_CURVE ( 'NONE', #22567, #15475, #30697, .T. ) ;
#20387 = CARTESIAN_POINT ( 'NONE',  ( 0.8240483502834883289, -3.944499275425427776, -68.10000000002501963 ) ) ;
#20388 = DIRECTION ( 'NONE',  ( 0.000000000000000000, -2.257145581549999994E-12, -1.000000000000000000 ) ) ;
#20389 = CARTESIAN_POINT ( 'NONE',  ( -3.607711123481817328, -1.653375552380872637, -44.10000000002498410 ) ) ;
#20390 = EDGE_CURVE ( 'NONE', #22757, #31042, #26423, .T. ) ;
#20391 = B_SPLINE_CURVE_WITH_KNOTS ( 'NONE', 3,
 ( #29584, #8019, #10552, #27223 ),
 .UNSPECIFIED., .F., .F.,
 ( 4, 4 ),
 ( 0.000000000000000000, 1.000000000000000000 ),
 .UNSPECIFIED. ) ;
#20392 = CARTESIAN_POINT ( 'NONE',  ( 14.81460958102759484, -23.82568693630179624, -32.34047020245367321 ) ) ;
#20393 = CARTESIAN_POINT ( 'NONE',  ( -4.977446647723676953, -11.28020519024507706, 232.6627637660202197 ) ) ;
#20394 = CARTESIAN_POINT ( 'NONE',  ( -1.143212971672624478, -4.711439499498765393, -62.34311227092499053 ) ) ;
#20395 = VERTEX_POINT ( 'NONE', #10889 ) ;
#20396 = CARTESIAN_POINT ( 'NONE',  ( 18.83543878183406051, 20.00014484542172966, 230.5612148851877521 ) ) ;
#20397 = ORIENTED_EDGE ( 'NONE', *, *, #5831, .T. ) ;
#20399 = EDGE_CURVE ( 'NONE', #26338, #27598, #896, .T. ) ;
#20398 = CARTESIAN_POINT ( 'NONE',  ( 8.700000000281498558, -22.22877482711028563, -40.15596262314623033 ) ) ;
#20400 = EDGE_LOOP ( 'NONE', ( #19669, #24395, #2862, #15059, #13535, #196, #19708, #26043, #23094, #3092, #19981, #20562 ) ) ;
#20401 = CARTESIAN_POINT ( 'NONE',  ( -2.267065256228490533, 2.465013841745427037, -42.01924257443324962 ) ) ;
#20402 = CARTESIAN_POINT ( 'NONE',  ( -28.49999999959999641, -10.47094308429999998, 229.0000000000000000 ) ) ;
#20403 = CARTESIAN_POINT ( 'NONE',  ( -0.7153897335033406746, 3.455736562763356279, 0.000000000000000000 ) ) ;
#20404 = CARTESIAN_POINT ( 'NONE',  ( -17.41915764887747997, -23.51136720943065228, -32.15933961136000363 ) ) ;
#20405 = DIRECTION ( 'NONE',  ( 0.000000000000000000, 0.000000000000000000, 1.000000000000000000 ) ) ;
#20406 = DIRECTION ( 'NONE',  ( 0.000000000000000000, 0.000000000000000000, -1.000000000000000000 ) ) ;
#20407 = ORIENTED_EDGE ( 'NONE', *, *, #24315, .F. ) ;
#20408 = DIRECTION ( 'NONE',  ( 0.000000000000000000, 0.000000000000000000, -1.000000000000000000 ) ) ;
#20409 = CARTESIAN_POINT ( 'NONE',  ( 28.04325408110000240, -4.147902640509999414E-14, 230.2432540810000319 ) ) ;
#20410 = ADVANCED_FACE ( 'NONE', ( #11047 ), #25685, .T. ) ;
#20411 = CARTESIAN_POINT ( 'NONE',  ( -17.93053308114354394, -8.908107087747509922, 0.000000000000000000 ) ) ;
#20412 = CARTESIAN_POINT ( 'NONE',  ( -24.66442003930000126, -14.28072947929999970, 226.1000014189999945 ) ) ;
#20413 = CARTESIAN_POINT ( 'NONE',  ( 20.30396079662882158, 20.00000000004802203, 3.000000000000002665 ) ) ;
#20414 = CARTESIAN_POINT ( 'NONE',  ( -17.59974562539740717, 10.19782190216913875, -1.400000000000001910 ) ) ;
#20415 = CARTESIAN_POINT ( 'NONE',  ( -0.8137756071791968360, 4.795696781221863603, -50.50792092402500799 ) ) ;
#20416 = DIRECTION ( 'NONE',  ( -5.962915006522622422E-16, -0.4383711467890810676, -0.8987940462991651502 ) ) ;
#20417 = EDGE_CURVE ( 'NONE', #11023, #16979, #24912, .T. ) ;
#20418 = CARTESIAN_POINT ( 'NONE',  ( 4.433903769297828035, -26.43189459824146326, 209.5952735306987336 ) ) ;
#20419 = CARTESIAN_POINT ( 'NONE',  ( -18.63196155432577328, 19.99999456996440017, 230.6139042306207898 ) ) ;
#20420 = CARTESIAN_POINT ( 'NONE',  ( -24.76171951330573862, -10.25169584067250383, 43.21714158839993303 ) ) ;
#20421 = CARTESIAN_POINT ( 'NONE',  ( 24.13062658790415682, -13.18986347251061808, 225.9130852754918806 ) ) ;
#20422 = ORIENTED_EDGE ( 'NONE', *, *, #15526, .T. ) ;
#20423 = CARTESIAN_POINT ( 'NONE',  ( -4.434312336397093546, -3.917832084918029256, -34.83447003410000065 ) ) ;
#20424 = ORIENTED_EDGE ( 'NONE', *, *, #1113, .F. ) ;
#20425 = DIRECTION ( 'NONE',  ( -0.8775825618903722036, -0.4794255386042041156, 0.000000000000000000 ) ) ;
#20426 = CARTESIAN_POINT ( 'NONE',  ( 4.101176313917073379, -1.931410228222276038, -52.69872167392500018 ) ) ;
#20427 = ORIENTED_EDGE ( 'NONE', *, *, #12699, .F. ) ;
#20428 = ITEM_DEFINED_TRANSFORMATION ( 'NONE', 'NONE', #22391,  #17722 ) ;
#20429 = ORIENTED_EDGE ( 'NONE', *, *, #12551, .T. ) ;
#20430 = EDGE_CURVE ( 'NONE', #20047, #17900, #23424, .T. ) ;
#20431 = VERTEX_POINT ( 'NONE', #16073 ) ;
#20432 = CARTESIAN_POINT ( 'NONE',  ( -17.82156395551385941, -9.499568885231910897, 0.000000000000000000 ) ) ;
#20433 = DIRECTION ( 'NONE',  ( 0.000000000000000000, 0.000000000000000000, 1.000000000000000000 ) ) ;
#20434 = CARTESIAN_POINT ( 'NONE',  ( 9.500000000000000000, 20.99999999999999645, -60.10000000019999788 ) ) ;
#20435 = EDGE_CURVE ( 'NONE', #24964, #27054, #518, .T. ) ;
#20436 = LINE ( 'NONE', #11004, #29013 ) ;
#20437 = CARTESIAN_POINT ( 'NONE',  ( -1.100000000000000311, -27.47799119229999931, 4.902983112562558254 ) ) ;
#20438 = CARTESIAN_POINT ( 'NONE',  ( -5.068867860199277153, -0.8055594120499698363, -0.6999999999999992895 ) ) ;
#20439 = CARTESIAN_POINT ( 'NONE',  ( 4.080592064681261455, -5.083854565965863159, -2.505321867100007704 ) ) ;
#20440 = ADVANCED_BREP_SHAPE_REPRESENTATION ( '', ( #121, #17722 ), #27910 ) ;
#20441 = CARTESIAN_POINT ( 'NONE',  ( -9.999999999979998222, -127.2536115484999897, -34.36329565063000047 ) ) ;
#20442 = DIRECTION ( 'NONE',  ( 1.000000000000000000, 6.668066630619518976E-24, -2.257150022442225012E-12 ) ) ;
#20443 = CARTESIAN_POINT ( 'NONE',  ( -4.799781135534763266, 0.1424267153701331001, -14.12054957890000040 ) ) ;
#20444 = CARTESIAN_POINT ( 'NONE',  ( 0.1051796283266584475, -6.084780997910130829, -33.41110030499999795 ) ) ;
#20445 = B_SPLINE_CURVE_WITH_KNOTS ( 'NONE', 5,
 ( #30988, #26117, #26427, #12246, #7530, #26267, #21549, #2811, #12403 ),
 .UNSPECIFIED., .F., .F.,
 ( 6, 3, 6 ),
 ( 0.000000000000000000, 0.7281981450769999809, 1.224410041430000096 ),
 .UNSPECIFIED. ) ;
#20446 = B_SPLINE_CURVE_WITH_KNOTS ( 'NONE', 3,
 ( #8293, #22948, #5940, #3579, #22784, #1237 ),
 .UNSPECIFIED., .F., .F.,
 ( 4, 2, 4 ),
 ( 0.000000000000000000, 0.5000000000000000000, 1.000000000000000000 ),
 .UNSPECIFIED. ) ;
#20447 = CARTESIAN_POINT ( 'NONE',  ( 16.40303402075260308, 10.20816091466531716, 0.000000000000000000 ) ) ;
#20448 = CARTESIAN_POINT ( 'NONE',  ( 8.700000000277906764, -15.94902145836247342, -35.53273252485295330 ) ) ;
#20449 = CARTESIAN_POINT ( 'NONE',  ( -2.656656946654432971, -2.398535190107887960, 227.6918569120630593 ) ) ;
#20450 = CARTESIAN_POINT ( 'NONE',  ( 0.03533597109940000286, -28.50021994999999819, 226.1000014189999945 ) ) ;
#20451 = CARTESIAN_POINT ( 'NONE',  ( -3.721299799755369619, 0.5540072166027351086, 227.7972036410060639 ) ) ;
#20452 = CARTESIAN_POINT ( 'NONE',  ( 20.30405755279999980, 20.00000000000000000, 228.5999999789999890 ) ) ;
#20453 = CARTESIAN_POINT ( 'NONE',  ( 8.000000000481156448, -28.77621036719994763, -25.95065533245048428 ) ) ;
#20454 = CARTESIAN_POINT ( 'NONE',  ( 0.07063658732710000054, -28.50016343120000073, 223.9013487590000011 ) ) ;
#20455 = ORIENTED_EDGE ( 'NONE', *, *, #3819, .T. ) ;
#20456 = ORIENTED_EDGE ( 'NONE', *, *, #5597, .F. ) ;
#20457 = CARTESIAN_POINT ( 'NONE',  ( -7.999999999726984612, -25.09035620932252186, -26.05319937760163285 ) ) ;
#20458 = CARTESIAN_POINT ( 'NONE',  ( 10.63581336919999920, 19.99999999999999645, -1.053405123100002783 ) ) ;
#20459 = ORIENTED_EDGE ( 'NONE', *, *, #18186, .F. ) ;
#20460 = AXIS2_PLACEMENT_3D ( 'NONE', #2496, #11930, #12084 ) ;
#20461 = LINE ( 'NONE', #30215, #1260 ) ;
#20462 = FACE_OUTER_BOUND ( 'NONE', #5576, .T. ) ;
#20463 = VERTEX_POINT ( 'NONE', #1605 ) ;
#20464 = CARTESIAN_POINT ( 'NONE',  ( -18.29999999989999893, -24.07317073171000033, -28.39999999989999679 ) ) ;
#20465 = ORIENTED_EDGE ( 'NONE', *, *, #3341, .T. ) ;
#20466 = VERTEX_POINT ( 'NONE', #18739 ) ;
#20467 =( NAMED_UNIT ( * ) PLANE_ANGLE_UNIT ( ) SI_UNIT ( $, .RADIAN. ) );
#20468 = VERTEX_POINT ( 'NONE', #2385 ) ;
#20469 = DIRECTION ( 'NONE',  ( -0.7071067811870476172, 0.000000000000000000, -0.7071067811860475283 ) ) ;
#20470 = EDGE_CURVE ( 'NONE', #21131, #27919, #1568, .T. ) ;
#20471 = CARTESIAN_POINT ( 'NONE',  ( -27.92857142909999979, 3.420150602519999655E-15, 142.0603150149999863 ) ) ;
#20472 = DIRECTION ( 'NONE',  ( 0.000000000000000000, 1.000000000000000000, 0.000000000000000000 ) ) ;
#20473 = FILL_AREA_STYLE_COLOUR ( '', #24491 ) ;
#20474 = EDGE_CURVE ( 'NONE', #25571, #28640, #21426, .T. ) ;
#20475 = CARTESIAN_POINT ( 'NONE',  ( -6.104465766177795238, 6.241691732493892530, -40.52344563684190604 ) ) ;
#20476 = CIRCLE ( 'NONE', #6907, 26.79999999129999821 ) ;
#20477 = EDGE_CURVE ( 'NONE', #13631, #3948, #26742, .T. ) ;
#20478 = CARTESIAN_POINT ( 'NONE',  ( 8.095177325567849635, -26.28419651245282651, 207.3284286765387208 ) ) ;
#20479 = CARTESIAN_POINT ( 'NONE',  ( 23.73992238019999945, -12.43607998449999918, 5.000000000000000000 ) ) ;
#20480 = CARTESIAN_POINT ( 'NONE',  ( -7.999999999669955564, -13.42967257572369277, -35.49331476339211378 ) ) ;
#20481 = ORIENTED_EDGE ( 'NONE', *, *, #16011, .F. ) ;
#20482 = VECTOR ( 'NONE', #1682, 1000.000000000000000 ) ;
#20483 = CARTESIAN_POINT ( 'NONE',  ( -4.921927080085812811, 2.567569881136803733, -2.418764356300004970 ) ) ;
#20484 = CARTESIAN_POINT ( 'NONE',  ( -4.430040892179064826, 1.363067613765865937, -21.82289663400000279 ) ) ;
#20485 = CARTESIAN_POINT ( 'NONE',  ( -8.414407093329968390, -26.18160851622837981, 206.9056236797458155 ) ) ;
#20486 = CIRCLE ( 'NONE', #13455, 27.50000000000000000 ) ;
#20487 = CARTESIAN_POINT ( 'NONE',  ( -27.50000000000000000, 3.552713678799999608E-15, 93.60555127549999099 ) ) ;
#20488 = CARTESIAN_POINT ( 'NONE',  ( 1.030413743093000045, -3.909765609533090380, -92.08560516904441329 ) ) ;
#20489 = CARTESIAN_POINT ( 'NONE',  ( -18.66688329739999830, 20.92780155480000204, 230.2432540810000319 ) ) ;
#20490 = CARTESIAN_POINT ( 'NONE',  ( 23.81569860410000317, -13.75000000000000000, 223.8999999999999773 ) ) ;
#20491 = FACE_OUTER_BOUND ( 'NONE', #14410, .T. ) ;
#20492 = CARTESIAN_POINT ( 'NONE',  ( 0.8697582157755545662, -3.930924299790361509, -38.89973510835485371 ) ) ;
#20493 = DIRECTION ( 'NONE',  ( -0.7071067811865475727, 0.7071067811865475727, 0.000000000000000000 ) ) ;
#20494 = CARTESIAN_POINT ( 'NONE',  ( -27.50000000000000000, 3.367667473009999970E-15, 86.39444872359999295 ) ) ;
#20495 = EDGE_LOOP ( 'NONE', ( #30235, #1947, #1794, #8233 ) ) ;
#20496 = CARTESIAN_POINT ( 'NONE',  ( 4.921121033118705412, -0.08698047164986451307, -57.34793411332498891 ) ) ;
#20497 = CARTESIAN_POINT ( 'NONE',  ( 9.897162125403639266, -25.37356426577972002, 91.66046017469999185 ) ) ;
#20498 = ORIENTED_EDGE ( 'NONE', *, *, #20430, .F. ) ;
#20499 = AXIS2_PLACEMENT_3D ( 'NONE', #28834, #16362, #30106 ) ;
#20500 = CARTESIAN_POINT ( 'NONE',  ( 5.320018516182488000, -2.211191048809329374, -17.87122516810000405 ) ) ;
#20501 = VERTEX_POINT ( 'NONE', #11824 ) ;
#20502 = DIRECTION ( 'NONE',  ( -0.7071067811870488384, 0.000000000000000000, -0.7071067811860461960 ) ) ;
#20503 = CARTESIAN_POINT ( 'NONE',  ( -4.005572406160169407, -0.6430491863098631855, -68.10000000002503384 ) ) ;
#20504 = EDGE_LOOP ( 'NONE', ( #24847, #7394, #16102, #7120 ) ) ;
#20505 = DIRECTION ( 'NONE',  ( 0.7600087925169251024, 0.4151946956549595336, 0.4999999999969509945 ) ) ;
#20506 = EDGE_LOOP ( 'NONE', ( #29068, #11919, #8609, #8140 ) ) ;
#20507 = ADVANCED_FACE ( 'NONE', ( #16536 ), #14033, .F. ) ;
#20508 = ORIENTED_EDGE ( 'NONE', *, *, #5387, .F. ) ;
#20509 = AXIS2_PLACEMENT_3D ( 'NONE', #1442, #18577, #16372 ) ;
#20510 = DIRECTION ( 'NONE',  ( -0.9316362575375349842, 0.3633921898465292122, -0.000000000000000000 ) ) ;
#20511 = ORIENTED_EDGE ( 'NONE', *, *, #8887, .F. ) ;
#20512 = DIRECTION ( 'NONE',  ( 0.000000000000000000, -1.000000000000000000, 2.257145581549999994E-12 ) ) ;
#20513 = VECTOR ( 'NONE', #17143, 1000.000000000000114 ) ;
#20514 = LINE ( 'NONE', #18142, #4920 ) ;
#20515 = CARTESIAN_POINT ( 'NONE',  ( -3.807105672867752588, -5.136256491769870536, -64.65409070562499494 ) ) ;
#20516 = CARTESIAN_POINT ( 'NONE',  ( 1.525061067771818824, -28.45945568257947400, 5.498290041128397476 ) ) ;
#20517 = CARTESIAN_POINT ( 'NONE',  ( -7.999999999692422925, -27.47597782790758814, -31.38791861944036654 ) ) ;
#20518 = DIRECTION ( 'NONE',  ( -1.000000000000000000, 0.000000000000000000, 0.000000000000000000 ) ) ;
#20519 = CARTESIAN_POINT ( 'NONE',  ( 8.699999999974995291, -116.4387282421506029, 10.14683980968718835 ) ) ;
#20520 = CARTESIAN_POINT ( 'NONE',  ( -25.05552767696902450, 13.58331698520493269, 3.920132093000017193 ) ) ;
#20521 = CIRCLE ( 'NONE', #11987, 6.000000000000000000 ) ;
#20522 = CARTESIAN_POINT ( 'NONE',  ( 1.708629737455300335, 5.223905898740939691, -10.07047964830000097 ) ) ;
#20523 = CARTESIAN_POINT ( 'NONE',  ( 24.37165445055180157, -14.77472140295711434, 4.999998581000003384 ) ) ;
#20524 = CARTESIAN_POINT ( 'NONE',  ( 19.68705805829999989, 19.53816415229999848, 229.3697640839999963 ) ) ;
#20525 = ORIENTED_EDGE ( 'NONE', *, *, #7267, .F. ) ;
#20526 = DIRECTION ( 'NONE',  ( -0.000000000000000000, -0.000000000000000000, -1.000000000000000000 ) ) ;
#20527 = VECTOR ( 'NONE', #13218, 1000.000000000000000 ) ;
#20528 = FACE_OUTER_BOUND ( 'NONE', #27925, .T. ) ;
#20529 = CARTESIAN_POINT ( 'NONE',  ( 7.105427357599999217E-15, 8.881784196999999612E-15, 43.60555127550000520 ) ) ;
#20530 = CARTESIAN_POINT ( 'NONE',  ( 9.993285220779439371, -25.61999708228226069, 27.99999999999999645 ) ) ;
#20531 = DIRECTION ( 'NONE',  ( 1.000000000000000000, -0.000000000000000000, -2.257150022439999944E-12 ) ) ;
#20532 = PLANE ( 'NONE',  #17703 ) ;
#20533 = AXIS2_PLACEMENT_3D ( 'NONE', #110, #21660, #2608 ) ;
#20534 = CARTESIAN_POINT ( 'NONE',  ( -23.78314118801539934, -14.39461388281613097, 6.098654095000016540 ) ) ;
#20535 = DIRECTION ( 'NONE',  ( -0.7198537139083028835, 0.6941258031311204890, 0.000000000000000000 ) ) ;
#20536 = ORIENTED_EDGE ( 'NONE', *, *, #11306, .T. ) ;
#20537 = EDGE_CURVE ( 'NONE', #2751, #16868, #26294, .T. ) ;
#20538 = FACE_BOUND ( 'NONE', #13031, .T. ) ;
#20539 = CARTESIAN_POINT ( 'NONE',  ( 26.95545381250000361, 8.667969403609998125, 226.2000000000000171 ) ) ;
#20540 = EDGE_CURVE ( 'NONE', #22220, #24506, #19210, .T. ) ;
#20541 = CARTESIAN_POINT ( 'NONE',  ( 2.746262074154482313, -3.444807799140186422, -68.10000000002501963 ) ) ;
#20542 = ADVANCED_FACE ( 'NONE', ( #31015 ), #28794, .T. ) ;
#20543 = AXIS2_PLACEMENT_3D ( 'NONE', #16803, #2498, #29073 ) ;
#20544 = CARTESIAN_POINT ( 'NONE',  ( 21.42460392489384091, 16.40003748012899010, -0.6999999999999784173 ) ) ;
#20545 = CARTESIAN_POINT ( 'NONE',  ( -24.18581885410760179, 13.70860090230524975, 6.072235418731803946 ) ) ;
#20546 = LINE ( 'NONE', #15361, #17695 ) ;
#20547 = CARTESIAN_POINT ( 'NONE',  ( -6.422810504744110638, -10.52451944200381462, 232.6627637660203334 ) ) ;
#20548 = CARTESIAN_POINT ( 'NONE',  ( 4.117846205589238195, 1.989599136607399954, -67.25315453642500074 ) ) ;
#20549 = ORIENTED_EDGE ( 'NONE', *, *, #4532, .T. ) ;
#20550 = CARTESIAN_POINT ( 'NONE',  ( 19.43676870293390735, 19.99999894348004759, 230.3055900836091325 ) ) ;
#20551 = ORIENTED_EDGE ( 'NONE', *, *, #2524, .F. ) ;
#20553 = CARTESIAN_POINT ( 'NONE',  ( 14.25032083473339206, -27.35421241518758961, 0.8585795199999857186 ) ) ;
#20552 = CIRCLE ( 'NONE', #26093, 3.500000000000000444 ) ;
#20554 = ORIENTED_EDGE ( 'NONE', *, *, #24827, .F. ) ;
#20555 = CARTESIAN_POINT ( 'NONE',  ( -11.39269908187263169, 20.99999999989999466, -70.09999999996071551 ) ) ;
#20556 = ADVANCED_FACE ( 'NONE', ( #4896 ), #14642, .T. ) ;
#20557 = CARTESIAN_POINT ( 'NONE',  ( -23.94466870085087606, -15.45669659436210175, 4.319305392000011068 ) ) ;
#20558 = CARTESIAN_POINT ( 'NONE',  ( -12.30000000000833005, -24.37864083493721878, -29.91085694131269790 ) ) ;
#20559 = CARTESIAN_POINT ( 'NONE',  ( -3.072394438959999974, -1.678456730820000020, 230.8356432492296619 ) ) ;
#20560 = CARTESIAN_POINT ( 'NONE',  ( -28.32387083329934185, 4.355427724292508351, 8.000000000000007105 ) ) ;
#20561 = DIRECTION ( 'NONE',  ( 1.000000000000000000, 0.000000000000000000, 0.000000000000000000 ) ) ;
#20562 = ORIENTED_EDGE ( 'NONE', *, *, #27899, .F. ) ;
#20563 = CARTESIAN_POINT ( 'NONE',  ( -24.06826084723317649, 20.50742046750733039, 1.000000000000000888 ) ) ;
#20564 = DIRECTION ( 'NONE',  ( 1.000000000000000000, -1.408687696619999864E-15, 6.771000000000000128E-12 ) ) ;
#20565 = FACE_OUTER_BOUND ( 'NONE', #12317, .T. ) ;
#20566 = CARTESIAN_POINT ( 'NONE',  ( -3.805699214915442052, 0.4083356014457980576, 230.6508329224847103 ) ) ;
#20567 = FACE_OUTER_BOUND ( 'NONE', #14679, .T. ) ;
#20568 = B_SPLINE_CURVE_WITH_KNOTS ( 'NONE', 3,
 ( #16084, #15769, #25382, #3820, #13406, #25696 ),
 .UNSPECIFIED., .F., .F.,
 ( 4, 2, 4 ),
 ( 0.000000000000000000, 0.5000000000000000000, 1.000000000000000000 ),
 .UNSPECIFIED. ) ;
#20569 = DIRECTION ( 'NONE',  ( -0.9316362575375349842, 0.3633921898465292122, -0.000000000000000000 ) ) ;
#20570 = B_SPLINE_CURVE_WITH_KNOTS ( 'NONE', 3,
 ( #7907, #10440, #17958, #22558, #8363, #15771, #8059, #12949, #1003, #29935 ),
 .UNSPECIFIED., .F., .F.,
 ( 4, 2, 2, 2, 4 ),
 ( 0.000000000000000000, 0.2500000000000000000, 0.5000000000000000000, 0.7500000000000000000, 1.000000000000000000 ),
 .UNSPECIFIED. ) ;
#20571 = FACE_OUTER_BOUND ( 'NONE', #29492, .T. ) ;
#20572 = CARTESIAN_POINT ( 'NONE',  ( 1.099998580829999906, -27.77839262550000043, 225.0000014190000002 ) ) ;
#20573 = CARTESIAN_POINT ( 'NONE',  ( -0.9881560945370695404, 5.823346091562972227, -51.25792092402499378 ) ) ;
#20574 = TOROIDAL_SURFACE ( 'NONE', #19077, 30.50000000000000000, 3.000000000000000000 ) ;
#20575 = CARTESIAN_POINT ( 'NONE',  ( 9.993285220779439371, -25.61999708228226069, 202.0000000000000000 ) ) ;
#20576 = CARTESIAN_POINT ( 'NONE',  ( -0.6766242627705201240, 1.992768275178435911, 226.6412452697800006 ) ) ;
#20577 = CARTESIAN_POINT ( 'NONE',  ( 18.11750013309444185, 11.57137507599268389, -4.336808689942017243E-16 ) ) ;
#20578 = CARTESIAN_POINT ( 'NONE',  ( -18.29999999989999893, -27.00000000000000000, -28.39999999989999679 ) ) ;
#20579 = EDGE_CURVE ( 'NONE', #5895, #17734, #19056, .T. ) ;
#20580 = FACE_OUTER_BOUND ( 'NONE', #1190, .T. ) ;
#20581 = VERTEX_POINT ( 'NONE', #17002 ) ;
#20582 = CARTESIAN_POINT ( 'NONE',  ( 4.417684705200791484, 4.247747620870205409, -35.92341724620000321 ) ) ;
#20583 = VERTEX_POINT ( 'NONE', #28652 ) ;
#20584 = CARTESIAN_POINT ( 'NONE',  ( -4.535753307212162078, -3.367775055652930227, -56.75895058492499601 ) ) ;
#20585 = ORIENTED_EDGE ( 'NONE', *, *, #16208, .T. ) ;
#20586 = ORIENTED_EDGE ( 'NONE', *, *, #14582, .T. ) ;
#20587 = ORIENTED_EDGE ( 'NONE', *, *, #24428, .T. ) ;
#20588 = ADVANCED_FACE ( 'NONE', ( #7096 ), #26605, .F. ) ;
#20589 = LINE ( 'NONE', #15876, #28831 ) ;
#20590 = CARTESIAN_POINT ( 'NONE',  ( -31.69999999989999395, 19.99999999999999645, -0.6999999999999992895 ) ) ;
#20591 = CARTESIAN_POINT ( 'NONE',  ( -7.999999999703424791, -29.80249410822368006, -29.47052640025566816 ) ) ;
#20592 = EDGE_CURVE ( 'NONE', #8194, #12035, #27137, .T. ) ;
#20593 = DIRECTION ( 'NONE',  ( 0.000000000000000000, 1.000000000000000000, 0.000000000000000000 ) ) ;
#20594 = CARTESIAN_POINT ( 'NONE',  ( 23.50667118420000179, -14.84174322970000048, 225.0000014190000002 ) ) ;
#20595 = EDGE_CURVE ( 'NONE', #662, #26590, #19525, .T. ) ;
#20596 = CARTESIAN_POINT ( 'NONE',  ( -16.29702427720857472, 11.97108418944526420, -4.336808689942018722E-16 ) ) ;
#20597 = CARTESIAN_POINT ( 'NONE',  ( -1.102325287918849650, -5.983340188646091740, -2.925234013000002520 ) ) ;
#20598 = CARTESIAN_POINT ( 'NONE',  ( 0.5207266838923305663, 1.948929461725765089, 230.8412452700000586 ) ) ;
#20599 = DIRECTION ( 'NONE',  ( 1.000000000000000000, -1.224606353819998843E-16, 0.000000000000000000 ) ) ;
#20600 = EDGE_CURVE ( 'NONE', #29682, #16141, #5082, .T. ) ;
#20601 = CARTESIAN_POINT ( 'NONE',  ( 3.904508939291349900, -1.994718106397494362, -12.41474735220000092 ) ) ;
#20602 = CARTESIAN_POINT ( 'NONE',  ( 5.877945039781666381, 1.734296231098907182, -35.53159726780000227 ) ) ;
#20603 = CARTESIAN_POINT ( 'NONE',  ( 17.04201355855559896, 9.897551528198281545, 0.000000000000000000 ) ) ;
#20604 = CARTESIAN_POINT ( 'NONE',  ( -1.100000000000000533, -26.77741585740000829, 5.097059005707468060 ) ) ;
#20605 = CARTESIAN_POINT ( 'NONE',  ( 8.000000000301639602, -14.95611408989132052, -40.37595097046627046 ) ) ;
#20606 = CARTESIAN_POINT ( 'NONE',  ( 23.39254333661255814, -15.30228500393733526, 8.000000000000007105 ) ) ;
#20607 = CARTESIAN_POINT ( 'NONE',  ( -17.38583936187866996, -28.31016903684225738, -33.41707624599442994 ) ) ;
#20608 = CARTESIAN_POINT ( 'NONE',  ( 22.47598016381773789, 18.14223004230803227, 1.000000000000000888 ) ) ;
#20609 = CIRCLE ( 'NONE', #5535, 26.80000000000000071 ) ;
#20610 = DIRECTION ( 'NONE',  ( 0.9316362575375356503, 0.3633921898465274913, 0.000000000000000000 ) ) ;
#20611 = CARTESIAN_POINT ( 'NONE',  ( 0.5057536231481192246, -27.79562098839016571, 6.099998581000020792 ) ) ;
#20612 = ADVANCED_FACE ( 'NONE', ( #25849 ), #23644, .F. ) ;
#20613 = VERTEX_POINT ( 'NONE', #30717 ) ;
#20614 = CARTESIAN_POINT ( 'NONE',  ( -8.000000000477658801, -25.77531388886969310, -25.66136093485691916 ) ) ;
#20615 = CARTESIAN_POINT ( 'NONE',  ( 10.95000000009999930, -31.44000000000000128, -28.39999999989999679 ) ) ;
#20616 = ORIENTED_EDGE ( 'NONE', *, *, #879, .F. ) ;
#20617 = CARTESIAN_POINT ( 'NONE',  ( -23.09961856954875614, -13.58841269839368771, 223.9123094310619422 ) ) ;
#20618 = CARTESIAN_POINT ( 'NONE',  ( 3.930748841427598173, 1.248291629424108651, -38.08800167882662890 ) ) ;
#20619 = CARTESIAN_POINT ( 'NONE',  ( 0.8178294365284820566, -26.78758452998259187, 4.262774516068433606 ) ) ;
#20620 = ORIENTED_EDGE ( 'NONE', *, *, #2315, .F. ) ;
#20621 = TOROIDAL_SURFACE ( 'NONE', #3035, 24.50000000000000000, 3.200000000000000178 ) ;
#20622 = CARTESIAN_POINT ( 'NONE',  ( -4.933588760076017543, -27.05494253741617428, 20.48841368488172776 ) ) ;
#20623 = ORIENTED_EDGE ( 'NONE', *, *, #23789, .T. ) ;
#20624 = EDGE_CURVE ( 'NONE', #17664, #23969, #4588, .T. ) ;
#20625 = ORIENTED_EDGE ( 'NONE', *, *, #27121, .T. ) ;
#20626 = SHAPE_REPRESENTATION ( 'Nut M6', ( #17722 ), #23366 ) ;
#20627 = ORIENTED_EDGE ( 'NONE', *, *, #30294, .F. ) ;
#20628 = B_SPLINE_CURVE_WITH_KNOTS ( 'NONE', 3,
 ( #20070, #19447, #21810, #7484, #15182, #17079 ),
 .UNSPECIFIED., .F., .F.,
 ( 4, 2, 4 ),
 ( 0.000000000000000000, 0.5000000000000000000, 1.000000000000000000 ),
 .UNSPECIFIED. ) ;
#20629 = CARTESIAN_POINT ( 'NONE',  ( -1.127665019380000189, -28.47796022459999676, 224.8959436220000043 ) ) ;
#20630 = B_SPLINE_CURVE_WITH_KNOTS ( 'NONE', 1,
 ( #30690, #21094 ),
 .UNSPECIFIED., .F., .F.,
 ( 2, 2 ),
 ( -0.7016521142910000508, 3.330669073875469621E-15 ),
 .UNSPECIFIED. ) ;
#20631 = ORIENTED_EDGE ( 'NONE', *, *, #29108, .T. ) ;
#20632 = CARTESIAN_POINT ( 'NONE',  ( -25.22069443620000229, -13.27363204220000092, 225.2084371580000095 ) ) ;
#20633 = ORIENTED_EDGE ( 'NONE', *, *, #24170, .T. ) ;
#20634 = CARTESIAN_POINT ( 'NONE',  ( 2.885864564934697896, 2.548163973319825359, -35.70000000000000284 ) ) ;
#20635 = STYLED_ITEM ( 'NONE', ( #16994 ), #121 ) ;
#20636 = CARTESIAN_POINT ( 'NONE',  ( -0.6094664100040195764, -28.49364619262437870, 4.895947184000021046 ) ) ;
#20637 = CARTESIAN_POINT ( 'NONE',  ( 13.65677330047603633, -23.08588181436693176, -1.399999999999998801 ) ) ;
#20638 = CARTESIAN_POINT ( 'NONE',  ( 23.68823177919582434, -12.53428999841347746, 5.486606152542477410 ) ) ;
#20639 = CARTESIAN_POINT ( 'NONE',  ( 24.05454679444040167, -13.93760249370175508, 4.035491118591038706 ) ) ;
#20640 = ORIENTED_EDGE ( 'NONE', *, *, #13209, .F. ) ;
#20641 = CARTESIAN_POINT ( 'NONE',  ( 0.6465148687764388225, -4.727082501367554812, -1.310624048000003095 ) ) ;
#20642 = CARTESIAN_POINT ( 'NONE',  ( -5.902313038799129608, -1.548398769286710053, -24.44656121679999927 ) ) ;
#20643 = CYLINDRICAL_SURFACE ( 'NONE', #17348, 26.80000000000002203 ) ;
#20644 =( REPRESENTATION_RELATIONSHIP ('NONE','NONE', #2712, #339 ) REPRESENTATION_RELATIONSHIP_WITH_TRANSFORMATION ( #27502 )SHAPE_REPRESENTATION_RELATIONSHIP( ) );
#20645 = CARTESIAN_POINT ( 'NONE',  ( 5.414213562369999622, -31.28896728272270877, -80.26658230080884948 ) ) ;
#20646 = CARTESIAN_POINT ( 'NONE',  ( 2.888061030912462801, -2.091444806055747563, -88.52261276308685467 ) ) ;
#20647 = CARTESIAN_POINT ( 'NONE',  ( -10.00000000000000000, 22.06507305262541863, -61.91147751336289673 ) ) ;
#20648 = CARTESIAN_POINT ( 'NONE',  ( -3.683257989657598319, -1.493295482194435086, -96.33992724130713725 ) ) ;
#20649 = CARTESIAN_POINT ( 'NONE',  ( -24.43799431770000297, -14.66523353640000060, 226.0028091380000035 ) ) ;
#20650 = VECTOR ( 'NONE', #26393, 1000.000000000000000 ) ;
#20651 = CARTESIAN_POINT ( 'NONE',  ( 24.28117756992811493, -12.91036561250576220, 224.4438356455087273 ) ) ;
#20652 = CARTESIAN_POINT ( 'NONE',  ( 6.408200674649999762, -17.12117065109999814, 230.6999999999999886 ) ) ;
#20653 = CARTESIAN_POINT ( 'NONE',  ( 7.670601361110000127, 15.86076312269999988, 230.0904314459999966 ) ) ;
#20654 = EDGE_CURVE ( 'NONE', #11991, #13180, #6480, .T. ) ;
#20655 = B_SPLINE_CURVE_WITH_KNOTS ( 'NONE', 5,
 ( #24761, #1008, #29783, #22248, #10297, #25071, #22709, #22099, #12803, #854, #19894, #29477 ),
 .UNSPECIFIED., .F., .F.,
 ( 6, 3, 3, 6 ),
 ( 0.000000000000000000, 2.812352518870000040, 5.624713923559999884, 7.679355242909999824 ),
 .UNSPECIFIED. ) ;
#20656 = VERTEX_POINT ( 'NONE', #15925 ) ;
#20657 = CARTESIAN_POINT ( 'NONE',  ( 4.855544147916073250, 1.989531035200713838, -60.14141554682500868 ) ) ;
#20658 = B_SPLINE_CURVE_WITH_KNOTS ( 'NONE', 3,
 ( #812, #25026, #6296, #30050, #27529, #3152 ),
 .UNSPECIFIED., .F., .F.,
 ( 4, 2, 4 ),
 ( 0.000000000000000000, 0.5000000000000000000, 1.000000000000000000 ),
 .UNSPECIFIED. ) ;
#20659 = DIRECTION ( 'NONE',  ( 0.000000000000000000, 0.9396926207858125046, 0.3420201433259318358 ) ) ;
#20660 = ORIENTED_EDGE ( 'NONE', *, *, #13898, .T. ) ;
#20661 = EDGE_CURVE ( 'NONE', #16790, #4605, #15879, .T. ) ;
#20662 = CARTESIAN_POINT ( 'NONE',  ( -4.338779899226326009, -4.343559731693466652, -9.813991631000003935 ) ) ;
#20663 = ORIENTED_EDGE ( 'NONE', *, *, #16598, .F. ) ;
#20664 = ADVANCED_FACE ( 'NONE', ( #6330 ), #4287, .T. ) ;
#20665 = CARTESIAN_POINT ( 'NONE',  ( 7.999999999994834354, -111.9817663810474642, 5.760339591636753021 ) ) ;
#20666 = CARTESIAN_POINT ( 'NONE',  ( 14.40197535836999876, -22.00000000000000000, -31.28675134584999640 ) ) ;
#20667 = ADVANCED_FACE ( 'NONE', ( #13721 ), #4585, .F. ) ;
#20668 = ORIENTED_EDGE ( 'NONE', *, *, #6189, .T. ) ;
#20669 = CARTESIAN_POINT ( 'NONE',  ( 10.69999999989999928, 19.99999999999999645, -2.399999999999999467 ) ) ;
#20670 = VERTEX_POINT ( 'NONE', #16082 ) ;
#20671 = ORIENTED_EDGE ( 'NONE', *, *, #10344, .T. ) ;
#20672 = DIRECTION ( 'NONE',  ( -1.000000000000000000, 0.000000000000000000, 0.000000000000000000 ) ) ;
#20673 = ORIENTED_EDGE ( 'NONE', *, *, #3522, .F. ) ;
#20674 = LINE ( 'NONE', #15948, #17469 ) ;
#20675 = DIRECTION ( 'NONE',  ( 0.9316362575375356503, 0.3633921898465274913, 0.000000000000000000 ) ) ;
#20676 = CARTESIAN_POINT ( 'NONE',  ( 2.917330641183085049, 3.968100254485465328, -65.89226422532500749 ) ) ;
#20677 = CARTESIAN_POINT ( 'NONE',  ( 20.12213002960000097, -20.25093488000000264, 229.9751245540000184 ) ) ;
#20678 = AXIS2_PLACEMENT_3D ( 'NONE', #151, #11790, #14770 ) ;
#20679 = CARTESIAN_POINT ( 'NONE',  ( -9.999999999969999109, -24.87872937729999734, -30.52127062079999931 ) ) ;
#20680 = DIRECTION ( 'NONE',  ( -5.962915006522622422E-16, -0.4383711467890810676, -0.8987940462991651502 ) ) ;
#20681 = CARTESIAN_POINT ( 'NONE',  ( 7.636659491129999644, 9.305401069029999306, 224.6412452697800290 ) ) ;
#20682 = VERTEX_POINT ( 'NONE', #25535 ) ;
#20683 = CARTESIAN_POINT ( 'NONE',  ( -26.57440607989999748, -3.469982107200002108, -1.399999999999998579 ) ) ;
#20684 = CARTESIAN_POINT ( 'NONE',  ( -6.108812354267502798, 0.1812703649498176306, -12.58304957890000253 ) ) ;
#20685 = FACE_OUTER_BOUND ( 'NONE', #17114, .T. ) ;
#20686 = CARTESIAN_POINT ( 'NONE',  ( 10.70000000009999930, -27.00000000000000000, -28.39999999989999679 ) ) ;
#20687 = ORIENTED_EDGE ( 'NONE', *, *, #7196, .T. ) ;
#20688 = LINE ( 'NONE', #10772, #8632 ) ;
#20689 = DIRECTION ( 'NONE',  ( 0.000000000000000000, 0.000000000000000000, 1.000000000000000000 ) ) ;
#20690 = CARTESIAN_POINT ( 'NONE',  ( -25.64086162999999630, 11.13108295319999819, 222.0000000000000000 ) ) ;
#20691 = CARTESIAN_POINT ( 'NONE',  ( 21.24683659263830293, 17.15008680908327321, 0.000000000000000000 ) ) ;
#20692 = CYLINDRICAL_SURFACE ( 'NONE', #30390, 2.100000000000000977 ) ;
#20693 = CARTESIAN_POINT ( 'NONE',  ( 2.743362564037614248, -4.941860934411918649, -55.58172062782499268 ) ) ;
#20694 = CARTESIAN_POINT ( 'NONE',  ( -23.62421573606080827, -14.65442406347138338, 6.042470790000031400 ) ) ;
#20695 = LINE ( 'NONE', #27304, #7733 ) ;
#20696 = ORIENTED_EDGE ( 'NONE', *, *, #20844, .T. ) ;
#20697 = CARTESIAN_POINT ( 'NONE',  ( 24.70074545465923421, -14.21822122957792445, 3.997190862000010725 ) ) ;
#20698 = CARTESIAN_POINT ( 'NONE',  ( 27.79999999999999716, -2.355675019179999893E-11, 223.3999999999999773 ) ) ;
#20699 = VECTOR ( 'NONE', #13925, 1000.000000000000114 ) ;
#20700 = CARTESIAN_POINT ( 'NONE',  ( 2.412358317651485784, -3.532528282628375926, -68.10000000002500542 ) ) ;
#20701 = EDGE_CURVE ( 'NONE', #14380, #4065, #20174, .T. ) ;
#20702 = VECTOR ( 'NONE', #19092, 1000.000000000000000 ) ;
#20703 = CARTESIAN_POINT ( 'NONE',  ( 8.699999999522411542, -24.26136093482726608, -29.62468611105379779 ) ) ;
#20704 = CARTESIAN_POINT ( 'NONE',  ( -4.258588862633405192, 0.9647698903526967795, -44.10000000002498410 ) ) ;
#20705 = SURFACE_STYLE_FILL_AREA ( #23227 ) ;
#20706 = CARTESIAN_POINT ( 'NONE',  ( 14.55660443455961328, -22.46388722856030640, -31.55457676213481477 ) ) ;
#20707 = CARTESIAN_POINT ( 'NONE',  ( 304364.2709395335405, -388808.3216389999725, -78777.77829863908119 ) ) ;
#20708 = CARTESIAN_POINT ( 'NONE',  ( -1.595193757947241497, 6.212219048941578059, -66.20876360962500939 ) ) ;
#20709 = ORIENTED_EDGE ( 'NONE', *, *, #15160, .T. ) ;
#20710 = CARTESIAN_POINT ( 'NONE',  ( 19.42269931435233588, 19.99999652952873319, 230.3137021383872138 ) ) ;
#20711 = ORIENTED_EDGE ( 'NONE', *, *, #22380, .F. ) ;
#20712 = CARTESIAN_POINT ( 'NONE',  ( 0.5632927345713620859, -3.521042344241311017, -88.52261276296684400 ) ) ;
#20713 = ORIENTED_EDGE ( 'NONE', *, *, #15730, .T. ) ;
#20714 = CARTESIAN_POINT ( 'NONE',  ( -11.69999999989999928, -24.11120071670000087, -0.6999999999999992895 ) ) ;
#20715 = CIRCLE ( 'NONE', #29262, 3.750000000000000000 ) ;
#20716 = EDGE_CURVE ( 'NONE', #8641, #3121, #13568, .T. ) ;
#20717 =( NAMED_UNIT ( * ) SI_UNIT ( $, .STERADIAN. ) SOLID_ANGLE_UNIT ( ) );
#20718 = CARTESIAN_POINT ( 'NONE',  ( -1.484924240490000047, 1.484924240490000047, 227.6412452697800006 ) ) ;
#20719 = DIRECTION ( 'NONE',  ( 1.000000000000000000, 0.000000000000000000, 0.000000000000000000 ) ) ;
#20720 = CARTESIAN_POINT ( 'NONE',  ( -10.69999999999999929, -24.00000000000000000, -28.40000000000000213 ) ) ;
#20721 = CARTESIAN_POINT ( 'NONE',  ( -12.34127026248313364, -22.00000000000000711, -27.51269861918589044 ) ) ;
#20722 = CARTESIAN_POINT ( 'NONE',  ( -1.419173372180000084E-06, -27.80022181310000207, 223.9000014189999774 ) ) ;
#20723 = ORIENTED_EDGE ( 'NONE', *, *, #10118, .F. ) ;
#20724 = CARTESIAN_POINT ( 'NONE',  ( 28.35945635836379708, 7.983396865348648674, 8.000000000000007105 ) ) ;
#20725 = DIRECTION ( 'NONE',  ( 1.224606353819999829E-16, 1.000000000000000000, 0.000000000000000000 ) ) ;
#20726 = ADVANCED_FACE ( 'NONE', ( #11833 ), #11673, .T. ) ;
#20727 = DIRECTION ( 'NONE',  ( 1.000000000000000000, 0.000000000000000000, 0.000000000000000000 ) ) ;
#20728 = B_SPLINE_CURVE_WITH_KNOTS ( 'NONE', 3,
 ( #21803, #16759, #26377, #9998, #4820, #19598, #29177, #16455, #12822, #7779 ),
 .UNSPECIFIED., .F., .F.,
 ( 4, 2, 2, 2, 4 ),
 ( 0.000000000000000000, 0.2500000000000000000, 0.5000000000000000000, 0.7500000000000000000, 1.000000000000000000 ),
 .UNSPECIFIED. ) ;
#20729 = CARTESIAN_POINT ( 'NONE',  ( -2.953785065807760457, 1.883894191386363381, 230.8358359828810364 ) ) ;
#20730 = CARTESIAN_POINT ( 'NONE',  ( -24.15901410609999900, -15.12012600319999933, 225.5071239680000303 ) ) ;
#20731 = CARTESIAN_POINT ( 'NONE',  ( 8.700000000111513643, -60.34578018690913837, -2.533826264234904091 ) ) ;
#20732 = CARTESIAN_POINT ( 'NONE',  ( 23.46464814832361157, 14.90844422066722430, 4.118060943961503462 ) ) ;
#20733 = CARTESIAN_POINT ( 'NONE',  ( -27.23548387060000309, 8.881784196999999612E-15, 191.6604601750000256 ) ) ;
#20734 = CARTESIAN_POINT ( 'NONE',  ( 4.085013927406620837, 4.246146200131522441, -47.89426496242500519 ) ) ;
#20735 = CARTESIAN_POINT ( 'NONE',  ( 14.80686173019908125, -23.75137256601108149, -24.50209323151165108 ) ) ;
#20736 = CARTESIAN_POINT ( 'NONE',  ( 7.160801144637284565, 5.243561765918017592, -40.03662512451870015 ) ) ;
#20737 = CARTESIAN_POINT ( 'NONE',  ( -17.10083289438509979, 9.923792022609076113, -0.000000000000000000 ) ) ;
#20738 = CIRCLE ( 'NONE', #12191, 7.354069295110000404 ) ;
#20739 = CYLINDRICAL_SURFACE ( 'NONE', #26813, 3.000000000000002220 ) ;
#20740 = ORIENTED_EDGE ( 'NONE', *, *, #29031, .F. ) ;
#20741 = CARTESIAN_POINT ( 'NONE',  ( 0.1051796283266584475, -6.084780997910130829, -34.01110030499999937 ) ) ;
#20742 = ORIENTED_EDGE ( 'NONE', *, *, #10992, .F. ) ;
#20743 = EDGE_CURVE ( 'NONE', #6498, #18537, #23748, .T. ) ;
#20744 = CARTESIAN_POINT ( 'NONE',  ( 0.7192951553254764985, 4.518739695583327887, -54.41500058692499664 ) ) ;
#20745 = VERTEX_POINT ( 'NONE', #20962 ) ;
#20746 = ORIENTED_EDGE ( 'NONE', *, *, #30316, .T. ) ;
#20747 = ORIENTED_EDGE ( 'NONE', *, *, #21123, .T. ) ;
#20748 = SURFACE_STYLE_USAGE ( .BOTH. , #6276 ) ;
#20749 = DIRECTION ( 'NONE',  ( 1.000000000000000000, 0.000000000000000000, 0.000000000000000000 ) ) ;
#20750 = LINE ( 'NONE', #20434, #401 ) ;
#20751 = DIRECTION ( 'NONE',  ( 0.000000000000000000, 0.000000000000000000, 1.000000000000000000 ) ) ;
#20752 = CARTESIAN_POINT ( 'NONE',  ( -16.56625540545879360, -7.923010675351982002, -0.6999999999999784173 ) ) ;
#20753 = CARTESIAN_POINT ( 'NONE',  ( -4.439228537916153350, -2.748747741535113587, -0.6999999999999992895 ) ) ;
#20754 = CARTESIAN_POINT ( 'NONE',  ( -2.624260084387262104, -3.463915187244965388, -3.228945369299999868 ) ) ;
#20755 = AXIS2_PLACEMENT_3D ( 'NONE', #19652, #29854, #8288 ) ;
#20756 = CARTESIAN_POINT ( 'NONE',  ( 10.69999999999999929, -29.12132034360000077, -30.52132034359999935 ) ) ;
#20757 = PLANE ( 'NONE',  #7461 ) ;
#20758 = EDGE_CURVE ( 'NONE', #19797, #2099, #18890, .T. ) ;
#20759 = CARTESIAN_POINT ( 'NONE',  ( 6.482330152203070739, 0.4632910120546396282, -15.24454535870000527 ) ) ;
#20760 = CARTESIAN_POINT ( 'NONE',  ( 4.618385388201741826, 1.362661324479865099, -34.59409726779999517 ) ) ;
#20761 = DIRECTION ( 'NONE',  ( 1.000000000000000000, 0.000000000000000000, 0.000000000000000000 ) ) ;
#20762 = CARTESIAN_POINT ( 'NONE',  ( 8.000000000232340369, -25.77531388888444752, -25.66136093478154123 ) ) ;
#20763 = CARTESIAN_POINT ( 'NONE',  ( 0.3832430167609999772, -28.49789927060000139, 223.9576737099999946 ) ) ;
#20764 = CARTESIAN_POINT ( 'NONE',  ( 28.32389467614452627, -4.355430725511089562, 8.000000000000007105 ) ) ;
#20765 = CARTESIAN_POINT ( 'NONE',  ( -3.340912886194220111, 1.213242220896334045, 227.6700366507570834 ) ) ;
#20766 = B_SPLINE_CURVE_WITH_KNOTS ( 'NONE', 5,
 ( #7600, #19101, #228, #5085, #14694, #24283 ),
 .UNSPECIFIED., .F., .F.,
 ( 6, 6 ),
 ( 0.000000000000000000, 2.319814892410000162 ),
 .UNSPECIFIED. ) ;
#20767 = CARTESIAN_POINT ( 'NONE',  ( 19.80538173989999962, 19.50875420239999869, 227.7999999360000061 ) ) ;
#20768 = CARTESIAN_POINT ( 'NONE',  ( 1.692897434406342549, -3.097451722116522976, 226.6412452697750268 ) ) ;
#20769 = CARTESIAN_POINT ( 'NONE',  ( -0.5821515579339680002, -27.79407096281863687, 4.791896188000022150 ) ) ;
#20770 = EDGE_CURVE ( 'NONE', #9833, #28814, #3842, .T. ) ;
#20771 = VECTOR ( 'NONE', #21088, 1000.000000000000114 ) ;
#20772 = EDGE_CURVE ( 'NONE', #5681, #7965, #5726, .T. ) ;
#20773 = CARTESIAN_POINT ( 'NONE',  ( -2.783363191001295700, -3.225935323956106604, -70.05247398454777397 ) ) ;
#20774 = ORIENTED_EDGE ( 'NONE', *, *, #12651, .F. ) ;
#20775 = PRESENTATION_LAYER_ASSIGNMENT (  '', '', ( #3182 ) ) ;
#20776 = CARTESIAN_POINT ( 'NONE',  ( 0.8585117870642997584, -3.500000000000000444, 227.7058346192808642 ) ) ;
#20777 = CARTESIAN_POINT ( 'NONE',  ( 4.006917070325392238, 0.8005523405751613364, -37.86962463647368082 ) ) ;
#20778 = CARTESIAN_POINT ( 'NONE',  ( -0.6848972644784130370, -5.175796693238598145, -0.7000250125985852945 ) ) ;
#20780 = ORIENTED_EDGE ( 'NONE', *, *, #22973, .F. ) ;
#20779 = AXIS2_PLACEMENT_3D ( 'NONE', #29261, #8156, #498 ) ;
#20781 = FACE_OUTER_BOUND ( 'NONE', #2422, .T. ) ;
#20782 = ORIENTED_EDGE ( 'NONE', *, *, #23903, .F. ) ;
#20783 = VERTEX_POINT ( 'NONE', #12292 ) ;
#20784 = EDGE_CURVE ( 'NONE', #21744, #29682, #189, .T. ) ;
#20785 = B_SPLINE_CURVE_WITH_KNOTS ( 'NONE', 3,
 ( #18004, #18489, #28087, #6533, #16129, #25741 ),
 .UNSPECIFIED., .F., .F.,
 ( 4, 2, 4 ),
 ( 0.000000000000000000, 0.5000000000000000000, 1.000000000000000000 ),
 .UNSPECIFIED. ) ;
#20786 = ORIENTED_EDGE ( 'NONE', *, *, #16433, .T. ) ;
#20787 = FACE_OUTER_BOUND ( 'NONE', #19465, .T. ) ;
#20788 = ORIENTED_EDGE ( 'NONE', *, *, #17444, .F. ) ;
#20789 = CARTESIAN_POINT ( 'NONE',  ( -24.50074272580000212, -13.13701158850000006, 225.6808342349999918 ) ) ;
#20790 = CARTESIAN_POINT ( 'NONE',  ( 24.06750537026301018, 15.26514225575822081, 4.098700193000015091 ) ) ;
#20791 =( NAMED_UNIT ( * ) PLANE_ANGLE_UNIT ( ) SI_UNIT ( $, .RADIAN. ) );
#20792 = CARTESIAN_POINT ( 'NONE',  ( -3.883058903150518049, -2.773382390028514610, -95.04434131332580193 ) ) ;
#20793 = EDGE_CURVE ( 'NONE', #22642, #2258, #3495, .T. ) ;
#20794 = CARTESIAN_POINT ( 'NONE',  ( -10.35000000009999965, 19.99999999999999645, -42.40000000045999684 ) ) ;
#20795 = CARTESIAN_POINT ( 'NONE',  ( -26.62824275575433930, -3.502825096380762115, 0.000000000000000000 ) ) ;
#20796 = VECTOR ( 'NONE', #27963, 1000.000000000000000 ) ;
#20797 = PLANE ( 'NONE',  #4959 ) ;
#20798 = AXIS2_PLACEMENT_3D ( 'NONE', #4528, #25782, #10988 ) ;
#20799 = ORIENTED_EDGE ( 'NONE', *, *, #15979, .T. ) ;
#20800 = CARTESIAN_POINT ( 'NONE',  ( 5.214500487626152037, -1.910846663805727541, -6.836105321700002513 ) ) ;
#20801 = CARTESIAN_POINT ( 'NONE',  ( 5.972505199797514486, -1.290950946386169917, -23.19036215650000088 ) ) ;
#20802 = AXIS2_PLACEMENT_3D ( 'NONE', #2369, #28780, #21881 ) ;
#20803 = CARTESIAN_POINT ( 'NONE',  ( -9.993285220779418054, -25.61999708228225714, 202.5329093469738666 ) ) ;
#20804 = CARTESIAN_POINT ( 'NONE',  ( 3.326321175718020218, -1.384230705528964878, -93.72782450567366652 ) ) ;
#20805 = CARTESIAN_POINT ( 'NONE',  ( -0.9470189794544437989, 3.499851337386774119, 227.7188583759513847 ) ) ;
#20806 = CARTESIAN_POINT ( 'NONE',  ( 0.000000000000000000, 0.000000000000000000, 210.0000000000000284 ) ) ;
#20807 = CARTESIAN_POINT ( 'NONE',  ( 10.00000000070000183, -130.0000000000000000, -41.24671599790000442 ) ) ;
#20808 = EDGE_CURVE ( 'NONE', #21002, #3946, #16692, .T. ) ;
#20809 = MANIFOLD_SOLID_BREP ( 'PartBody', #19085 ) ;
#20810 = CARTESIAN_POINT ( 'NONE',  ( 6.999999999944251705, -114.9756814442911264, 22.27940384858688816 ) ) ;
#20811 = FACE_OUTER_BOUND ( 'NONE', #2448, .T. ) ;
#20812 = CARTESIAN_POINT ( 'NONE',  ( -22.97825597456790092, -13.83688083289194992, -1.399999999999998579 ) ) ;
#20813 = ORIENTED_EDGE ( 'NONE', *, *, #782, .T. ) ;
#20814 = CARTESIAN_POINT ( 'NONE',  ( -1.143212971672624478, -4.711439499498765393, -61.54311227092500758 ) ) ;
#20815 = PLANE ( 'NONE',  #25360 ) ;
#20816 = ORIENTED_EDGE ( 'NONE', *, *, #20031, .T. ) ;
#20817 = CARTESIAN_POINT ( 'NONE',  ( 25.46997661260000001, 13.23369636690000029, 222.0000000000000000 ) ) ;
#20818 = CARTESIAN_POINT ( 'NONE',  ( 6.379535387291454640, -1.442012952481606991, -32.78377053309999667 ) ) ;
#20819 = VERTEX_POINT ( 'NONE', #24412 ) ;
#20820 = SHAPE_REPRESENTATION ( 'Bolt M6', ( #17722 ), #13276 ) ;
#20821 = CARTESIAN_POINT ( 'NONE',  ( -23.84638031100276123, 14.29033435813013853, 4.441358500814834187 ) ) ;
#20822 = CARTESIAN_POINT ( 'NONE',  ( -2.486632795208609803, -3.039739661661432280, -68.10000000002499121 ) ) ;
#20823 = VECTOR ( 'NONE', #22095, 1000.000000000000114 ) ;
#20824 = ORIENTED_EDGE ( 'NONE', *, *, #20793, .T. ) ;
#20825 = AXIS2_PLACEMENT_3D ( 'NONE', #8404, #28238, #25740 ) ;
#20826 = ORIENTED_EDGE ( 'NONE', *, *, #9506, .F. ) ;
#20827 = AXIS2_PLACEMENT_3D ( 'NONE', #12372, #16935, #26542 ) ;
#20828 = EDGE_LOOP ( 'NONE', ( #5674, #29668, #10711, #701 ) ) ;
#20829 = AXIS2_PLACEMENT_3D ( 'NONE', #24560, #29267, #20727 ) ;
#20830 = DIRECTION ( 'NONE',  ( 0.9690327085533227969, 0.2219413702013694756, -0.1082480389981703706 ) ) ;
#20831 = AXIS2_PLACEMENT_3D ( 'NONE', #14269, #4827, #2157 ) ;
#20832 = EDGE_LOOP ( 'NONE', ( #26594, #3022, #19394, #19823, #8555, #29329, #28323, #25236 ) ) ;
#20833 = DIRECTION ( 'NONE',  ( 0.000000000000000000, 1.000000000000000000, 0.000000000000000000 ) ) ;
#20834 = CARTESIAN_POINT ( 'NONE',  ( 3.466821295769682159E-14, -2.890242878314739659E-13, 27.99999999999999645 ) ) ;
#20835 = CARTESIAN_POINT ( 'NONE',  ( -3.447099378712505935, 3.428612291819206792, -68.19322600342499641 ) ) ;
#20836 = CARTESIAN_POINT ( 'NONE',  ( 5.225008591809999992, -30.81438311299999810, 229.2930790960000138 ) ) ;
#20837 = CARTESIAN_POINT ( 'NONE',  ( -2.664535259099999568E-14, -26.80000000000000071, 223.8999999999999773 ) ) ;
#20838 = EDGE_CURVE ( 'NONE', #12344, #29903, #19537, .T. ) ;
#20839 = CARTESIAN_POINT ( 'NONE',  ( 8.000000000236575204, -29.80249033211431708, -29.47052495773638370 ) ) ;
#20840 = CARTESIAN_POINT ( 'NONE',  ( -23.60764285266575868, -12.68553248570766456, 5.737227008375342052 ) ) ;
#20841 = FACE_OUTER_BOUND ( 'NONE', #8902, .T. ) ;
#20842 = EDGE_LOOP ( 'NONE', ( #135, #7507, #8934, #6974 ) ) ;
#20843 = CARTESIAN_POINT ( 'NONE',  ( -22.63992238019999803, -14.34133587289999845, 225.0000000000000000 ) ) ;
#20844 = EDGE_CURVE ( 'NONE', #29055, #8641, #10977, .T. ) ;
#20845 = CARTESIAN_POINT ( 'NONE',  ( -1.184025259985572953, -4.532227402022651397, -12.55022317840000312 ) ) ;
#20846 = LINE ( 'NONE', #30449, #19352 ) ;
#20847 = EDGE_CURVE ( 'NONE', #25525, #6418, #13244, .T. ) ;
#20848 = B_SPLINE_CURVE_WITH_KNOTS ( 'NONE', 3,
 ( #24256, #17922, #15275, #20457, #3461, #20614 ),
 .UNSPECIFIED., .F., .F.,
 ( 4, 2, 4 ),
 ( 0.000000000000000000, 0.5000000000000000000, 1.000000000000000000 ),
 .UNSPECIFIED. ) ;
#20849 = AXIS2_PLACEMENT_3D ( 'NONE', #26122, #11641, #30838 ) ;
#20850 = CARTESIAN_POINT ( 'NONE',  ( 0.000000000000000000, 3.552713678799999608E-15, 193.2171415880000040 ) ) ;
#20851 = ORIENTED_EDGE ( 'NONE', *, *, #19098, .T. ) ;
#20852 = CARTESIAN_POINT ( 'NONE',  ( -8.699999998974114135, -28.22468611108677194, -31.13863906519358693 ) ) ;
#20853 = CARTESIAN_POINT ( 'NONE',  ( 0.8794532062878365197, -27.78659480101269708, 3.957673652000032405 ) ) ;
#20854 = CIRCLE ( 'NONE', #25890, 27.50000000000000000 ) ;
#20855 = CARTESIAN_POINT ( 'NONE',  ( -8.699999999684472130, -15.22718887828181522, -33.11694077318242790 ) ) ;
#20856 = VECTOR ( 'NONE', #16393, 1000.000000000000000 ) ;
#20857 = DIRECTION ( 'NONE',  ( 0.8660254037843289066, -0.5000000000001899592, 0.000000000000000000 ) ) ;
#20858 = CARTESIAN_POINT ( 'NONE',  ( 11.06030393429999847, -24.60936423240000082, -1.629296559500004182 ) ) ;
#20859 = B_SPLINE_CURVE_WITH_KNOTS ( 'NONE', 3,
 ( #17437, #27652, #12714, #5480, #7834, #8136, #25144, #10368 ),
 .UNSPECIFIED., .F., .F.,
 ( 4, 2, 2, 4 ),
 ( 0.000000000000000000, 0.2499999999999999445, 0.4999999999999998890, 1.000000000000000000 ),
 .UNSPECIFIED. ) ;
#20860 = CARTESIAN_POINT ( 'NONE',  ( 3.599561039400463347, 4.779710538180673041, -54.62619010302499589 ) ) ;
#20861 = CARTESIAN_POINT ( 'NONE',  ( 8.000000000245886866, -28.22468611110216230, -31.13863906511491209 ) ) ;
#20862 = DIRECTION ( 'NONE',  ( -1.000000000000000000, 1.224646799149999589E-16, 0.000000000000000000 ) ) ;
#20863 = ORIENTED_EDGE ( 'NONE', *, *, #23502, .F. ) ;
#20864 = SURFACE_STYLE_USAGE ( .BOTH. , #4019 ) ;
#20865 = CARTESIAN_POINT ( 'NONE',  ( -17.83929479963776288, 19.99998902616253105, -0.6999999999999784173 ) ) ;
#20866 = CARTESIAN_POINT ( 'NONE',  ( 1.172141357840190468, -3.890077810869508657, -68.10000000002501963 ) ) ;
#20867 = AXIS2_PLACEMENT_3D ( 'NONE', #22586, #10315, #29961 ) ;
#20868 = LINE ( 'NONE', #6535, #710 ) ;
#20869 = CARTESIAN_POINT ( 'NONE',  ( -4.332055453559614300, 1.117314083138565284, -44.10000000002499121 ) ) ;
#20870 = DIRECTION ( 'NONE',  ( 1.000000000000000000, 0.000000000000000000, 0.000000000000000000 ) ) ;
#20871 = MANIFOLD_SOLID_BREP ( 'PartBody', #18583 ) ;
#20872 = ORIENTED_EDGE ( 'NONE', *, *, #1482, .F. ) ;
#20873 = CARTESIAN_POINT ( 'NONE',  ( 12.12499559729999810, 21.69999999929999390, -55.73512174120000395 ) ) ;
#20874 = CARTESIAN_POINT ( 'NONE',  ( 4.117846205589234643, 1.989599136607407504, -66.85315453642499506 ) ) ;
#20875 = CIRCLE ( 'NONE', #19865, 27.92857142860000152 ) ;
#20876 = VERTEX_POINT ( 'NONE', #29736 ) ;
#20877 = DIRECTION ( 'NONE',  ( -0.3633921898465292122, -0.9316362575375349842, 0.000000000000000000 ) ) ;
#20878 = VERTEX_POINT ( 'NONE', #19847 ) ;
#20879 = CARTESIAN_POINT ( 'NONE',  ( -19.68707896189999929, 19.53815547089999782, 229.3695869349999725 ) ) ;
#20880 = VERTEX_POINT ( 'NONE', #29428 ) ;
#20881 = DIRECTION ( 'NONE',  ( -1.000000000000000000, 0.000000000000000000, 0.000000000000000000 ) ) ;
#20882 = CARTESIAN_POINT ( 'NONE',  ( -23.81776757772072983, -15.65134804123479917, 4.999998581000003384 ) ) ;
#20883 = CARTESIAN_POINT ( 'NONE',  ( 27.50000000000000000, -3.367667472999999580E-15, 43.60555127639999995 ) ) ;
#20884 = DIRECTION ( 'NONE',  ( 0.000000000000000000, -1.000000000000000000, 0.000000000000000000 ) ) ;
#20885 = EDGE_CURVE ( 'NONE', #7731, #27018, #19615, .T. ) ;
#20886 = DIRECTION ( 'NONE',  ( 0.000000000000000000, 0.000000000000000000, 1.000000000000000000 ) ) ;
#20887 = CARTESIAN_POINT ( 'NONE',  ( 6.992762038593867580, -16.10185592147890077, -74.73892582082525848 ) ) ;
#20888 = EDGE_CURVE ( 'NONE', #22622, #27055, #24712, .T. ) ;
#20889 = AXIS2_PLACEMENT_3D ( 'NONE', #8830, #13718, #20958 ) ;
#20890 = ORIENTED_EDGE ( 'NONE', *, *, #15081, .F. ) ;
#20891 = FACE_OUTER_BOUND ( 'NONE', #22785, .T. ) ;
#20892 = CARTESIAN_POINT ( 'NONE',  ( -27.50000000000000000, 1.776356839399999804E-15, 43.60555127550000520 ) ) ;
#20893 = CARTESIAN_POINT ( 'NONE',  ( 18.31087175629999919, 19.88197256460000162, 229.9783849850000195 ) ) ;
#20894 = CARTESIAN_POINT ( 'NONE',  ( -2.700260886555499340, 2.323010950798258811, 230.8013441257832028 ) ) ;
#20895 = CARTESIAN_POINT ( 'NONE',  ( 8.700000000134913591, -66.94093258036980387, -17.28188441695247235 ) ) ;
#20896 = CARTESIAN_POINT ( 'NONE',  ( 0.000000000000000000, -130.0000000000000000, -43.39999999999999858 ) ) ;
#20897 = CARTESIAN_POINT ( 'NONE',  ( 23.81866167241657806, 14.33570040768432996, 3.899998581000013509 ) ) ;
#20898 = CYLINDRICAL_SURFACE ( 'NONE', #18120, 3.200000000000001510 ) ;
#20899 = CARTESIAN_POINT ( 'NONE',  ( 1.728540313474559387, 5.648005006634932990, -51.46125421262499344 ) ) ;
#20900 = CARTESIAN_POINT ( 'NONE',  ( -23.34643930348873653, -14.53345043297602679, 5.642510478632145166 ) ) ;
#20901 = CARTESIAN_POINT ( 'NONE',  ( 14.77560465009611335, -28.51899377725004925, -33.29642281725517705 ) ) ;
#20902 = CARTESIAN_POINT ( 'NONE',  ( -1.861312627829580402, -20.50181238059027677, -27.47976714800043041 ) ) ;
#20903 = LINE ( 'NONE', #11457, #16766 ) ;
#20904 = ORIENTED_EDGE ( 'NONE', *, *, #31079, .F. ) ;
#20905 = CARTESIAN_POINT ( 'NONE',  ( -24.55841378230000061, -14.46270012129999927, 223.9201349020000009 ) ) ;
#20906 = ORIENTED_EDGE ( 'NONE', *, *, #15047, .T. ) ;
#20907 = CARTESIAN_POINT ( 'NONE',  ( -0.9891938378274525157, -4.753657830815115837, -52.92706695232499925 ) ) ;
#20908 = ORIENTED_EDGE ( 'NONE', *, *, #29648, .F. ) ;
#20909 = EDGE_CURVE ( 'NONE', #24098, #22030, #20391, .T. ) ;
#20910 = APPLICATION_PROTOCOL_DEFINITION ( 'draft international standard', 'automotive_design', 1998, #6356 ) ;
#20911 = ORIENTED_EDGE ( 'NONE', *, *, #11074, .F. ) ;
#20912 = DIRECTION ( 'NONE',  ( 0.000000000000000000, 0.000000000000000000, -1.000000000000000000 ) ) ;
#20913 = ORIENTED_EDGE ( 'NONE', *, *, #2907, .T. ) ;
#20914 = DIRECTION ( 'NONE',  ( 7.764622278472185525E-13, 0.9341647027306024809, 0.3568421334038978099 ) ) ;
#20915 = PLANE ( 'NONE',  #6437 ) ;
#20916 = DIRECTION ( 'NONE',  ( 1.000000000000000000, 0.000000000000000000, 0.000000000000000000 ) ) ;
#20917 = DIRECTION ( 'NONE',  ( 1.000000000000000000, 0.000000000000000000, 0.000000000000000000 ) ) ;
#20918 = CARTESIAN_POINT ( 'NONE',  ( -3.950471790850672793, -3.522405822398885888, -0.6999999999999992895 ) ) ;
#20919 = CARTESIAN_POINT ( 'NONE',  ( 5.530149664617865390, 2.595584118083901881, -1.879170051700004951 ) ) ;
#20920 = CARTESIAN_POINT ( 'NONE',  ( -14.09657507470000226, -28.30410041510000241, 229.0000000000000000 ) ) ;
#20921 = ORIENTED_EDGE ( 'NONE', *, *, #25979, .F. ) ;
#20922 = DIRECTION ( 'NONE',  ( 0.000000000000000000, 0.000000000000000000, 1.000000000000000000 ) ) ;
#20923 = CARTESIAN_POINT ( 'NONE',  ( -5.853056545089267537, 1.703994407032248581, -16.30443125759999745 ) ) ;
#20924 = CARTESIAN_POINT ( 'NONE',  ( -0.4593365651765490831, 6.553622599173768215, -34.89518930509999706 ) ) ;
#20925 = CARTESIAN_POINT ( 'NONE',  ( -0.9876156946213142662, -26.78228253924901026, 5.491373163700855820 ) ) ;
#20926 = CARTESIAN_POINT ( 'NONE',  ( 0.03443198227100000008, -27.80021999669999744, 223.9000014189999774 ) ) ;
#20927 = CARTESIAN_POINT ( 'NONE',  ( -10.49401243977554188, -26.66603606335209875, 8.000000000000007105 ) ) ;
#20928 = CARTESIAN_POINT ( 'NONE',  ( -2.567750454434825080, 2.552195388715847724, 227.7157682482517771 ) ) ;
#20929 = CARTESIAN_POINT ( 'NONE',  ( -14.89999999913999851, -27.00000000059169736, -22.62649730796000114 ) ) ;
#20930 = CARTESIAN_POINT ( 'NONE',  ( -23.73988890810277752, -12.43614388128984594, 4.854121447335470130 ) ) ;
#20931 = CARTESIAN_POINT ( 'NONE',  ( -0.4846640835643744039, -27.79604706135699033, 4.493528488000025689 ) ) ;
#20932 = EDGE_CURVE ( 'NONE', #19872, #19818, #8596, .T. ) ;
#20933 = DIRECTION ( 'NONE',  ( 0.000000000000000000, 0.000000000000000000, -1.000000000000000000 ) ) ;
#20934 = ORIENTED_EDGE ( 'NONE', *, *, #15759, .T. ) ;
#20935 = PLANE ( 'NONE',  #9817 ) ;
#20936 = CARTESIAN_POINT ( 'NONE',  ( 0.000000000000000000, 0.000000000000000000, -85.94068374632500706 ) ) ;
#20937 = CARTESIAN_POINT ( 'NONE',  ( -0.6108973618901316627, -5.182830691052390470, -0.7000282472846792725 ) ) ;
#20938 = ORIENTED_EDGE ( 'NONE', *, *, #567, .F. ) ;
#20939 = CARTESIAN_POINT ( 'NONE',  ( -10.00000000021934099, -128.8192055956760953, -36.36585972233515918 ) ) ;
#20940 = ORIENTED_EDGE ( 'NONE', *, *, #7167, .F. ) ;
#20941 = ADVANCED_FACE ( 'NONE', ( #1103, #5510, #22361, #22514 ), #5162, .F. ) ;
#20942 = ORIENTED_EDGE ( 'NONE', *, *, #17326, .T. ) ;
#20943 = ORIENTED_EDGE ( 'NONE', *, *, #20981, .F. ) ;
#20944 = FACE_BOUND ( 'NONE', #2587, .T. ) ;
#20945 = ORIENTED_EDGE ( 'NONE', *, *, #9626, .F. ) ;
#20946 = LINE ( 'NONE', #1446, #17069 ) ;
#20947 = CARTESIAN_POINT ( 'NONE',  ( 23.29312071241426096, 15.17488100587054767, 4.493007569000006640 ) ) ;
#20948 = LINE ( 'NONE', #18895, #30052 ) ;
#20949 = CARTESIAN_POINT ( 'NONE',  ( -10.00000000030000002, -28.14046567939999832, -25.54455802970000278 ) ) ;
#20950 = CARTESIAN_POINT ( 'NONE',  ( -0.1501630637024684578, -28.50011693320769623, 4.099092748999999536 ) ) ;
#20951 = CARTESIAN_POINT ( 'NONE',  ( 14.74301764161975825, -21.99999999999999289, -27.03153114797974865 ) ) ;
#20952 = CARTESIAN_POINT ( 'NONE',  ( -8.699999999648149185, -16.34590724145236251, -38.02265883393443602 ) ) ;
#20953 = CARTESIAN_POINT ( 'NONE',  ( 17.16657240419154462, 10.99999999996915179, -0.6999999999999784173 ) ) ;
#20954 = EDGE_CURVE ( 'NONE', #24391, #22821, #11132, .T. ) ;
#20955 = EDGE_LOOP ( 'NONE', ( #8774, #11628, #24008, #30434 ) ) ;
#20956 = CARTESIAN_POINT ( 'NONE',  ( -1.814319851916122772, 5.833166587536846137, -5.374955258299999983 ) ) ;
#20957 = CARTESIAN_POINT ( 'NONE',  ( 0.09521150875770739708, -4.665041947735808492, -24.41888333260000365 ) ) ;
#20958 = DIRECTION ( 'NONE',  ( -1.000000000000000000, 0.000000000000000000, 0.000000000000000000 ) ) ;
#20959 = PRODUCT ( 'Plunger Rod', 'Plunger Rod', '', ( #28523 ) ) ;
#20960 = CARTESIAN_POINT ( 'NONE',  ( 23.53911279562209202, -12.81252279912947323, 225.8816713824184035 ) ) ;
#20961 = CARTESIAN_POINT ( 'NONE',  ( 0.8681810495354941315, 3.499839992690838120, 227.7073827799873982 ) ) ;
#20962 = CARTESIAN_POINT ( 'NONE',  ( 23.20948082139999968, -13.40000000000000036, 3.900000000369999942 ) ) ;
#20963 = CARTESIAN_POINT ( 'NONE',  ( 8.999999999770000869, 20.99999999959999997, -44.96700259529604438 ) ) ;
#20964 = DIRECTION ( 'NONE',  ( 0.1090476345695682997, 0.6986477033489653099, 0.7071067811865462405 ) ) ;
#20965 = PLANE ( 'NONE',  #13233 ) ;
#20966 = DIRECTION ( 'NONE',  ( 0.000000000000000000, 0.000000000000000000, 1.000000000000000000 ) ) ;
#20967 = VERTEX_POINT ( 'NONE', #27679 ) ;
#20968 = CARTESIAN_POINT ( 'NONE',  ( 4.009291712408949770, -2.091746824018178685, -61.31790713612500099 ) ) ;
#20969 = MECHANICAL_DESIGN_GEOMETRIC_PRESENTATION_REPRESENTATION (  '', ( #19464 ), #5878 ) ;
#20970 = CARTESIAN_POINT ( 'NONE',  ( -23.81776757771349295, -15.65134804123035828, 5.147520325772222627 ) ) ;
#20971 = ORIENTED_EDGE ( 'NONE', *, *, #3987, .T. ) ;
#20972 = VERTEX_POINT ( 'NONE', #20605 ) ;
#20973 = LINE ( 'NONE', #19228, #17767 ) ;
#20974 = CARTESIAN_POINT ( 'NONE',  ( 2.193772516446764076, 5.694542648089183423, -26.09462237480000724 ) ) ;
#20975 = ORIENTED_EDGE ( 'NONE', *, *, #5405, .F. ) ;
#20976 = CARTESIAN_POINT ( 'NONE',  ( 22.97726876109999949, 16.89265187250000011, 222.9999999789999947 ) ) ;
#20977 = EDGE_CURVE ( 'NONE', #28677, #15618, #27998, .T. ) ;
#20978 = DIRECTION ( 'NONE',  ( 0.000000000000000000, -0.3420201433259318358, 0.9396926207858125046 ) ) ;
#20979 = EDGE_LOOP ( 'NONE', ( #22790, #21337, #24823, #28210 ) ) ;
#20980 = ORIENTED_EDGE ( 'NONE', *, *, #21723, .T. ) ;
#20981 = EDGE_CURVE ( 'NONE', #27055, #23754, #14143, .T. ) ;
#20982 = ORIENTED_EDGE ( 'NONE', *, *, #19593, .F. ) ;
#20983 = DIRECTION ( 'NONE',  ( -1.000000000000000000, 5.665498452320000818E-16, 0.000000000000000000 ) ) ;
#20984 = B_SPLINE_SURFACE_WITH_KNOTS ( 'NONE', 5, 1, ( 
 ( #24127, #2566 ),
 ( #17034, #12153 ),
 ( #21764, #26787 ),
 ( #9804, #214 ),
 ( #19403, #534 ),
 ( #5228, #5077 ),
 ( #14845, #24436 ),
 ( #2870, #12462 ),
 ( #10116, #19716 ),
 ( #29296, #3325 ),
 ( #27100, #3023 ),
 ( #10271, #13226 ),
 ( #10720, #17493 ),
 ( #29611, #1129 ),
 ( #12777, #8043 ) ),
 .UNSPECIFIED., .F., .F., .F.,
 ( 6, 3, 3, 3, 6 ),
 ( 2, 2 ),
 ( 0.000000000000000000, 0.5239049113010000314, 1.047809822600000107, 1.571714733900000160, 1.746349704340000031 ),
 ( -0.7000000000009999335, 2.557520719980000135E-06 ),
 .UNSPECIFIED. ) ;
#20985 = EDGE_LOOP ( 'NONE', ( #22908, #23935, #823, #199 ) ) ;
#20986 = CARTESIAN_POINT ( 'NONE',  ( -12.30000000038183039, -30.11671256533862007, -29.23759322996053100 ) ) ;
#20987 = DIRECTION ( 'NONE',  ( -1.000000000000000000, 0.000000000000000000, 0.000000000000000000 ) ) ;
#20988 = CARTESIAN_POINT ( 'NONE',  ( 5.807653394784360934, -2.603268055249425394, -66.79841551502499897 ) ) ;
#20989 = CARTESIAN_POINT ( 'NONE',  ( -24.41841039498785193, -14.69667350221323865, 3.899998581000013509 ) ) ;
#20990 = VECTOR ( 'NONE', #25644, 1000.000000000000000 ) ;
#20991 = TOROIDAL_SURFACE ( 'NONE', #26511, 24.50000000000000000, 4.000000000000000000 ) ;
#20992 = FACE_OUTER_BOUND ( 'NONE', #19902, .T. ) ;
#20993 = FACE_OUTER_BOUND ( 'NONE', #20197, .T. ) ;
#20994 = EDGE_CURVE ( 'NONE', #974, #22866, #7623, .T. ) ;
#20995 = CARTESIAN_POINT ( 'NONE',  ( -17.43796590507927746, -23.65055572458717492, -24.56029040692275345 ) ) ;
#20996 = ORIENTED_EDGE ( 'NONE', *, *, #5968, .F. ) ;
#20997 = CARTESIAN_POINT ( 'NONE',  ( -19.42125183333303795, 20.00000466481577988, -0.3145118510766364284 ) ) ;
#20998 = CARTESIAN_POINT ( 'NONE',  ( -1.657635364023947400, -6.345118362804027079, -12.55022317840000312 ) ) ;
#20999 = DIRECTION ( 'NONE',  ( -1.000000000000000000, 5.665498452320000818E-16, 0.000000000000000000 ) ) ;
#21000 = ADVANCED_FACE ( 'NONE', ( #4087 ), #17223, .F. ) ;
#21001 = CARTESIAN_POINT ( 'NONE',  ( -10.69999999895494192, -23.79999999999999716, -28.40000000000000213 ) ) ;
#21002 = VERTEX_POINT ( 'NONE', #21086 ) ;
#21003 = DIRECTION ( 'NONE',  ( 0.9831920802501790124, 0.1715636151751586680, 0.06244404920691486172 ) ) ;
#21004 = CARTESIAN_POINT ( 'NONE',  ( -10.69999999999999929, -129.1531271268999888, -37.03846033197000054 ) ) ;
#21005 = CARTESIAN_POINT ( 'NONE',  ( 17.93011078763067090, 11.79183908526299085, -0.6999999999999784173 ) ) ;
#21006 = VECTOR ( 'NONE', #26101, 1000.000000000000000 ) ;
#21007 = CARTESIAN_POINT ( 'NONE',  ( 1.647792172260419852, -20.50181238077959733, -27.47976714835313317 ) ) ;
#21008 = EDGE_CURVE ( 'NONE', #24996, #15092, #14387, .T. ) ;
#21009 = CARTESIAN_POINT ( 'NONE',  ( 11.66358246589999936, -24.14124255329999968, -1.399999999999998579 ) ) ;
#21010 = CARTESIAN_POINT ( 'NONE',  ( -1.909971040720825908, -5.612411004515823088, -46.99520033292500187 ) ) ;
#21011 = AXIS2_PLACEMENT_3D ( 'NONE', #22419, #10604, #5871 ) ;
#21012 = CARTESIAN_POINT ( 'NONE',  ( 26.94142135619999934, 4.549494481000000867, 230.0000000000000000 ) ) ;
#21013 = CARTESIAN_POINT ( 'NONE',  ( 16.27441336913832615, 11.65945330722155759, -0.6999999999999783062 ) ) ;
#21014 = VERTEX_POINT ( 'NONE', #17121 ) ;
#21015 = SURFACE_STYLE_FILL_AREA ( #25583 ) ;
#21016 = CARTESIAN_POINT ( 'NONE',  ( -8.999999999699999975, 21.69999999929999390, -51.10000000000999876 ) ) ;
#21017 = CARTESIAN_POINT ( 'NONE',  ( 2.729399839092999436, -3.446420600438925508, -68.10000000002500542 ) ) ;
#21019 = EDGE_CURVE ( 'NONE', #29115, #28085, #2201, .T. ) ;
#21018 = VECTOR ( 'NONE', #24289, 1000.000000000000114 ) ;
#21020 = CARTESIAN_POINT ( 'NONE',  ( 2.664535259099999805E-15, 2.694277338339796213, -67.89769279494430521 ) ) ;
#21021 = CARTESIAN_POINT ( 'NONE',  ( -4.201749689532753962, 0.5185635314718879396, -44.10000000002499831 ) ) ;
#21022 = EDGE_CURVE ( 'NONE', #14059, #2111, #2356, .T. ) ;
#21023 = ORIENTED_EDGE ( 'NONE', *, *, #18680, .T. ) ;
#21024 = FACE_OUTER_BOUND ( 'NONE', #21562, .T. ) ;
#21025 = CARTESIAN_POINT ( 'NONE',  ( -3.807105672873282831, -5.136256491778199873, -65.13409070562501313 ) ) ;
#21026 = ORIENTED_EDGE ( 'NONE', *, *, #15468, .F. ) ;
#21027 = ADVANCED_FACE ( 'NONE', ( #7671 ), #28624, .T. ) ;
#21028 = CARTESIAN_POINT ( 'NONE',  ( 24.71263212711717117, -12.73382341766860293, 4.267021104580390300 ) ) ;
#21029 = VECTOR ( 'NONE', #954, 1000.000000000000000 ) ;
#21030 = B_SPLINE_CURVE_WITH_KNOTS ( 'NONE', 3,
 ( #9118, #28319, #19191, #21406, #9272, #21244, #6606, #23770 ),
 .UNSPECIFIED., .F., .F.,
 ( 4, 2, 2, 4 ),
 ( 0.000000000000000000, 0.2500000000000000555, 0.5000000000000001110, 1.000000000000000000 ),
 .UNSPECIFIED. ) ;
#21031 = CARTESIAN_POINT ( 'NONE',  ( -26.80856362799623582, -7.546808677664434306, 0.000000000000000000 ) ) ;
#21032 = EDGE_LOOP ( 'NONE', ( #20131, #29717, #19822, #3621, #857 ) ) ;
#21033 = CARTESIAN_POINT ( 'NONE',  ( 9.738910687886868089, -24.96785170200598358, 115.0000000000000000 ) ) ;
#21034 = DIRECTION ( 'NONE',  ( -1.000000000000000000, -6.565028073413479156E-24, -2.257144471327815248E-12 ) ) ;
#21035 = CARTESIAN_POINT ( 'NONE',  ( 9.867241297310000547, 19.99999999999999645, -42.91081254286000046 ) ) ;
#21036 = CARTESIAN_POINT ( 'NONE',  ( -3.257018533420682704, -1.358678418916599018, 230.8224594091674930 ) ) ;
#21037 = UNCERTAINTY_MEASURE_WITH_UNIT (LENGTH_MEASURE( 1.000000000000000082E-05 ), #11774, 'distance_accuracy_value', 'NONE');
#21038 = CARTESIAN_POINT ( 'NONE',  ( -0.1464386043128553250, -27.80011885101413682, 4.099092748999999536 ) ) ;
#21039 = CIRCLE ( 'NONE', #25049, 4.000000004070001225 ) ;
#21040 = CARTESIAN_POINT ( 'NONE',  ( -7.861312627709999390, 2.450513428968473129, -42.01217025057427179 ) ) ;
#21041 = CARTESIAN_POINT ( 'NONE',  ( 16.40303402077768169, -9.791839085275103827, -0.6999999999999784173 ) ) ;
#21042 = EDGE_LOOP ( 'NONE', ( #2259, #22492, #19083, #30269 ) ) ;
#21043 = FACE_OUTER_BOUND ( 'NONE', #9154, .T. ) ;
#21044 = CARTESIAN_POINT ( 'NONE',  ( 9.993285220779506872, -25.61999708228222872, 43.60555127639999995 ) ) ;
#21045 = CARTESIAN_POINT ( 'NONE',  ( 3.441895575009999764, 11.73074918480000051, 232.6627643349999914 ) ) ;
#21046 = CARTESIAN_POINT ( 'NONE',  ( -2.687036963334896278, -2.345727656357492918, 230.7977248921665137 ) ) ;
#21047 = CYLINDRICAL_SURFACE ( 'NONE', #27226, 2.000000000000003553 ) ;
#21048 = CARTESIAN_POINT ( 'NONE',  ( 0.1368966849300000121, -12.12573834550000029, 230.6412452697800006 ) ) ;
#21049 = CARTESIAN_POINT ( 'NONE',  ( -0.8805184773353784689, -27.48609199508887002, 225.6749683491974565 ) ) ;
#21050 = CARTESIAN_POINT ( 'NONE',  ( 26.79556473285982321, 0.4875557887249620803, 0.000000000000000000 ) ) ;
#21051 = CARTESIAN_POINT ( 'NONE',  ( 1.592968524163114852, 5.205024221813498109, -50.66125421252500161 ) ) ;
#21052 = CIRCLE ( 'NONE', #19019, 3.200000004570001888 ) ;
#21053 = CARTESIAN_POINT ( 'NONE',  ( 27.79539923781684507, 0.5057481689249188062, 0.8585786439999909536 ) ) ;
#21054 = CARTESIAN_POINT ( 'NONE',  ( -7.494278858881251892, -6.635700603326244007, -34.24272173891409210 ) ) ;
#21055 = CARTESIAN_POINT ( 'NONE',  ( 10.69999999999999929, -24.87867965640000278, -30.52132034359999935 ) ) ;
#21056 = EDGE_CURVE ( 'NONE', #12853, #4792, #20000, .T. ) ;
#21057 = CARTESIAN_POINT ( 'NONE',  ( -24.25955693044071637, -12.95188430987226802, 224.3574895194784347 ) ) ;
#21058 = EDGE_CURVE ( 'NONE', #11115, #10219, #7109, .T. ) ;
#21059 = ADVANCED_FACE ( 'NONE', ( #14154, #9417 ), #21548, .F. ) ;
#21060 = FACE_OUTER_BOUND ( 'NONE', #1241, .T. ) ;
#21061 = TOROIDAL_SURFACE ( 'NONE', #20040, 24.50000000000000000, 3.200000000000000178 ) ;
#21062 = EDGE_CURVE ( 'NONE', #25858, #5609, #15144, .T. ) ;
#21063 = ORIENTED_EDGE ( 'NONE', *, *, #26420, .T. ) ;
#21064 = CARTESIAN_POINT ( 'NONE',  ( 4.390418465362644795, -3.559810858784186127, -55.40923804942499942 ) ) ;
#21065 = EDGE_LOOP ( 'NONE', ( #25277, #365, #17537, #21250 ) ) ;
#21066 = CONTEXT_DEPENDENT_SHAPE_REPRESENTATION ( #7184, #29506 ) ;
#21067 = ORIENTED_EDGE ( 'NONE', *, *, #11511, .T. ) ;
#21068 = DIRECTION ( 'NONE',  ( 0.000000000000000000, -1.000000000000000000, 0.000000000000000000 ) ) ;
#21069 = ORIENTED_EDGE ( 'NONE', *, *, #2318, .T. ) ;
#21070 = CARTESIAN_POINT ( 'NONE',  ( 8.881784197000000993E-16, -2.220446049249999755E-16, 230.8412452700000017 ) ) ;
#21071 = CARTESIAN_POINT ( 'NONE',  ( 1.065814103639999922E-14, 0.000000000000000000, 38.33953982530000104 ) ) ;
#21072 = CARTESIAN_POINT ( 'NONE',  ( -17.37283180966073459, -28.23568901534668285, -23.33992269394541452 ) ) ;
#21073 = AXIS2_PLACEMENT_3D ( 'NONE', #25611, #21189, #13957 ) ;
#21074 = DIRECTION ( 'NONE',  ( 0.000000000000000000, 0.000000000000000000, 1.000000000000000000 ) ) ;
#21075 = CARTESIAN_POINT ( 'NONE',  ( -4.276011752261355880, -103.0613381315345123, 16.56805218637121513 ) ) ;
#21076 = CARTESIAN_POINT ( 'NONE',  ( -17.40480267186241292, 11.95092772882062704, -4.336808689942017243E-16 ) ) ;
#21077 = CARTESIAN_POINT ( 'NONE',  ( -4.325159770583737462, -1.744232581393518444, -0.9971974345000036433 ) ) ;
#21078 = CARTESIAN_POINT ( 'NONE',  ( 5.086809642800000475, -29.99929454970000009, 230.6999999999999886 ) ) ;
#21079 = ORIENTED_EDGE ( 'NONE', *, *, #28189, .T. ) ;
#21080 = CARTESIAN_POINT ( 'NONE',  ( -17.93324555120827668, 10.97998838178171432, -0.6999999989999727834 ) ) ;
#21081 = CARTESIAN_POINT ( 'NONE',  ( 3.256742448429973624, 4.730705660258329281, -17.81259163650000232 ) ) ;
#21082 = CARTESIAN_POINT ( 'NONE',  ( 6.568447637800200134, 5.835222101079285295, -40.32519715133864935 ) ) ;
#21083 = CIRCLE ( 'NONE', #4503, 2.000000000000000000 ) ;
#21084 = CIRCLE ( 'NONE', #29608, 3.000000000000001332 ) ;
#21085 = CARTESIAN_POINT ( 'NONE',  ( -8.000000000444114079, -28.22468611108740788, -31.13863906519029001 ) ) ;
#21086 = CARTESIAN_POINT ( 'NONE',  ( -7.999999999985950794, -116.8591659214701792, 11.34031266722930908 ) ) ;
#21087 = CARTESIAN_POINT ( 'NONE',  ( -18.81428968775364652, -21.61535361001210731, 8.000000000000007105 ) ) ;
#21088 = DIRECTION ( 'NONE',  ( -0.8660254037843289066, -0.5000000000001899592, 0.000000000000000000 ) ) ;
#21089 = CARTESIAN_POINT ( 'NONE',  ( 27.31421068595970780, 9.888053941072412201, 0.5017677510000262409 ) ) ;
#21090 = CARTESIAN_POINT ( 'NONE',  ( -3.528956123591135086, 0.08598667200548251732, 226.6412452697750552 ) ) ;
#21091 = CARTESIAN_POINT ( 'NONE',  ( -0.3682501489830092845, -27.79783598715961901, 4.319846982000025370 ) ) ;
#21092 = CARTESIAN_POINT ( 'NONE',  ( -2.128136350289183021, -3.759461034538412516, -70.24666146241560227 ) ) ;
#21093 = ORIENTED_EDGE ( 'NONE', *, *, #12701, .F. ) ;
#21094 = CARTESIAN_POINT ( 'NONE',  ( 23.55411374389282386, 16.04538543799059980, 8.000000000000007105 ) ) ;
#21095 = SURFACE_STYLE_FILL_AREA ( #12378 ) ;
#21096 = B_SPLINE_CURVE_WITH_KNOTS ( 'NONE', 5,
 ( #2009, #21197, #9075, #21048, #30648, #11599, #18670, #11448, #30795, #21356, #28432, #18519, #28121, #18829, #7183, #6866, #28272, #16159, #16316, #8918, #9378 ),
 .UNSPECIFIED., .F., .F.,
 ( 6, 3, 3, 3, 3, 3, 6 ),
 ( 0.000000000000000000, 8.467772783080000920, 16.93507402329999678, 25.40292880620000204, 33.87083985430000155, 42.33863182420000015, 46.94504270979999916 ),
 .UNSPECIFIED. ) ;
#21097 = CARTESIAN_POINT ( 'NONE',  ( 0.9242227292564770824, -26.78436817533707526, 4.402069900664497659 ) ) ;
#21098 = VERTEX_POINT ( 'NONE', #470 ) ;
#21099 = CARTESIAN_POINT ( 'NONE',  ( -4.592700181227121980, -1.655560342997616896, -44.41497819512500200 ) ) ;
#21100 = ORIENTED_EDGE ( 'NONE', *, *, #15252, .F. ) ;
#21101 = ORIENTED_EDGE ( 'NONE', *, *, #23441, .F. ) ;
#21102 = CIRCLE ( 'NONE', #25113, 1.099999999570000497 ) ;
#21103 = VERTEX_POINT ( 'NONE', #19024 ) ;
#21104 = CARTESIAN_POINT ( 'NONE',  ( -1.115050571030000048, -28.47845913019999742, 224.7918862260000026 ) ) ;
#21105 = ORIENTED_EDGE ( 'NONE', *, *, #25496, .T. ) ;
#21106 = CARTESIAN_POINT ( 'NONE',  ( -24.91946588839999777, -13.83134141909999926, 226.0028092389999870 ) ) ;
#21107 = DIRECTION ( 'NONE',  ( 1.000000000000000000, 0.000000000000000000, 0.000000000000000000 ) ) ;
#21108 = LINE ( 'NONE', #30703, #28033 ) ;
#21109 = CARTESIAN_POINT ( 'NONE',  ( 2.105781777274182698, 3.334946656835463319, -35.69999999999999574 ) ) ;
#21110 = CARTESIAN_POINT ( 'NONE',  ( 2.414417451572403728, -4.362164995236931908, -94.44574089077143242 ) ) ;
#21111 = CARTESIAN_POINT ( 'NONE',  ( 26.43121445407034287, -4.566620399128002994, -1.399999999999998579 ) ) ;
#21112 = CARTESIAN_POINT ( 'NONE',  ( 3.224831307069992992, -1.414428330319838389, 227.6554536018044814 ) ) ;
#21113 = CARTESIAN_POINT ( 'NONE',  ( -10.99999999969999998, 20.99999999999999645, -58.51619611000000276 ) ) ;
#21114 = EDGE_CURVE ( 'NONE', #30998, #19325, #28245, .T. ) ;
#21115 = ORIENTED_EDGE ( 'NONE', *, *, #15759, .F. ) ;
#21116 = CARTESIAN_POINT ( 'NONE',  ( -0.7873752056533391830, -4.273814420472604070, -4.025234013000003053 ) ) ;
#21117 = CARTESIAN_POINT ( 'NONE',  ( 4.692682656939434871, -1.014318600726540787, -22.85286215650000585 ) ) ;
#21118 = CARTESIAN_POINT ( 'NONE',  ( -1.110223024630000146E-16, 0.000000000000000000, -44.10000000000000142 ) ) ;
#21119 = LINE ( 'NONE', #25691, #3628 ) ;
#21120 = DIRECTION ( 'NONE',  ( -1.000000000000000000, 0.000000000000000000, 0.000000000000000000 ) ) ;
#21121 = DIRECTION ( 'NONE',  ( -0.000000000000000000, 0.000000000000000000, 1.000000000000000000 ) ) ;
#21122 = CARTESIAN_POINT ( 'NONE',  ( -26.80000000069999899, 3.281945028329999726E-15, 18.39142920540000148 ) ) ;
#21123 = EDGE_CURVE ( 'NONE', #22430, #7318, #1588, .T. ) ;
#21124 = CIRCLE ( 'NONE', #7546, 4.439999999480002124 ) ;
#21125 = CARTESIAN_POINT ( 'NONE',  ( -27.50000000000000000, 3.367667473009999970E-15, 65.00000000000000000 ) ) ;
#21126 = CARTESIAN_POINT ( 'NONE',  ( 1.568292632109252738, -27.75603058367127574, 5.310199493000017590 ) ) ;
#21127 = CARTESIAN_POINT ( 'NONE',  ( 10.69999999989999928, -25.00000000000000000, -16.71944709739999979 ) ) ;
#21128 = ORIENTED_EDGE ( 'NONE', *, *, #13338, .F. ) ;
#21129 = CARTESIAN_POINT ( 'NONE',  ( -1.078772944755383767, 5.890544393200768170, -60.25324387862499975 ) ) ;
#21130 = CARTESIAN_POINT ( 'NONE',  ( -27.09307779329999732, 4.568309977820000256, 229.9751247039999953 ) ) ;
#21131 = VERTEX_POINT ( 'NONE', #7064 ) ;
#21132 = DIRECTION ( 'NONE',  ( 0.3633921898465292122, 0.9316362575375348731, -6.938893903907226800E-15 ) ) ;
#21133 = CARTESIAN_POINT ( 'NONE',  ( 3.241815827827634777, 4.728971459636320596, -35.21970670789999502 ) ) ;
#21134 = ORIENTED_EDGE ( 'NONE', *, *, #10373, .T. ) ;
#21135 = CYLINDRICAL_SURFACE ( 'NONE', #22378, 1.000000000000001332 ) ;
#21136 = PLANE ( 'NONE',  #20319 ) ;
#21137 = VERTEX_POINT ( 'NONE', #5244 ) ;
#21138 = ORIENTED_EDGE ( 'NONE', *, *, #20954, .F. ) ;
#21139 = ORIENTED_EDGE ( 'NONE', *, *, #22690, .T. ) ;
#21140 = VERTEX_POINT ( 'NONE', #26426 ) ;
#21141 = CARTESIAN_POINT ( 'NONE',  ( -12.29999999970000069, -23.80000000074999988, -28.40000000001083791 ) ) ;
#21142 = EDGE_CURVE ( 'NONE', #2860, #1244, #18668, .T. ) ;
#21143 = CARTESIAN_POINT ( 'NONE',  ( -16.81341597756113515, 9.900182044522454206, -0.6999999989999727834 ) ) ;
#21144 = CARTESIAN_POINT ( 'NONE',  ( 3.542472921321142110, 4.818407451951889797, -66.16226422552499287 ) ) ;
#21145 = CARTESIAN_POINT ( 'NONE',  ( 20.23761873489999985, -20.36716332730000190, 229.9172016509999992 ) ) ;
#21146 = CARTESIAN_POINT ( 'NONE',  ( 6.792853103711780527, -7.106081641748739131, -34.01330157743200289 ) ) ;
#21147 = CARTESIAN_POINT ( 'NONE',  ( 3.916247328310000331, -28.49226594579999983, 222.0000000000000000 ) ) ;
#21148 = CARTESIAN_POINT ( 'NONE',  ( 1.896306263639558010, -4.736092137553404413, -0.7000633247167794559 ) ) ;
#21149 = ORIENTED_EDGE ( 'NONE', *, *, #255, .T. ) ;
#21150 = CARTESIAN_POINT ( 'NONE',  ( -17.83928249649999742, 19.99999999999999645, -1.399999999999998579 ) ) ;
#21151 = AXIS2_PLACEMENT_3D ( 'NONE', #8567, #6378, #15824 ) ;
#21152 = CARTESIAN_POINT ( 'NONE',  ( -5.517889265940039145, -2.627421812126006451, -12.37655742009999926 ) ) ;
#21153 = CARTESIAN_POINT ( 'NONE',  ( 27.92857142909999979, -3.420150602509999660E-15, 137.9396849850000137 ) ) ;
#21154 = CARTESIAN_POINT ( 'NONE',  ( -10.69999999967889615, -26.16298946189287022, -31.51701243199215341 ) ) ;
#21155 = ORIENTED_EDGE ( 'NONE', *, *, #29397, .T. ) ;
#21156 = CARTESIAN_POINT ( 'NONE',  ( -9.000000000000000000, 19.99999999999999645, -42.39999999999999858 ) ) ;
#21157 = CARTESIAN_POINT ( 'NONE',  ( 1.645560275461343203, -28.45273235261698019, 4.999998581000003384 ) ) ;
#21158 = CARTESIAN_POINT ( 'NONE',  ( -27.70209899609999837, 2.554093293449999802, 222.0000000000000000 ) ) ;
#21159 = ADVANCED_FACE ( 'NONE', ( #2962 ), #11621, .F. ) ;
#21160 = CARTESIAN_POINT ( 'NONE',  ( 8.986416953306171962, -25.99194954040538619, 23.96300465906694299 ) ) ;
#21161 = FACE_OUTER_BOUND ( 'NONE', #14597, .T. ) ;
#21162 = DIRECTION ( 'NONE',  ( 0.000000000000000000, 0.000000000000000000, -1.000000000000000000 ) ) ;
#21163 = DIRECTION ( 'NONE',  ( 0.7071067811870024311, 0.6455034179958023532, -0.2886612848220092009 ) ) ;
#21164 = DIRECTION ( 'NONE',  ( -0.000000000000000000, -0.000000000000000000, -1.000000000000000000 ) ) ;
#21165 = ORIENTED_EDGE ( 'NONE', *, *, #21170, .F. ) ;
#21166 = CARTESIAN_POINT ( 'NONE',  ( -10.69999999999999929, -24.00310551309999951, -28.69094250879999919 ) ) ;
#21167 = DIRECTION ( 'NONE',  ( -0.4999999999969509945, 0.4151946956549595336, 0.7600087925169251024 ) ) ;
#21168 = CARTESIAN_POINT ( 'NONE',  ( 2.713364190111911434, -3.841189043361406430, -68.10000000002503384 ) ) ;
#21169 = EDGE_CURVE ( 'NONE', #17667, #22455, #13989, .T. ) ;
#21170 = EDGE_CURVE ( 'NONE', #18252, #3758, #27485, .T. ) ;
#21171 = CARTESIAN_POINT ( 'NONE',  ( 2.131591336857817875, -2.813577582618851380, -0.6999999999999784173 ) ) ;
#21172 = CARTESIAN_POINT ( 'NONE',  ( 6.321956670630000552, 10.26563848810000046, 230.6412452697800006 ) ) ;
#21173 = ORIENTED_EDGE ( 'NONE', *, *, #29562, .F. ) ;
#21174 = CARTESIAN_POINT ( 'NONE',  ( 27.63177356690000153, -3.383804547719999749E-15, 37.36052363810000543 ) ) ;
#21175 = ADVANCED_BREP_SHAPE_REPRESENTATION ( '', ( #11026, #17722 ), #2272 ) ;
#21176 = CARTESIAN_POINT ( 'NONE',  ( -5.427432314178970429, 2.515719109140460041, -66.25526299442500999 ) ) ;
#21177 = ORIENTED_EDGE ( 'NONE', *, *, #17106, .F. ) ;
#21178 = CARTESIAN_POINT ( 'NONE',  ( -7.999999999638116144, -22.83323352248630655, -39.84673050082100332 ) ) ;
#21179 = EDGE_CURVE ( 'NONE', #7809, #27823, #8330, .T. ) ;
#21180 = B_SPLINE_CURVE_WITH_KNOTS ( 'NONE', 1,
 ( #1664, #20865 ),
 .UNSPECIFIED., .F., .F.,
 ( 2, 2 ),
 ( -0.7031437918980000257, 3.133915349451399379E-11 ),
 .UNSPECIFIED. ) ;
#21181 = CARTESIAN_POINT ( 'NONE',  ( 8.000000000229924524, -28.07052495763006661, -25.59750966822355522 ) ) ;
#21182 = ORIENTED_EDGE ( 'NONE', *, *, #9018, .T. ) ;
#21183 = DIRECTION ( 'NONE',  ( 0.000000000000000000, 0.5000000000001900702, -0.8660254037843290176 ) ) ;
#21184 = CARTESIAN_POINT ( 'NONE',  ( 11.20000000009999930, -24.50000000030000180, -24.06987298079999604 ) ) ;
#21185 = LINE ( 'NONE', #20718, #26061 ) ;
#21186 = CARTESIAN_POINT ( 'NONE',  ( 0.2655682516278248806, -27.79918151443105856, 3.920205022000022854 ) ) ;
#21187 = EDGE_CURVE ( 'NONE', #29481, #19467, #2342, .T. ) ;
#21188 = CARTESIAN_POINT ( 'NONE',  ( 26.93395387800000051, -3.298349105250000085E-15, 42.24324102359999955 ) ) ;
#21189 = DIRECTION ( 'NONE',  ( 4.428977494234582379E-12, 0.8987940462991651502, -0.4383711467890810676 ) ) ;
#21190 = ORIENTED_EDGE ( 'NONE', *, *, #5021, .T. ) ;
#21191 = DIRECTION ( 'NONE',  ( 0.000000000000000000, -1.000000000000000000, 0.000000000000000000 ) ) ;
#21192 = CARTESIAN_POINT ( 'NONE',  ( 1.099998580829999906, -27.77839262550000043, 225.0000014190000002 ) ) ;
#21193 = CARTESIAN_POINT ( 'NONE',  ( 18.22444678769999982, 20.00000155620000086, 230.6880676309999956 ) ) ;
#21194 = CARTESIAN_POINT ( 'NONE',  ( -15.75156552665617937, -9.231204648498994914, 0.000000000000000000 ) ) ;
#21195 = CIRCLE ( 'NONE', #30765, 27.92857142860000152 ) ;
#21196 = CARTESIAN_POINT ( 'NONE',  ( -2.846903954058784159, 11.76276068685684173, 232.0000000000052580 ) ) ;
#21197 = CARTESIAN_POINT ( 'NONE',  ( -2.247467472309999437, -11.88585404939999890, 230.6412452697800006 ) ) ;
#21198 = CIRCLE ( 'NONE', #7618, 17.84349269770000035 ) ;
#21199 = DIRECTION ( 'NONE',  ( -0.8329895880221872551, 0.5532886644841250590, 0.000000000000000000 ) ) ;
#21200 = CARTESIAN_POINT ( 'NONE',  ( 23.62906798355282589, -14.64615088352157812, 225.6773072844200101 ) ) ;
#21201 = CARTESIAN_POINT ( 'NONE',  ( 2.528196872781957705, -4.554263998399506796, -54.78172062782500973 ) ) ;
#21202 = ADVANCED_FACE ( 'NONE', ( #22776 ), #15078, .T. ) ;
#21203 = CARTESIAN_POINT ( 'NONE',  ( -20.30396346370000060, 20.00000000000000000, 228.5999999999999943 ) ) ;
#21204 = CARTESIAN_POINT ( 'NONE',  ( 18.26377084502559356, 11.16397745125027541, -4.336808689942018722E-16 ) ) ;
#21205 = CARTESIAN_POINT ( 'NONE',  ( 4.041451884329999800, 2.220446049249999755E-16, 230.5235986622430175 ) ) ;
#21206 = CARTESIAN_POINT ( 'NONE',  ( -0.9131176269203642448, -27.48533474125000708, 224.3574895203637141 ) ) ;
#21207 = CARTESIAN_POINT ( 'NONE',  ( -24.43799431780000120, -14.66523353630000059, 223.9971937000000253 ) ) ;
#21208 = CARTESIAN_POINT ( 'NONE',  ( 0.9406167415608388538, 5.909121140422558760, -54.41500058692499664 ) ) ;
#21209 = ORIENTED_EDGE ( 'NONE', *, *, #15354, .T. ) ;
#21210 = ITEM_DEFINED_TRANSFORMATION ( 'NONE', 'NONE', #25919,  #17722 ) ;
#21211 = VECTOR ( 'NONE', #29232, 1000.000000000000000 ) ;
#21212 = ORIENTED_EDGE ( 'NONE', *, *, #12614, .T. ) ;
#21213 = CARTESIAN_POINT ( 'NONE',  ( -17.49355845095107043, -29.49704728436632806, -32.73183177029086011 ) ) ;
#21214 = ORIENTED_EDGE ( 'NONE', *, *, #16820, .F. ) ;
#21215 = CARTESIAN_POINT ( 'NONE',  ( -8.699999999952064300, -113.1082736028020577, 6.336644014756059207 ) ) ;
#21216 = CARTESIAN_POINT ( 'NONE',  ( -11.00000000000000000, 25.22617105830878614, -61.82510970417090590 ) ) ;
#21217 = CARTESIAN_POINT ( 'NONE',  ( -27.79539923781684507, -0.5057481689249130330, 8.000000000000007105 ) ) ;
#21218 = MANIFOLD_SOLID_BREP ( 'PartBody', #1506 ) ;
#21219 = CARTESIAN_POINT ( 'NONE',  ( 1.065814103639999922E-14, 0.000000000000000000, 36.78285841159999592 ) ) ;
#21220 = CARTESIAN_POINT ( 'NONE',  ( 27.79539923781684507, 0.5057481689249235801, 8.000000000000007105 ) ) ;
#21221 = EDGE_CURVE ( 'NONE', #17368, #30391, #13595, .T. ) ;
#21222 = DIRECTION ( 'NONE',  ( 0.000000000000000000, 0.000000000000000000, 1.000000000000000000 ) ) ;
#21223 = CARTESIAN_POINT ( 'NONE',  ( -3.630162863991666988, -2.403661707492382060, -6.389929326000004295 ) ) ;
#21224 = CARTESIAN_POINT ( 'NONE',  ( -28.49999999959999641, -10.47094308429999998, 229.2404163060000144 ) ) ;
#21225 = ORIENTED_EDGE ( 'NONE', *, *, #8961, .F. ) ;
#21226 = CARTESIAN_POINT ( 'NONE',  ( 13.46518788483360041, 20.99999999997146105, -56.74319753100301256 ) ) ;
#21227 = EDGE_CURVE ( 'NONE', #3911, #27980, #27034, .T. ) ;
#21228 = CARTESIAN_POINT ( 'NONE',  ( 2.558869066659682723, 3.716983018758990287, -18.15009163650000090 ) ) ;
#21229 = CARTESIAN_POINT ( 'NONE',  ( -20.30403093138962234, 20.00000000003553424, 1.000000000000000888 ) ) ;
#21230 = CARTESIAN_POINT ( 'NONE',  ( -9.631068057916044367, 21.00000000000229861, -53.61809490181903470 ) ) ;
#21231 = EDGE_CURVE ( 'NONE', #6895, #23358, #6754, .T. ) ;
#21232 = VECTOR ( 'NONE', #2391, 1000.000000000000000 ) ;
#21233 = CARTESIAN_POINT ( 'NONE',  ( 28.64321111491632976, -9.935962574576189255, 0.5017677510000262409 ) ) ;
#21234 = CARTESIAN_POINT ( 'NONE',  ( -24.46845037339999962, -13.19716075180000026, 224.2397332909999932 ) ) ;
#21235 = CARTESIAN_POINT ( 'NONE',  ( 19.29387769735768998, -21.32719583073583536, 8.000000000000007105 ) ) ;
#21236 = CARTESIAN_POINT ( 'NONE',  ( 4.248246898893026646, -2.821772188863608921, -42.87875473022499762 ) ) ;
#21237 = B_SPLINE_CURVE_WITH_KNOTS ( 'NONE', 3,
 ( #2773, #10476, #12365, #20073, #29348, #29662, #19451, #19608, #7637, #26838, #5289, #23061 ),
 .UNSPECIFIED., .F., .F.,
 ( 4, 2, 2, 2, 2, 4 ),
 ( 0.000000000000000000, 0.1250000000000004163, 0.2500000000000008327, 0.5000000000000005551, 0.7500000000000002220, 1.000000000000000000 ),
 .UNSPECIFIED. ) ;
#21239 = CARTESIAN_POINT ( 'NONE',  ( 23.77307027441306531, -14.41181805765238444, 4.999998581000003384 ) ) ;
#21238 = B_SPLINE_CURVE_WITH_KNOTS ( 'NONE', 3,
 ( #17093, #30958, #4673, #21514 ),
 .UNSPECIFIED., .F., .F.,
 ( 4, 4 ),
 ( 0.000000000000000000, 1.000000000000000000 ),
 .UNSPECIFIED. ) ;
#21240 = CARTESIAN_POINT ( 'NONE',  ( -3.293366139499089851, -1.270718008849189173, 226.6412452697750268 ) ) ;
#21241 = CARTESIAN_POINT ( 'NONE',  ( 0.5057536231481327693, -27.79562098839016571, 3.899998581000013509 ) ) ;
#21242 = CARTESIAN_POINT ( 'NONE',  ( 27.50000000000000000, 1.776356839399999804E-15, 186.3944487249999895 ) ) ;
#21243 = ORIENTED_EDGE ( 'NONE', *, *, #17444, .T. ) ;
#21244 = CARTESIAN_POINT ( 'NONE',  ( 5.007332623075492428, -31.60226355569895773, -80.38061281867886976 ) ) ;
#21245 = CARTESIAN_POINT ( 'NONE',  ( -7.105427357599999217E-15, -7.105427357599999217E-15, 36.78285841159999592 ) ) ;
#21246 = PRESENTATION_STYLE_ASSIGNMENT (( #12220 ) ) ;
#21247 = DIRECTION ( 'NONE',  ( 1.000000000000000000, 0.000000000000000000, 0.000000000000000000 ) ) ;
#21248 = ORIENTED_EDGE ( 'NONE', *, *, #2727, .F. ) ;
#21249 = CARTESIAN_POINT ( 'NONE',  ( 0.6626488065253229864, -5.424947836095445730, -44.58057807742500955 ) ) ;
#21250 = ORIENTED_EDGE ( 'NONE', *, *, #9442, .F. ) ;
#21251 = EDGE_LOOP ( 'NONE', ( #3280, #7769, #29936, #2827 ) ) ;
#21252 = CARTESIAN_POINT ( 'NONE',  ( 0.000000000000000000, 0.000000000000000000, 0.000000000000000000 ) ) ;
#21253 = EDGE_LOOP ( 'NONE', ( #13823, #1274, #19071, #2027 ) ) ;
#21254 = CARTESIAN_POINT ( 'NONE',  ( -16.91615862483482857, -10.10168739744133859, 0.000000000000000000 ) ) ;
#21255 = EDGE_LOOP ( 'NONE', ( #17440, #307, #29616, #12824 ) ) ;
#21256 = VECTOR ( 'NONE', #26391, 1000.000000000000114 ) ;
#21257 = CARTESIAN_POINT ( 'NONE',  ( 10.69999999997255991, -29.39962415735867296, -30.24292916419924993 ) ) ;
#21258 = CARTESIAN_POINT ( 'NONE',  ( 23.83861932470720291, 15.61961844235199948, 4.689445052000001724 ) ) ;
#21259 = FACE_OUTER_BOUND ( 'NONE', #27208, .T. ) ;
#21260 = CARTESIAN_POINT ( 'NONE',  ( -1.484924240490000047, -1.484924240490000047, 227.6412452697800006 ) ) ;
#21261 = CARTESIAN_POINT ( 'NONE',  ( 18.15446590459846377, 19.99997493598501208, -0.6870078918781518107 ) ) ;
#21262 = CARTESIAN_POINT ( 'NONE',  ( 20.39644572738137285, -17.41965902382794695, -1.399999999999998579 ) ) ;
#21263 = CARTESIAN_POINT ( 'NONE',  ( -22.65536398236773508, -14.31703479018443304, 5.288095983115937315 ) ) ;
#21264 = DIRECTION ( 'NONE',  ( 0.2815395369041025497, 0.9595496282943490884, 0.000000000000000000 ) ) ;
#21265 = ORIENTED_EDGE ( 'NONE', *, *, #17254, .F. ) ;
#21266 = CARTESIAN_POINT ( 'NONE',  ( 1.604951280288043014, -4.392199147046020435, -6.260585232200001293 ) ) ;
#21267 = CARTESIAN_POINT ( 'NONE',  ( -1.782928038406566884, 3.983823234458335527, -22.23780126169999960 ) ) ;
#21268 = CYLINDRICAL_SURFACE ( 'NONE', #2260, 1.099999999999999867 ) ;
#21269 = EDGE_CURVE ( 'NONE', #26433, #29406, #15098, .T. ) ;
#21270 = DIRECTION ( 'NONE',  ( -1.000000000000000000, 0.000000000000000000, 0.000000000000000000 ) ) ;
#21271 = DIRECTION ( 'NONE',  ( 0.000000000000000000, 0.000000000000000000, 1.000000000000000000 ) ) ;
#21272 = CARTESIAN_POINT ( 'NONE',  ( -27.79999999999999716, -2.354383354940000152E-11, 222.0000000000000000 ) ) ;
#21273 = CARTESIAN_POINT ( 'NONE',  ( -23.51354662350000169, -14.83147814589999847, 225.2084356629999888 ) ) ;
#21274 = CARTESIAN_POINT ( 'NONE',  ( 27.77512470430000135, 2.244123299190000168E-11, 229.2930777930000090 ) ) ;
#21275 = CARTESIAN_POINT ( 'NONE',  ( 1.495522319900055574, -27.76012052182101542, 5.506490228000010312 ) ) ;
#21276 = CARTESIAN_POINT ( 'NONE',  ( -10.00000000022208901, -26.89269887560480043, -15.86139282056708133 ) ) ;
#21277 = ORIENTED_EDGE ( 'NONE', *, *, #27698, .F. ) ;
#21278 = CARTESIAN_POINT ( 'NONE',  ( -5.545418199629476241, -2.237997381628727300, -59.38491726642499202 ) ) ;
#21279 = AXIS2_PLACEMENT_3D ( 'NONE', #23763, #30684, #6759 ) ;
#21280 = CARTESIAN_POINT ( 'NONE',  ( -4.884981308350000102E-15, -2.100000000000000089, 226.6412452697800006 ) ) ;
#21281 = VERTEX_POINT ( 'NONE', #4363 ) ;
#21282 = CARTESIAN_POINT ( 'NONE',  ( 8.700000000275743162, -15.22877080015275908, -33.11623335687269076 ) ) ;
#21283 = CARTESIAN_POINT ( 'NONE',  ( -28.50000000000000000, -5.684341886079999373E-14, 229.0000000000000000 ) ) ;
#21284 = EDGE_LOOP ( 'NONE', ( #14267, #4597, #27505, #2218 ) ) ;
#21285 = CARTESIAN_POINT ( 'NONE',  ( 8.699999999516576210, -29.80249410823907752, -29.47052640017699687 ) ) ;
#21286 = LINE ( 'NONE', #9319, #28856 ) ;
#21287 = ORIENTED_EDGE ( 'NONE', *, *, #14968, .T. ) ;
#21288 = EDGE_LOOP ( 'NONE', ( #27549, #6213, #26126, #4717, #29526, #24043, #14522 ) ) ;
#21289 = ORIENTED_EDGE ( 'NONE', *, *, #11201, .F. ) ;
#21290 = SHAPE_REPRESENTATION_RELATIONSHIP ( 'NONE' , 'NONE' ,  #24039, #17044 ) ;
#21291 = ORIENTED_EDGE ( 'NONE', *, *, #25827, .T. ) ;
#21292 = CARTESIAN_POINT ( 'NONE',  ( 24.49145441566124148, -14.57548795709913847, 5.680829342999987652 ) ) ;
#21293 = B_SPLINE_CURVE_WITH_KNOTS ( 'NONE', 3,
 ( #9845, #21967, #14263, #26828, #4966, #23869, #14578, #2310, #419, #24165 ),
 .UNSPECIFIED., .F., .F.,
 ( 4, 2, 2, 2, 4 ),
 ( 0.000000000000000000, 0.2500000000000000000, 0.5000000000000000000, 0.7500000000000000000, 1.000000000000000000 ),
 .UNSPECIFIED. ) ;
#21294 = DIRECTION ( 'NONE',  ( 0.000000000000000000, 0.000000000000000000, -1.000000000000000000 ) ) ;
#21296 = CARTESIAN_POINT ( 'NONE',  ( 1.515105966928380399, -5.232275150219822812, -66.90367649362498526 ) ) ;
#21295 = VECTOR ( 'NONE', #20933, 1000.000000000000000 ) ;
#21298 = ADVANCED_FACE ( 'NONE', ( #25461 ), #3715, .F. ) ;
#21297 = AXIS2_PLACEMENT_3D ( 'NONE', #17164, #19385, #28975 ) ;
#21299 = CARTESIAN_POINT ( 'NONE',  ( 27.79999999980000069, -7.282770092329999834, 229.1414213560000235 ) ) ;
#21300 = CIRCLE ( 'NONE', #10729, 1.472846691535505848 ) ;
#21301 = B_SPLINE_CURVE_WITH_KNOTS ( 'NONE', 3,
 ( #19070, #512, #2549, #28666, #12443, #22061 ),
 .UNSPECIFIED., .F., .F.,
 ( 4, 2, 4 ),
 ( 0.000000000000000000, 0.5000000000000000000, 1.000000000000000000 ),
 .UNSPECIFIED. ) ;
#21302 = CARTESIAN_POINT ( 'NONE',  ( 24.14762151235643728, -13.77513428986648059, 226.1000014190000513 ) ) ;
#21303 = CARTESIAN_POINT ( 'NONE',  ( 27.33171840929999874, -5.762472401450000170, 222.0000000000000000 ) ) ;
#21304 = CARTESIAN_POINT ( 'NONE',  ( 0.03533597109940000286, -28.50021994999999819, 226.1000014189999945 ) ) ;
#21305 = ORIENTED_EDGE ( 'NONE', *, *, #21872, .T. ) ;
#21306 = CARTESIAN_POINT ( 'NONE',  ( -18.70388666750742246, 19.99992613001282038, -0.5969568546230863415 ) ) ;
#21307 = CARTESIAN_POINT ( 'NONE',  ( 1.757687669117797835, -5.210066540036287996, -14.26414732020001175 ) ) ;
#21308 = DIRECTION ( 'NONE',  ( 0.000000000000000000, 0.3420201433259318913, -0.9396926207858126157 ) ) ;
#21309 = CARTESIAN_POINT ( 'NONE',  ( -27.29371452669260734, -0.4966198192113801535, -0.6577119969999878357 ) ) ;
#21310 = EDGE_LOOP ( 'NONE', ( #19515, #21572, #7236, #8658 ) ) ;
#21311 = CARTESIAN_POINT ( 'NONE',  ( -2.220446049249999755E-16, -0.1455297029551360921, -71.05965357398815740 ) ) ;
#21312 = CARTESIAN_POINT ( 'NONE',  ( 1.344125205454980154, -28.46870209102154448, 4.240358041999986227 ) ) ;
#21313 = CARTESIAN_POINT ( 'NONE',  ( -23.55406854719999998, 16.04544955540000117, 222.0000000000000000 ) ) ;
#21314 = DIRECTION ( 'NONE',  ( -5.551115123049999208E-18, 0.000000000000000000, -1.000000000000000000 ) ) ;
#21315 = DIRECTION ( 'NONE',  ( -0.000000000000000000, -0.000000000000000000, -1.000000000000000000 ) ) ;
#21316 = CARTESIAN_POINT ( 'NONE',  ( 12.77819780750000156, 20.99999999999999645, -56.09999999999999432 ) ) ;
#21317 = FACE_OUTER_BOUND ( 'NONE', #28684, .T. ) ;
#21318 = AXIS2_PLACEMENT_3D ( 'NONE', #113, #4974, #11597 ) ;
#21319 = VERTEX_POINT ( 'NONE', #1695 ) ;
#21320 = CARTESIAN_POINT ( 'NONE',  ( -10.00000000066199668, -27.39269908169871925, -31.40000000000157954 ) ) ;
#21321 = CARTESIAN_POINT ( 'NONE',  ( -7.999999999664230366, -18.46837034096498442, -35.57215028647357968 ) ) ;
#21322 = CIRCLE ( 'NONE', #28828, 4.000000000000001776 ) ;
#21323 = VECTOR ( 'NONE', #22638, 1000.000000000000000 ) ;
#21324 = CARTESIAN_POINT ( 'NONE',  ( 0.9411048234942640534, -4.889285007102426306, -68.10000000002503384 ) ) ;
#21325 = LINE ( 'NONE', #4806, #28342 ) ;
#21326 = ADVANCED_FACE ( 'NONE', ( #30797 ), #9076, .F. ) ;
#21327 = FACE_OUTER_BOUND ( 'NONE', #11308, .T. ) ;
#21328 = CARTESIAN_POINT ( 'NONE',  ( -4.846949687726242573, -1.117598880638678738, -44.10000000002499121 ) ) ;
#21329 =( NAMED_UNIT ( * ) SI_UNIT ( $, .STERADIAN. ) SOLID_ANGLE_UNIT ( ) );
#21330 = VERTEX_POINT ( 'NONE', #15857 ) ;
#21331 = CARTESIAN_POINT ( 'NONE',  ( 27.50000000000000000, -3.367667472999999580E-15, 165.0000000000000000 ) ) ;
#21332 = CARTESIAN_POINT ( 'NONE',  ( -4.185763533044374540, 4.163314928055855901, -68.94322600512501253 ) ) ;
#21333 = ORIENTED_EDGE ( 'NONE', *, *, #19198, .T. ) ;
#21334 = EDGE_CURVE ( 'NONE', #8037, #16, #12796, .T. ) ;
#21335 = CARTESIAN_POINT ( 'NONE',  ( -26.80000000000000071, 9.769962616700000205E-15, 186.7828584120000244 ) ) ;
#21336 = CARTESIAN_POINT ( 'NONE',  ( -24.90295381356148141, -14.88027900779681723, 0.2686745300000126235 ) ) ;
#21337 = ORIENTED_EDGE ( 'NONE', *, *, #7989, .T. ) ;
#21339 = CARTESIAN_POINT ( 'NONE',  ( -0.1656472034169999830, 5.899424820049999241, 226.6412452697800006 ) ) ;
#21338 = VECTOR ( 'NONE', #27385, 1000.000000000000000 ) ;
#21340 = VECTOR ( 'NONE', #21985, 1000.000000000000000 ) ;
#21341 = CARTESIAN_POINT ( 'NONE',  ( -24.06750537087913600, -15.26514226587110379, 4.098700198000015504 ) ) ;
#21342 = CARTESIAN_POINT ( 'NONE',  ( 7.999999999977091214, -107.4273096626279482, 14.66297538114749344 ) ) ;
#21343 = AXIS2_PLACEMENT_3D ( 'NONE', #30129, #24942, #25423 ) ;
#21344 = VECTOR ( 'NONE', #18437, 1000.000000000000000 ) ;
#21345 = CARTESIAN_POINT ( 'NONE',  ( -10.69999999999999929, -24.14402093200000010, -27.39080718840000017 ) ) ;
#21346 = DIRECTION ( 'NONE',  ( 1.386461269282634800E-13, 1.000000000000000000, 0.000000000000000000 ) ) ;
#21347 = CARTESIAN_POINT ( 'NONE',  ( 0.000000000000000000, 0.000000000000000000, 231.1412452697749984 ) ) ;
#21348 = ORIENTED_EDGE ( 'NONE', *, *, #21781, .T. ) ;
#21349 = DIRECTION ( 'NONE',  ( -0.8687154346624373913, -0.4953115116563036602, 0.000000000000000000 ) ) ;
#21350 = EDGE_CURVE ( 'NONE', #5339, #15540, #6087, .T. ) ;
#21351 = DIRECTION ( 'NONE',  ( -0.000000000000000000, -0.000000000000000000, -1.000000000000000000 ) ) ;
#21352 = CARTESIAN_POINT ( 'NONE',  ( 10.70000000009999930, -27.00000000000000000, -28.39999999989999679 ) ) ;
#21353 = ADVANCED_FACE ( 'NONE', ( #16317 ), #27807, .F. ) ;
#21354 = CARTESIAN_POINT ( 'NONE',  ( -27.79999999990000248, 4.328052761030000362, 224.8000000000000114 ) ) ;
#21355 = CARTESIAN_POINT ( 'NONE',  ( 8.700000000232593678, -29.57788259996195634, -26.81583080857759072 ) ) ;
#21356 = CARTESIAN_POINT ( 'NONE',  ( 10.20188979230000115, -6.555481593089999670, 230.6412452697800006 ) ) ;
#21357 = DIRECTION ( 'NONE',  ( 0.7071067811896790678, 0.6355433650254203037, -0.3099752105697111126 ) ) ;
#21358 =( GEOMETRIC_REPRESENTATION_CONTEXT ( 3 ) GLOBAL_UNCERTAINTY_ASSIGNED_CONTEXT ( ( #29493 ) ) GLOBAL_UNIT_ASSIGNED_CONTEXT ( ( #11540, #16411, #26324 ) ) REPRESENTATION_CONTEXT ( 'NONE', 'WORKASPACE' ) );
#21359 = DIRECTION ( 'NONE',  ( -0.9316362575375349842, 0.3633921898465292122, -0.000000000000000000 ) ) ;
#21360 = CARTESIAN_POINT ( 'NONE',  ( 0.5234957687185571862, -1.947945353336631991, 227.6412452703391409 ) ) ;
#21361 = CARTESIAN_POINT ( 'NONE',  ( 4.390418465360985678, -3.559810858786684129, -54.92923804942499544 ) ) ;
#21362 = CARTESIAN_POINT ( 'NONE',  ( 11.28406995534932555, 4.374602741788584659, 232.0000002394077683 ) ) ;
#21363 = DIRECTION ( 'NONE',  ( -1.000000000000000000, 0.000000000000000000, -2.257144471330000330E-12 ) ) ;
#21364 = FACE_OUTER_BOUND ( 'NONE', #28134, .T. ) ;
#21365 = AXIS2_PLACEMENT_3D ( 'NONE', #13483, #18195, #16156 ) ;
#21366 = CYLINDRICAL_SURFACE ( 'NONE', #8217, 1.099999999999999201 ) ;
#21367 = ORIENTED_EDGE ( 'NONE', *, *, #17166, .F. ) ;
#21368 = CARTESIAN_POINT ( 'NONE',  ( -23.66327188690000227, -14.59170227459999936, 224.2397348780000073 ) ) ;
#21369 = EDGE_CURVE ( 'NONE', #12344, #29912, #13918, .T. ) ;
#21370 = B_SPLINE_CURVE_WITH_KNOTS ( 'NONE', 5,
 ( #30778, #23085, #6851, #6391, #9532, #9996, #29175, #2909, #2455, #7169, #7015, #9841, #19437, #4818, #21801, #5111, #19126, #258, #12501, #5269, #14882, #28573, #29027, #16910, #23860, #14414, #24473, #100, #24310, #16757, #21652, #26520, #28876, #4960, #12188, #2761, #26824, #17071, #7476, #7327, #30937, #9362, #21491, #12047, #4648, #14573, #28722, #26669, #11887, #7624, #2305, #16605, #26373, #24014, #17219, #14719, #9681, #413, #31089, #18967, #19285, #24160, #12354, #21961, #14259, #2601, #19596, #26213, #20056, #17530, #7776, #15484, #19905, #15030, #15333 ),
 .UNSPECIFIED., .F., .F.,
 ( 6, 3, 3, 3, 3, 3, 3, 3, 3, 3, 3, 3, 3, 3, 3, 3, 3, 3, 3, 3, 3, 3, 3, 3, 6 ),
 ( 8.127326494049999184, 11.49596029219999949, 23.35952330949999833, 35.23214498380000492, 46.71570041139999319, 58.48118637179999268, 70.16173614769999745, 81.99711437660000968, 93.33986353700001359, 104.8204913790000035, 116.3828353250000021, 128.2105526469999859, 137.7231253239999944, 147.2120576640000138, 156.6774103699999898, 168.4624398839999913, 180.2684855139999911, 192.1268167670000082, 203.5147100690000173, 215.0810220189999882, 226.8492753339999979, 238.4740513719999910, 250.2932425120000062, 262.1023078380000015, 271.0195818650000206 ),
 .UNSPECIFIED. ) ;
#21371 = CARTESIAN_POINT ( 'NONE',  ( -4.240613917342964889, -1.711409762446096439, -59.78491726642500481 ) ) ;
#21372 = ORIENTED_EDGE ( 'NONE', *, *, #21740, .F. ) ;
#21373 =( BOUNDED_SURFACE ( )  B_SPLINE_SURFACE ( 5, 5, ( 
 ( #18722, #19038, #15904, #6610, #30388, #3947 ),
 ( #1901, #13540, #2057, #18571, #23152, #16059 ),
 ( #23304, #4566, #21249, #30849, #18415, #1594 ),
 ( #11182, #9280, #16520, #4414, #13700, #25825 ),
 ( #28171, #4260, #13859, #23467, #11496, #21099 ),
 ( #25976, #30694, #18885, #16366, #28324, #6770 ),
 ( #28480, #6921, #26130, #14170, #21715, #636 ),
 ( #483, #24081, #28947, #24226, #5029, #2668 ),
 ( #16985, #4724, #12106, #29096, #14637, #22175 ),
 ( #19511, #17134, #14483, #17292, #19196, #9749 ),
 ( #165, #14, #19356, #24388, #7388, #2823 ),
 ( #26589, #7685, #9597, #10218, #2521, #28781 ),
 ( #12264, #21882, #16671, #14940, #327, #19821 ),
 ( #7081, #9908, #7543, #26736, #26899, #7238 ),
 ( #5173, #26280, #14335, #5336, #14787, #12415 ),
 ( #22032, #16831, #23933, #2370, #19662, #10065 ),
 ( #29246, #24540, #2979, #26438, #4878, #11956 ),
 ( #12569, #21565, #12883, #27500, #5947, #29715 ),
 ( #27050, #13179, #3584, #8142, #29404, #27355 ),
 ( #8455, #24849, #6100, #3278, #22332, #7995 ),
 ( #22487, #15545, #17738, #10674, #10994, #20126 ),
 ( #5798, #1397, #3430, #25152, #18052, #3755 ),
 ( #10375, #936, #13030, #22792, #29560, #1243 ),
 ( #5487, #10528, #19965, #3123, #15395, #24994 ),
 ( #10841, #22639, #17594, #27658, #15697, #13347 ),
 ( #15094, #27202, #8299, #17894, #1082, #20268 ),
 ( #5641, #29866, #7839, #15238, #20426, #30021 ),
 ( #25311, #22952, #784, #17442, #24688, #12722 ),
 ( #6421, #11307, #6573, #18534, #16173, #20907 ),
 ( #18211, #25636, #11461, #28135, #4530, #18381 ),
 ( #30662, #27979, #30809, #1558, #23267, #25786 ),
 ( #23119, #6268, #30345, #4066, #6876, #1861 ),
 ( #21208, #11147, #14133, #16020, #13502, #20744 ),
 ( #25473, #4218, #13661, #1707, #13820, #30506 ),
 ( #13977, #8935, #8775, #23434, #23738, #30181 ),
 ( #21064, #6726, #18843, #9087, #18683, #2174 ),
 ( #16331, #9236, #26094, #28285, #25938, #4373 ),
 ( #23588, #2025, #11612, #28445, #27817, #16480 ),
 ( #3907, #20584, #8611, #15871, #24346, #4992 ),
 ( #21990, #10028, #26858, #23897, #18998, #21522 ),
 ( #21835, #16788, #2632, #17100, #29924, #12224 ),
 ( #9560, #19623, #28746, #28605, #9870, #11766 ),
 ( #19158, #293, #9396, #17248, #26551, #26247 ),
 ( #26698, #2334, #24042, #19470, #14749, #16944 ),
 ( #29061, #29205, #24500, #5303, #14290, #447 ),
 ( #7199, #7506, #11917, #7650, #26403, #7043 ),
 ( #4845, #14906, #24190, #14445, #12382, #2486 ),
 ( #30965, #12073, #5137, #2789, #16633, #9710 ),
 ( #21681, #19317, #131, #4683, #21371, #28909 ),
 ( #14602, #7355, #12532, #12849, #24960, #20232 ),
 ( #3391, #10640, #3241, #1047, #596, #17858 ),
 ( #5758, #5602, #10338, #19931, #29981, #3086 ),
 ( #15664, #17704, #15363, #22451, #17559, #29826 ),
 ( #12996, #2939, #24806, #22608, #8415, #12683 ),
 ( #22139, #27318, #8264, #899, #27167, #27465 ),
 ( #5907, #10181, #10492, #15509, #20394, #27621 ),
 ( #7806, #6067, #19780, #20090, #29363, #25116 ),
 ( #18014, #22293, #3551, #29520, #22754, #13144 ),
 ( #17405, #27011, #1203, #5452, #10799, #15058 ),
 ( #24653, #29681, #747, #7958, #8108, #15204 ),
 ( #13626, #27945, #11268, #4183, #30145, #13780 ),
 ( #13462, #1990, #11112, #1360, #23399, #25273 ),
 ( #3872, #1830, #22919, #30773, #8896, #8575 ),
 ( #30627, #15834, #6387, #11424, #28248, #30471 ),
 ( #21025, #11579, #6848, #9202, #27780, #13941 ),
 ( #23078, #9054, #6225, #23552, #25440, #10953 ),
 ( #30306, #21176, #6539, #8737, #25908, #1521 ),
 ( #20708, #18176, #18344, #15984, #25595, #3708 ),
 ( #18500, #28413, #6693, #18805, #4028, #28098 ),
 ( #13308, #23230, #18649, #1672, #20548, #20874 ),
 ( #16136, #25751, #16293, #4343, #26209, #4499 ),
 ( #16751, #16449, #14409, #14566, #26664, #11884 ),
 ( #26368, #29171, #21796, #408, #9835, #24010 ),
 ( #21647, #2597, #5106, #21954, #9358, #28569 ),
 ( #2755, #16599, #12184, #23856, #14715, #251 ),
 ( #21332, #9991, #9675, #19590, #24156, #17065 ),
 ( #14099, #4814, #7469, #21488, #2450, #19122 ),
 ( #12041, #28716, #96, #26514, #30934, #4955 ) ),
 .UNSPECIFIED., .F., .F., .T. ) 
 B_SPLINE_SURFACE_WITH_KNOTS ( ( 6, 3, 3, 3, 3, 3, 3, 3, 3, 3, 3, 3, 3, 3, 3, 3, 3, 3, 3, 3, 3, 3, 3, 3, 3, 6 ),
 ( 6, 6 ),
 ( 0.000000000000000000, 11.49596029219999949, 23.35952330949999833, 35.23214498380000492, 46.71570041140000029, 58.48118637179999979, 70.16173614769999745, 81.99711437660000968, 93.33986353700001359, 104.8204913790000035, 116.3828353250000021, 128.2105526469999859, 137.7231253239999944, 147.2120576640000138, 156.6774103699999898, 168.4624398839999913, 180.2684855139999911, 192.1268167670000082, 203.5147100690000173, 215.0810220189999882, 226.8492753339999979, 238.4740513719999910, 250.2932425120000062, 262.1023078380000015, 273.4723917590000042, 284.7968047250000154 ),
 ( 6.674405137519999975, 13.34881027499999995 ),
 .UNSPECIFIED. ) 
 GEOMETRIC_REPRESENTATION_ITEM ( )  RATIONAL_B_SPLINE_SURFACE ( (
 ( 0.2500000000000000000, 0.2500000000000000000, 0.2999999999999999889, 0.4000000000000000222, 0.5999999999999999778, 1.000000000000000000),
 ( 0.2500000000000000000, 0.2500000000000000000, 0.2999999999999999889, 0.4000000000000000222, 0.5999999999999999778, 1.000000000000000000),
 ( 0.2500000000000000000, 0.2500000000000000000, 0.2999999999999999889, 0.4000000000000000222, 0.5999999999999999778, 1.000000000000000000),
 ( 0.2500000000000000000, 0.2500000000000000000, 0.2999999999999999889, 0.4000000000000000222, 0.5999999999999999778, 1.000000000000000000),
 ( 0.2500000000000000000, 0.2500000000000000000, 0.2999999999999999889, 0.4000000000000000222, 0.5999999999999999778, 1.000000000000000000),
 ( 0.2500000000000000000, 0.2500000000000000000, 0.2999999999999999889, 0.4000000000000000222, 0.5999999999999999778, 1.000000000000000000),
 ( 0.2500000000000000000, 0.2500000000000000000, 0.2999999999999999889, 0.4000000000000000222, 0.5999999999999999778, 1.000000000000000000),
 ( 0.2500000000000000000, 0.2500000000000000000, 0.2999999999999999889, 0.4000000000000000222, 0.5999999999999999778, 1.000000000000000000),
 ( 0.2500000000000000000, 0.2500000000000000000, 0.2999999999999999889, 0.4000000000000000222, 0.5999999999999999778, 1.000000000000000000),
 ( 0.2500000000000000000, 0.2500000000000000000, 0.2999999999999999889, 0.4000000000000000222, 0.5999999999999999778, 1.000000000000000000),
 ( 0.2500000000000000000, 0.2500000000000000000, 0.2999999999999999889, 0.4000000000000000222, 0.5999999999999999778, 1.000000000000000000),
 ( 0.2500000000000000000, 0.2500000000000000000, 0.2999999999999999889, 0.4000000000000000222, 0.5999999999999999778, 1.000000000000000000),
 ( 0.2500000000000000000, 0.2500000000000000000, 0.2999999999999999889, 0.4000000000000000222, 0.5999999999999999778, 1.000000000000000000),
 ( 0.2500000000000000000, 0.2500000000000000000, 0.2999999999999999889, 0.4000000000000000222, 0.5999999999999999778, 1.000000000000000000),
 ( 0.2500000000000000000, 0.2500000000000000000, 0.2999999999999999889, 0.4000000000000000222, 0.5999999999999999778, 1.000000000000000000),
 ( 0.2500000000000000000, 0.2500000000000000000, 0.2999999999999999889, 0.4000000000000000222, 0.5999999999999999778, 1.000000000000000000),
 ( 0.2500000000000000000, 0.2500000000000000000, 0.2999999999999999889, 0.4000000000000000222, 0.5999999999999999778, 1.000000000000000000),
 ( 0.2500000000000000000, 0.2500000000000000000, 0.2999999999999999889, 0.4000000000000000222, 0.5999999999999999778, 1.000000000000000000),
 ( 0.2500000000000000000, 0.2500000000000000000, 0.2999999999999999889, 0.4000000000000000222, 0.5999999999999999778, 1.000000000000000000),
 ( 0.2500000000000000000, 0.2500000000000000000, 0.2999999999999999889, 0.4000000000000000222, 0.5999999999999999778, 1.000000000000000000),
 ( 0.2500000000000000000, 0.2500000000000000000, 0.2999999999999999889, 0.4000000000000000222, 0.5999999999999999778, 1.000000000000000000),
 ( 0.2500000000000000000, 0.2500000000000000000, 0.2999999999999999889, 0.4000000000000000222, 0.5999999999999999778, 1.000000000000000000),
 ( 0.2500000000000000000, 0.2500000000000000000, 0.2999999999999999889, 0.4000000000000000222, 0.5999999999999999778, 1.000000000000000000),
 ( 0.2500000000000000000, 0.2500000000000000000, 0.2999999999999999889, 0.4000000000000000222, 0.5999999999999999778, 1.000000000000000000),
 ( 0.2500000000000000000, 0.2500000000000000000, 0.2999999999999999889, 0.4000000000000000222, 0.5999999999999999778, 1.000000000000000000),
 ( 0.2500000000000000000, 0.2500000000000000000, 0.2999999999999999889, 0.4000000000000000222, 0.5999999999999999778, 1.000000000000000000),
 ( 0.2500000000000000000, 0.2500000000000000000, 0.2999999999999999889, 0.4000000000000000222, 0.5999999999999999778, 1.000000000000000000),
 ( 0.2500000000000000000, 0.2500000000000000000, 0.2999999999999999889, 0.4000000000000000222, 0.5999999999999999778, 1.000000000000000000),
 ( 0.2500000000000000000, 0.2500000000000000000, 0.2999999999999999889, 0.4000000000000000222, 0.5999999999999999778, 1.000000000000000000),
 ( 0.2500000000000000000, 0.2500000000000000000, 0.2999999999999999889, 0.4000000000000000222, 0.5999999999999999778, 1.000000000000000000),
 ( 0.2500000000000000000, 0.2500000000000000000, 0.2999999999999999889, 0.4000000000000000222, 0.5999999999999999778, 1.000000000000000000),
 ( 0.2500000000000000000, 0.2500000000000000000, 0.2999999999999999889, 0.4000000000000000222, 0.5999999999999999778, 1.000000000000000000),
 ( 0.2500000000000000000, 0.2500000000000000000, 0.2999999999999999889, 0.4000000000000000222, 0.5999999999999999778, 1.000000000000000000),
 ( 0.2500000000000000000, 0.2500000000000000000, 0.2999999999999999889, 0.4000000000000000222, 0.5999999999999999778, 1.000000000000000000),
 ( 0.2500000000000000000, 0.2500000000000000000, 0.2999999999999999889, 0.4000000000000000222, 0.5999999999999999778, 1.000000000000000000),
 ( 0.2500000000000000000, 0.2500000000000000000, 0.2999999999999999889, 0.4000000000000000222, 0.5999999999999999778, 1.000000000000000000),
 ( 0.2500000000000000000, 0.2500000000000000000, 0.2999999999999999889, 0.4000000000000000222, 0.5999999999999999778, 1.000000000000000000),
 ( 0.2500000000000000000, 0.2500000000000000000, 0.2999999999999999889, 0.4000000000000000222, 0.5999999999999999778, 1.000000000000000000),
 ( 0.2500000000000000000, 0.2500000000000000000, 0.2999999999999999889, 0.4000000000000000222, 0.5999999999999999778, 1.000000000000000000),
 ( 0.2500000000000000000, 0.2500000000000000000, 0.2999999999999999889, 0.4000000000000000222, 0.5999999999999999778, 1.000000000000000000),
 ( 0.2500000000000000000, 0.2500000000000000000, 0.2999999999999999889, 0.4000000000000000222, 0.5999999999999999778, 1.000000000000000000),
 ( 0.2500000000000000000, 0.2500000000000000000, 0.2999999999999999889, 0.4000000000000000222, 0.5999999999999999778, 1.000000000000000000),
 ( 0.2500000000000000000, 0.2500000000000000000, 0.2999999999999999889, 0.4000000000000000222, 0.5999999999999999778, 1.000000000000000000),
 ( 0.2500000000000000000, 0.2500000000000000000, 0.2999999999999999889, 0.4000000000000000222, 0.5999999999999999778, 1.000000000000000000),
 ( 0.2500000000000000000, 0.2500000000000000000, 0.2999999999999999889, 0.4000000000000000222, 0.5999999999999999778, 1.000000000000000000),
 ( 0.2500000000000000000, 0.2500000000000000000, 0.2999999999999999889, 0.4000000000000000222, 0.5999999999999999778, 1.000000000000000000),
 ( 0.2500000000000000000, 0.2500000000000000000, 0.2999999999999999889, 0.4000000000000000222, 0.5999999999999999778, 1.000000000000000000),
 ( 0.2500000000000000000, 0.2500000000000000000, 0.2999999999999999889, 0.4000000000000000222, 0.5999999999999999778, 1.000000000000000000),
 ( 0.2500000000000000000, 0.2500000000000000000, 0.2999999999999999889, 0.4000000000000000222, 0.5999999999999999778, 1.000000000000000000),
 ( 0.2500000000000000000, 0.2500000000000000000, 0.2999999999999999889, 0.4000000000000000222, 0.5999999999999999778, 1.000000000000000000),
 ( 0.2500000000000000000, 0.2500000000000000000, 0.2999999999999999889, 0.4000000000000000222, 0.5999999999999999778, 1.000000000000000000),
 ( 0.2500000000000000000, 0.2500000000000000000, 0.2999999999999999889, 0.4000000000000000222, 0.5999999999999999778, 1.000000000000000000),
 ( 0.2500000000000000000, 0.2500000000000000000, 0.2999999999999999889, 0.4000000000000000222, 0.5999999999999999778, 1.000000000000000000),
 ( 0.2500000000000000000, 0.2500000000000000000, 0.2999999999999999889, 0.4000000000000000222, 0.5999999999999999778, 1.000000000000000000),
 ( 0.2500000000000000000, 0.2500000000000000000, 0.2999999999999999889, 0.4000000000000000222, 0.5999999999999999778, 1.000000000000000000),
 ( 0.2500000000000000000, 0.2500000000000000000, 0.2999999999999999889, 0.4000000000000000222, 0.5999999999999999778, 1.000000000000000000),
 ( 0.2500000000000000000, 0.2500000000000000000, 0.2999999999999999889, 0.4000000000000000222, 0.5999999999999999778, 1.000000000000000000),
 ( 0.2500000000000000000, 0.2500000000000000000, 0.2999999999999999889, 0.4000000000000000222, 0.5999999999999999778, 1.000000000000000000),
 ( 0.2500000000000000000, 0.2500000000000000000, 0.2999999999999999889, 0.4000000000000000222, 0.5999999999999999778, 1.000000000000000000),
 ( 0.2500000000000000000, 0.2500000000000000000, 0.2999999999999999889, 0.4000000000000000222, 0.5999999999999999778, 1.000000000000000000),
 ( 0.2500000000000000000, 0.2500000000000000000, 0.2999999999999999889, 0.4000000000000000222, 0.5999999999999999778, 1.000000000000000000),
 ( 0.2500000000000000000, 0.2500000000000000000, 0.2999999999999999889, 0.4000000000000000222, 0.5999999999999999778, 1.000000000000000000),
 ( 0.2500000000000000000, 0.2500000000000000000, 0.2999999999999999889, 0.4000000000000000222, 0.5999999999999999778, 1.000000000000000000),
 ( 0.2500000000000000000, 0.2500000000000000000, 0.2999999999999999889, 0.4000000000000000222, 0.5999999999999999778, 1.000000000000000000),
 ( 0.2500000000000000000, 0.2500000000000000000, 0.2999999999999999889, 0.4000000000000000222, 0.5999999999999999778, 1.000000000000000000),
 ( 0.2500000000000000000, 0.2500000000000000000, 0.2999999999999999889, 0.4000000000000000222, 0.5999999999999999778, 1.000000000000000000),
 ( 0.2500000000000000000, 0.2500000000000000000, 0.2999999999999999889, 0.4000000000000000222, 0.5999999999999999778, 1.000000000000000000),
 ( 0.2500000000000000000, 0.2500000000000000000, 0.2999999999999999889, 0.4000000000000000222, 0.5999999999999999778, 1.000000000000000000),
 ( 0.2500000000000000000, 0.2500000000000000000, 0.2999999999999999889, 0.4000000000000000222, 0.5999999999999999778, 1.000000000000000000),
 ( 0.2500000000000000000, 0.2500000000000000000, 0.2999999999999999889, 0.4000000000000000222, 0.5999999999999999778, 1.000000000000000000),
 ( 0.2500000000000000000, 0.2500000000000000000, 0.2999999999999999889, 0.4000000000000000222, 0.5999999999999999778, 1.000000000000000000),
 ( 0.2500000000000000000, 0.2500000000000000000, 0.2999999999999999889, 0.4000000000000000222, 0.5999999999999999778, 1.000000000000000000),
 ( 0.2500000000000000000, 0.2500000000000000000, 0.2999999999999999889, 0.4000000000000000222, 0.5999999999999999778, 1.000000000000000000),
 ( 0.2500000000000000000, 0.2500000000000000000, 0.2999999999999999889, 0.4000000000000000222, 0.5999999999999999778, 1.000000000000000000),
 ( 0.2500000000000000000, 0.2500000000000000000, 0.2999999999999999889, 0.4000000000000000222, 0.5999999999999999778, 1.000000000000000000),
 ( 0.2500000000000000000, 0.2500000000000000000, 0.2999999999999999889, 0.4000000000000000222, 0.5999999999999999778, 1.000000000000000000),
 ( 0.2500000000000000000, 0.2500000000000000000, 0.2999999999999999889, 0.4000000000000000222, 0.5999999999999999778, 1.000000000000000000),
 ( 0.2500000000000000000, 0.2500000000000000000, 0.2999999999999999889, 0.4000000000000000222, 0.5999999999999999778, 1.000000000000000000) ) ) 
 REPRESENTATION_ITEM ( '' )  SURFACE ( )  );
#21374 = ORIENTED_EDGE ( 'NONE', *, *, #3854, .T. ) ;
#21375 = DIRECTION ( 'NONE',  ( 0.000000000000000000, 1.000000000000000000, 0.000000000000000000 ) ) ;
#21376 = ORIENTED_EDGE ( 'NONE', *, *, #18525, .T. ) ;
#21377 = AXIS2_PLACEMENT_3D ( 'NONE', #9774, #4582, #28966 ) ;
#21378 = AXIS2_PLACEMENT_3D ( 'NONE', #28641, #10069, #24691 ) ;
#21379 = FACE_OUTER_BOUND ( 'NONE', #1429, .T. ) ;
#21380 = EDGE_CURVE ( 'NONE', #30700, #25431, #4552, .T. ) ;
#21381 = CARTESIAN_POINT ( 'NONE',  ( -8.699999999640422033, -12.54233388092882784, -39.16320152032577795 ) ) ;
#21382 = CARTESIAN_POINT ( 'NONE',  ( -25.38146355688631317, 12.59839640959181395, 8.000000000000007105 ) ) ;
#21383 = CARTESIAN_POINT ( 'NONE',  ( -1.705642473229999956, -12.17534878329999870, 232.6627648150000027 ) ) ;
#21384 = FACE_BOUND ( 'NONE', #15063, .T. ) ;
#21385 = CARTESIAN_POINT ( 'NONE',  ( 27.92857142909999979, -3.420150602509999660E-15, 87.93968498519998889 ) ) ;
#21386 = CARTESIAN_POINT ( 'NONE',  ( -2.150134890876696847, -3.785840986416655340, -6.685065142700001850 ) ) ;
#21387 = CARTESIAN_POINT ( 'NONE',  ( 21.13564515570000069, -21.27093644839999698, 229.4982322489999831 ) ) ;
#21388 = B_SPLINE_CURVE_WITH_KNOTS ( 'NONE', 5,
 ( #26888, #5327, #12561, #625, #19808, #10208 ),
 .UNSPECIFIED., .F., .F.,
 ( 6, 6 ),
 ( -2.319815200109999864, 0.000000000000000000 ),
 .UNSPECIFIED. ) ;
#21389 = VERTEX_POINT ( 'NONE', #6560 ) ;
#21390 = CARTESIAN_POINT ( 'NONE',  ( -24.09883371379999772, -15.21565466309999870, 224.8957841300000098 ) ) ;
#21391 = EDGE_CURVE ( 'NONE', #10044, #14421, #13260, .T. ) ;
#21392 = CARTESIAN_POINT ( 'NONE',  ( 4.190083271568243894, -3.954132654168471817, -18.63565260999999751 ) ) ;
#21393 = CARTESIAN_POINT ( 'NONE',  ( -27.79999999999999716, -2.358036054649999912E-11, 226.2000000000000171 ) ) ;
#21394 = DIRECTION ( 'NONE',  ( -0.8775825618903722036, -0.4794255386042040601, 0.000000000000000000 ) ) ;
#21395 = EDGE_CURVE ( 'NONE', #26472, #19928, #828, .T. ) ;
#21396 = CARTESIAN_POINT ( 'NONE',  ( -0.1368966847449999968, 12.12573834550000029, 230.6412452697800006 ) ) ;
#21397 = CARTESIAN_POINT ( 'NONE',  ( 27.54391552369999729, -3.373045395939999845E-15, 192.9562530129999800 ) ) ;
#21398 = PRODUCT_DEFINITION ( 'UNKNOWN', '', #26920, #15959 ) ;
#21399 = CARTESIAN_POINT ( 'NONE',  ( -18.92328505709462405, 19.72870074452574940, 0.1493323239999955199 ) ) ;
#21400 = DIRECTION ( 'NONE',  ( 0.000000000000000000, 0.000000000000000000, 1.000000000000000000 ) ) ;
#21401 = CARTESIAN_POINT ( 'NONE',  ( -23.72659782641452608, -12.46160334549828619, 4.711904017072684248 ) ) ;
#21402 = CARTESIAN_POINT ( 'NONE',  ( -24.54452542612009225, -14.48555670042145138, 6.079852602000002548 ) ) ;
#21403 = PRODUCT_DEFINITION_FORMATION_WITH_SPECIFIED_SOURCE ( 'ANY', '', #23487, .NOT_KNOWN. ) ;
#21404 = CARTESIAN_POINT ( 'NONE',  ( -24.32472894358752313, 13.45989150749028873, 3.899998581000013509 ) ) ;
#21405 = ORIENTED_EDGE ( 'NONE', *, *, #1552, .T. ) ;
#21406 = CARTESIAN_POINT ( 'NONE',  ( 4.517774681172858742, -31.77982753731929577, -80.44524082266653409 ) ) ;
#21407 =( LENGTH_UNIT ( ) NAMED_UNIT ( * ) SI_UNIT ( .MILLI., .METRE. ) );
#21408 = ADVANCED_FACE ( 'NONE', ( #20571 ), #416, .F. ) ;
#21409 = CARTESIAN_POINT ( 'NONE',  ( -7.999999999653043758, -13.95409160420028449, -37.06321646920958557 ) ) ;
#21410 = ORIENTED_EDGE ( 'NONE', *, *, #28773, .T. ) ;
#21411 = DIRECTION ( 'NONE',  ( -1.000000000000000000, 5.665498452320000818E-16, 0.000000000000000000 ) ) ;
#21412 = EDGE_LOOP ( 'NONE', ( #8526, #27356, #4148, #14975 ) ) ;
#21413 = ORIENTED_EDGE ( 'NONE', *, *, #12685, .T. ) ;
#21414 = EDGE_CURVE ( 'NONE', #11584, #18993, #2620, .T. ) ;
#21415 = DIRECTION ( 'NONE',  ( 0.000000000000000000, 0.000000000000000000, 1.000000000000000000 ) ) ;
#21416 = ORIENTED_EDGE ( 'NONE', *, *, #27309, .T. ) ;
#21417 = CARTESIAN_POINT ( 'NONE',  ( -17.01911899311089371, -10.09155933042922726, 0.000000000000000000 ) ) ;
#21418 = VERTEX_POINT ( 'NONE', #11905 ) ;
#21419 = DIRECTION ( 'NONE',  ( 0.7198537139083028835, -0.6941258031311204890, 0.000000000000000000 ) ) ;
#21420 = CARTESIAN_POINT ( 'NONE',  ( 23.23277125981546476, 15.26692728828886025, 4.895813257000003915 ) ) ;
#21421 = ADVANCED_FACE ( 'NONE', ( #9699 ), #26231, .F. ) ;
#21422 = LINE ( 'NONE', #9292, #23545 ) ;
#21423 = CARTESIAN_POINT ( 'NONE',  ( 1.552911329599348633, 4.674210618965234154, -35.70000000000000284 ) ) ;
#21424 = CARTESIAN_POINT ( 'NONE',  ( 10.69999999930000101, -30.00000000000000000, -28.40000000000000213 ) ) ;
#21425 = CARTESIAN_POINT ( 'NONE',  ( -24.60726957497166367, 14.37955347300500364, 5.901399683999997592 ) ) ;
#21426 = LINE ( 'NONE', #14499, #25695 ) ;
#21427 = CARTESIAN_POINT ( 'NONE',  ( -19.18334381879999739, 20.00000379799999806, 230.4459753579999983 ) ) ;
#21428 = CARTESIAN_POINT ( 'NONE',  ( -2.365148379994555849, -4.164425085035065699, -7.622565142700000074 ) ) ;
#21429 = CARTESIAN_POINT ( 'NONE',  ( 2.499950477468915189, 3.566222500441431187, -28.71106724380000230 ) ) ;
#21430 = DIRECTION ( 'NONE',  ( 1.000000000000000000, 0.000000000000000000, 0.000000000000000000 ) ) ;
#21431 = CARTESIAN_POINT ( 'NONE',  ( -23.72659769747987824, -12.46160974968614887, 224.7121835346307535 ) ) ;
#21432 = CARTESIAN_POINT ( 'NONE',  ( 0.000000000000000000, 20.99999999999999645, -44.10000000017154065 ) ) ;
#21433 = CARTESIAN_POINT ( 'NONE',  ( -22.97554992469999746, 15.65135060219999907, 222.0000000000000000 ) ) ;
#21434 = CARTESIAN_POINT ( 'NONE',  ( 4.360957369889326252, -0.1505632777267507105, -2.685409721200002320 ) ) ;
#21435 = FACE_OUTER_BOUND ( 'NONE', #22379, .T. ) ;
#21436 = CARTESIAN_POINT ( 'NONE',  ( 7.325158325029101469, -6.564015909067758336, -34.27768470040534510 ) ) ;
#21437 = DIRECTION ( 'NONE',  ( 1.000000000000000000, -1.843431230200084908E-12, 2.650498504963248473E-12 ) ) ;
#21438 = ORIENTED_EDGE ( 'NONE', *, *, #15029, .T. ) ;
#21439 = DIRECTION ( 'NONE',  ( 1.000000000000000000, 0.000000000000000000, 0.000000000000000000 ) ) ;
#21440 = CARTESIAN_POINT ( 'NONE',  ( -5.151963982244392781, -3.152247574024123811, -21.90799200640000777 ) ) ;
#21441 = ORIENTED_EDGE ( 'NONE', *, *, #23945, .F. ) ;
#21442 = CARTESIAN_POINT ( 'NONE',  ( 23.81569860410000317, -13.75000000000000000, 6.099999999630000502 ) ) ;
#21443 = CARTESIAN_POINT ( 'NONE',  ( 24.41841038956698640, 14.69667349781389376, 3.899998581000013509 ) ) ;
#21444 = ADVANCED_FACE ( 'NONE', ( #9225 ), #28897, .F. ) ;
#21445 = B_SPLINE_CURVE_WITH_KNOTS ( 'NONE', 3,
 ( #16280, #25898, #1191, #9515, #21320, #19267 ),
 .UNSPECIFIED., .F., .F.,
 ( 4, 2, 4 ),
 ( 0.000000000000000000, 0.5000000000000000000, 1.000000000000000000 ),
 .UNSPECIFIED. ) ;
#21446 = EDGE_LOOP ( 'NONE', ( #7360, #21886, #894, #31083 ) ) ;
#21447 = EDGE_LOOP ( 'NONE', ( #23834, #30966, #16410, #23352 ) ) ;
#21448 = ORIENTED_EDGE ( 'NONE', *, *, #28630, .F. ) ;
#21449 = SURFACE_STYLE_FILL_AREA ( #2711 ) ;
#21450 = ORIENTED_EDGE ( 'NONE', *, *, #6362, .T. ) ;
#21451 = CYLINDRICAL_SURFACE ( 'NONE', #30048, 10.00000000000000178 ) ;
#21452 = ADVANCED_FACE ( 'NONE', ( #26540, #31107 ), #18987, .T. ) ;
#21453 = EDGE_CURVE ( 'NONE', #4187, #7813, #16789, .T. ) ;
#21454 = CARTESIAN_POINT ( 'NONE',  ( 27.03594125075309762, 0.4919295335571040040, -0.6999999999999784173 ) ) ;
#21455 = DIRECTION ( 'NONE',  ( 0.000000000000000000, 0.000000000000000000, -1.000000000000000000 ) ) ;
#21456 = ORIENTED_EDGE ( 'NONE', *, *, #27913, .T. ) ;
#21457 = CARTESIAN_POINT ( 'NONE',  ( 16.04656078597520974, 10.97998838177520931, -1.452769935612311825 ) ) ;
#21458 = CARTESIAN_POINT ( 'NONE',  ( 24.07552309629999954, -13.90001137829999855, 226.1000014189999945 ) ) ;
#21459 = CARTESIAN_POINT ( 'NONE',  ( -10.35667741062608371, -26.55163333981974816, 40.00000000000000000 ) ) ;
#21460 = CARTESIAN_POINT ( 'NONE',  ( 5.245096043587340162, -0.2338077457563897399, -35.69999999999999574 ) ) ;
#21461 = ORIENTED_EDGE ( 'NONE', *, *, #30801, .T. ) ;
#21462 = CARTESIAN_POINT ( 'NONE',  ( -20.08956181735672430, 20.00001759534566403, 0.2963061688068184263 ) ) ;
#21463 = AXIS2_PLACEMENT_3D ( 'NONE', #28873, #12187, #24472 ) ;
#21464 = CARTESIAN_POINT ( 'NONE',  ( 3.256742448429973624, 4.730705660258329281, -17.21259163649999735 ) ) ;
#21465 = DIRECTION ( 'NONE',  ( 0.000000000000000000, 0.000000000000000000, 1.000000000000000000 ) ) ;
#21466 = CARTESIAN_POINT ( 'NONE',  ( -8.699999999703425857, -29.80249410822303346, -29.47052640025896508 ) ) ;
#21467 = ORIENTED_EDGE ( 'NONE', *, *, #1052, .T. ) ;
#21468 = DIRECTION ( 'NONE',  ( 0.000000000000000000, -0.3420201433259318913, 0.9396926207858126157 ) ) ;
#21469 = CARTESIAN_POINT ( 'NONE',  ( 1.605176535610508326, -27.75389821387976852, 4.999998581000003384 ) ) ;
#21470 = CARTESIAN_POINT ( 'NONE',  ( -2.098672137722010334, -3.287437779826620776, -44.10000000002499121 ) ) ;
#21471 = DIRECTION ( 'NONE',  ( 0.6941258031311203780, 0.7198537139083029945, 0.000000000000000000 ) ) ;
#21472 = CARTESIAN_POINT ( 'NONE',  ( 5.242919931573567283, -2.735361231296036699, -61.31790713612500099 ) ) ;
#21473 = CARTESIAN_POINT ( 'NONE',  ( -10.00000000066199490, -26.60730091830108179, -31.40000000000157954 ) ) ;
#21474 = CARTESIAN_POINT ( 'NONE',  ( 8.000000000250089727, -26.69041892760361279, -31.40984194550128805 ) ) ;
#21475 = ORIENTED_EDGE ( 'NONE', *, *, #2907, .F. ) ;
#21476 = CARTESIAN_POINT ( 'NONE',  ( -12.38365826780663426, -23.49682068899581466, -24.64905882652923097 ) ) ;
#21477 = CARTESIAN_POINT ( 'NONE',  ( -17.62526668112344908, -8.236461616547455122, -0.6999999999999784173 ) ) ;
#21478 = EDGE_CURVE ( 'NONE', #2398, #931, #10180, .T. ) ;
#21479 = CARTESIAN_POINT ( 'NONE',  ( -2.324326393622344611, -4.567114707776696925, -68.10000000002501963 ) ) ;
#21480 = CARTESIAN_POINT ( 'NONE',  ( 9.999999999938754769, -26.89269887572167761, -15.86139282090652891 ) ) ;
#21481 = ORIENTED_EDGE ( 'NONE', *, *, #27081, .F. ) ;
#21482 = AXIS2_PLACEMENT_3D ( 'NONE', #22762, #20719, #20884 ) ;
#21483 = CARTESIAN_POINT ( 'NONE',  ( 3.458129700889219116, -0.5397582531354573332, -88.52261276322501260 ) ) ;
#21484 = PRESENTATION_STYLE_ASSIGNMENT (( #17062 ) ) ;
#21485 = CIRCLE ( 'NONE', #17449, 4.000000004070001225 ) ;
#21486 = ORIENTED_EDGE ( 'NONE', *, *, #25923, .F. ) ;
#21487 = CARTESIAN_POINT ( 'NONE',  ( 23.94793942833934963, 15.45149536900696674, 5.679609032776862243 ) ) ;
#21488 = CARTESIAN_POINT ( 'NONE',  ( -1.560798555979769464, 4.306275027539294697, -69.90099036452500059 ) ) ;
#21489 = VERTEX_POINT ( 'NONE', #2163 ) ;
#21490 = CARTESIAN_POINT ( 'NONE',  ( -26.03214543848244844, 7.091100912325356553, 0.000000000000000000 ) ) ;
#21491 = CARTESIAN_POINT ( 'NONE',  ( -0.05052225346893063351, 4.317558364482401601, -57.31818518972499987 ) ) ;
#21492 = DIRECTION ( 'NONE',  ( -0.000000000000000000, -0.000000000000000000, -1.000000000000000000 ) ) ;
#21493 = CARTESIAN_POINT ( 'NONE',  ( -24.38199545545641911, -14.75707035126829147, 3.901343066999990228 ) ) ;
#21494 = CARTESIAN_POINT ( 'NONE',  ( 24.64642659020000082, -14.31106159850000026, 223.9013459049999994 ) ) ;
#21495 = CARTESIAN_POINT ( 'NONE',  ( -7.999999999682144924, -15.00895261645561618, -33.21453337755221469 ) ) ;
#21496 = CARTESIAN_POINT ( 'NONE',  ( -10.69999999992358397, -25.00000000000000355, -8.545053439230965608 ) ) ;
#21497 = CARTESIAN_POINT ( 'NONE',  ( 8.000000000264140709, -18.27877680372071723, -30.94409471150577318 ) ) ;
#21498 = EDGE_LOOP ( 'NONE', ( #3770, #21566, #821, #27626 ) ) ;
#21499 = CARTESIAN_POINT ( 'NONE',  ( 0.000000000000000000, 0.000000000000000000, 190.0000000000000000 ) ) ;
#21500 = EDGE_CURVE ( 'NONE', #12226, #11846, #12773, .T. ) ;
#21501 = CARTESIAN_POINT ( 'NONE',  ( 19.49298387170000169, 19.58648673140000440, 229.5592795560000070 ) ) ;
#21502 = EDGE_CURVE ( 'NONE', #18431, #14341, #28592, .T. ) ;
#21503 = AXIS2_PLACEMENT_3D ( 'NONE', #24617, #5564, #861 ) ;
#21504 = CARTESIAN_POINT ( 'NONE',  ( -26.95773186790000153, 8.656139628340000058, 229.0000000000000000 ) ) ;
#21505 = FACE_OUTER_BOUND ( 'NONE', #9102, .T. ) ;
#21506 = DIRECTION ( 'NONE',  ( -1.000000000000000000, 2.082932338114093583E-15, -6.768115529734696084E-12 ) ) ;
#21507 = CIRCLE ( 'NONE', #25530, 2.299999999990001598 ) ;
#21508 = CARTESIAN_POINT ( 'NONE',  ( 8.999999999770000869, 20.13144615300854312, -44.09999999954493433 ) ) ;
#21509 = CIRCLE ( 'NONE', #13983, 2.999999999999999556 ) ;
#21510 = DIRECTION ( 'NONE',  ( -0.7198537139083028835, 0.6941258031311204890, 0.000000000000000000 ) ) ;
#21511 = CARTESIAN_POINT ( 'NONE',  ( -12.47331730070000155, 20.99999999999999645, -55.90289625529999995 ) ) ;
#21512 = EDGE_CURVE ( 'NONE', #23430, #25954, #22442, .T. ) ;
#21513 = CARTESIAN_POINT ( 'NONE',  ( -26.80000000069999899, 3.281945028329999726E-15, 93.21714158910000947 ) ) ;
#21514 = CARTESIAN_POINT ( 'NONE',  ( 13.67718073920000066, 20.99999999999999645, -57.16242423349999768 ) ) ;
#21515 = CARTESIAN_POINT ( 'NONE',  ( 10.69999999999999929, -120.0000000000000000, -41.24671599705000347 ) ) ;
#21516 = VERTEX_POINT ( 'NONE', #12674 ) ;
#21517 = AXIS2_PLACEMENT_3D ( 'NONE', #20590, #30188, #8620 ) ;
#21518 = CARTESIAN_POINT ( 'NONE',  ( 7.038311529316255921, 4.106927189824788549, -42.82005722189286701 ) ) ;
#21519 = ORIENTED_EDGE ( 'NONE', *, *, #19642, .T. ) ;
#21520 = CARTESIAN_POINT ( 'NONE',  ( 4.373195337096333013, -2.904765488536246387, -36.55875473019999333 ) ) ;
#21521 = EDGE_CURVE ( 'NONE', #17900, #27200, #26353, .T. ) ;
#21522 = CARTESIAN_POINT ( 'NONE',  ( -4.178199994060140199, -1.098053884355548737, -56.45102360502500005 ) ) ;
#21523 = ORIENTED_EDGE ( 'NONE', *, *, #25901, .T. ) ;
#21524 = CIRCLE ( 'NONE', #25552, 27.92857142860000152 ) ;
#21525 = ITEM_DEFINED_TRANSFORMATION ( 'NONE', 'NONE', #13850,  #17722 ) ;
#21526 = ORIENTED_EDGE ( 'NONE', *, *, #25745, .F. ) ;
#21528 = CARTESIAN_POINT ( 'NONE',  ( -15.73360964030186970, 11.02001161816959396, -1.000005633855494125E-09 ) ) ;
#21527 = AXIS2_PLACEMENT_3D ( 'NONE', #27597, #22581, #18316 ) ;
#21529 = EDGE_LOOP ( 'NONE', ( #7159, #17066, #12054, #18179 ) ) ;
#21530 = ADVANCED_FACE ( 'NONE', ( #12987 ), #9767, .T. ) ;
#21531 = CARTESIAN_POINT ( 'NONE',  ( 1.834980886315526805, 1.057731052269877070, 226.6412452697800575 ) ) ;
#21532 = CARTESIAN_POINT ( 'NONE',  ( 17.16657240420000008, 10.97998838177520931, -1.972246272986471594 ) ) ;
#21533 = DIRECTION ( 'NONE',  ( -5.962915006522622422E-16, -0.4383711467890810676, -0.8987940462991651502 ) ) ;
#21534 = PRODUCT_DEFINITION_SHAPE ( 'NONE', 'NONE',  #31139 ) ;
#21535 = MANIFOLD_SOLID_BREP ( 'PartBody', #12051 ) ;
#21536 = CARTESIAN_POINT ( 'NONE',  ( 10.00047450490000145, 7.228941357680000124, 232.6627648150000027 ) ) ;
#21537 = DIRECTION ( 'NONE',  ( -0.1090476345695678556, -0.6986477033489640887, -0.7071067811865475727 ) ) ;
#21538 = FACE_OUTER_BOUND ( 'NONE', #10494, .T. ) ;
#21539 = CARTESIAN_POINT ( 'NONE',  ( 0.2392016894930265591, 6.101552847015987879, -7.337690181100003706 ) ) ;
#21540 = CARTESIAN_POINT ( 'NONE',  ( -28.35924375250000296, 0.000000000000000000, 229.7625741969999922 ) ) ;
#21541 = ORIENTED_EDGE ( 'NONE', *, *, #14555, .T. ) ;
#21542 = LINE ( 'NONE', #16962, #29064 ) ;
#21543 = AXIS2_PLACEMENT_3D ( 'NONE', #25758, #9366, #23562 ) ;
#21544 = CARTESIAN_POINT ( 'NONE',  ( 2.992916622598570608, -2.824380467281231599, -18.53565260999999609 ) ) ;
#21545 = CARTESIAN_POINT ( 'NONE',  ( -0.2820369105234935003, -27.79912531870053272, 226.0732182084217641 ) ) ;
#21546 = CARTESIAN_POINT ( 'NONE',  ( -21.20818545079999851, 16.99505982179999819, 230.6999999999999886 ) ) ;
#21547 = AXIS2_PLACEMENT_3D ( 'NONE', #8651, #12763, #22377 ) ;
#21548 = PLANE ( 'NONE',  #1086 ) ;
#21549 = CARTESIAN_POINT ( 'NONE',  ( -15.97294062935416115, -8.309387060397886771, 0.000000000000000000 ) ) ;
#21550 = CARTESIAN_POINT ( 'NONE',  ( -19.18296382695153213, 19.99999944541083963, -0.4461354429999841997 ) ) ;
#21551 = ADVANCED_FACE ( 'NONE', ( #1039 ), #24949, .T. ) ;
#21552 = CARTESIAN_POINT ( 'NONE',  ( -19.29999999990000248, -27.00000000000000000, -28.39999999989999679 ) ) ;
#21553 = DIRECTION ( 'NONE',  ( 0.000000000000000000, 0.9396926207858125046, 0.3420201433259318358 ) ) ;
#21554 = LINE ( 'NONE', #3, #15313 ) ;
#21555 = AXIS2_PLACEMENT_3D ( 'NONE', #6253, #15856, #13485 ) ;
#21556 = CARTESIAN_POINT ( 'NONE',  ( 10.35000000039999968, -43.95328087560000085, -27.24755286599999948 ) ) ;
#21557 = B_SPLINE_CURVE_WITH_KNOTS ( 'NONE', 5,
 ( #27709, #27557, #13232, #20325, #1455, #8193, #23166, #13714, #11048, #22847, #30234, #8668, #18264, #25524, #1606 ),
 .UNSPECIFIED., .F., .F.,
 ( 6, 3, 3, 3, 6 ),
 ( 0.000000000000000000, 0.1000000000028630903, 0.3999999999999999667, 0.7000000000005727196, 1.000000000000000000 ),
 .UNSPECIFIED. ) ;
#21558 = EDGE_LOOP ( 'NONE', ( #25874, #9625, #3312, #7300, #6746, #8854, #6971 ) ) ;
#21559 = CARTESIAN_POINT ( 'NONE',  ( -17.62526623054365871, -8.236462051082252600, 0.000000000000000000 ) ) ;
#21560 = CARTESIAN_POINT ( 'NONE',  ( -15.73360964037622622, -8.979988381802643360, -0.6999999999999784173 ) ) ;
#21561 = DIRECTION ( 'NONE',  ( 0.000000000000000000, -1.000000000000000000, 0.000000000000000000 ) ) ;
#21562 = EDGE_LOOP ( 'NONE', ( #1784, #14764, #21574, #15142 ) ) ;
#21563 = EDGE_CURVE ( 'NONE', #15790, #25571, #7642, .T. ) ;
#21564 = CARTESIAN_POINT ( 'NONE',  ( 24.73568148353697183, -12.68911065183860920, 4.319165765000021473 ) ) ;
#21565 = CARTESIAN_POINT ( 'NONE',  ( 5.943504367937093136, -0.4395870339238064362, -49.60442242802498924 ) ) ;
#21566 = ORIENTED_EDGE ( 'NONE', *, *, #23999, .T. ) ;
#21567 = ORIENTED_EDGE ( 'NONE', *, *, #24317, .F. ) ;
#21568 = VECTOR ( 'NONE', #22308, 1000.000000000000000 ) ;
#21569 = EDGE_CURVE ( 'NONE', #27894, #5868, #17789, .T. ) ;
#21570 = DIRECTION ( 'NONE',  ( 0.000000000000000000, 0.000000000000000000, 1.000000000000000000 ) ) ;
#21571 = B_SPLINE_SURFACE_WITH_KNOTS ( 'NONE', 5, 1, ( 
 ( #14144, #6431 ),
 ( #25949, #11472 ),
 ( #30358, #18697 ),
 ( #6740, #2034 ),
 ( #11622, #26104 ),
 ( #23749, #26254 ),
 ( #2187, #21383 ),
 ( #30975, #9407 ),
 ( #19011, #4693 ),
 ( #14301, #18390 ),
 ( #16029, #25646 ),
 ( #4076, #10040 ),
 ( #3098, #12083 ),
 ( #27024, #24200 ),
 ( #457, #2495 ),
 ( #19793, #19328 ),
 ( #4855, #7818 ),
 ( #5003, #22150 ),
 ( #15068, #16957 ),
 ( #21691, #26562 ),
 ( #19335, #29376 ),
 ( #19482, #606 ),
 ( #19633, #21536 ),
 ( #9572, #302 ),
 ( #9881, #12392 ),
 ( #5147, #29219 ),
 ( #10193, #140 ),
 ( #24663, #2949 ),
 ( #2642, #28921 ),
 ( #17415, #9721 ) ),
 .UNSPECIFIED., .F., .F., .F.,
 ( 6, 3, 3, 3, 3, 3, 3, 3, 3, 6 ),
 ( 2, 2 ),
 ( 295.9469361829999912, 296.7817637200000149, 302.0406471359999614, 307.2995305649999978, 312.5584139889999733, 317.8172974060000229, 323.0761808360000487, 328.3350642730000004, 333.5939477180000381, 336.3523335059999795 ),
 ( -9.355471259890000464E-07, 0.7003637394550000783 ),
 .UNSPECIFIED. ) ;
#21572 = ORIENTED_EDGE ( 'NONE', *, *, #29562, .T. ) ;
#21573 = CARTESIAN_POINT ( 'NONE',  ( -17.54655709608498881, -9.840444911176506437, 0.000000000000000000 ) ) ;
#21574 = ORIENTED_EDGE ( 'NONE', *, *, #3930, .T. ) ;
#21575 = CARTESIAN_POINT ( 'NONE',  ( 16.06675444876397307, -9.020011618195203695, -1.000005633855494125E-09 ) ) ;
#21576 = DIRECTION ( 'NONE',  ( 0.000000000000000000, 0.000000000000000000, 1.000000000000000000 ) ) ;
#21577 = DIRECTION ( 'NONE',  ( 1.000000000000000000, 0.000000000000000000, 0.000000000000000000 ) ) ;
#21578 = CARTESIAN_POINT ( 'NONE',  ( 0.2009654409541410391, 4.469944785342635285, -35.69999999999999574 ) ) ;
#21579 = ADVANCED_FACE ( 'NONE', ( #10628 ), #19924, .T. ) ;
#21580 = CYLINDRICAL_SURFACE ( 'NONE', #17589, 2.500000000000001776 ) ;
#21581 = CARTESIAN_POINT ( 'NONE',  ( -3.806419540421088321, -0.6621889094791760799, -0.6999999999999992895 ) ) ;
#21582 = CARTESIAN_POINT ( 'NONE',  ( -5.288124922799195993, -8.247920380278689123, -33.45638961376399578 ) ) ;
#21583 = AXIS2_PLACEMENT_3D ( 'NONE', #12319, #6980, #16570 ) ;
#21584 = CARTESIAN_POINT ( 'NONE',  ( -19.06889133170000150, 19.69230209619999883, 229.7995039799999972 ) ) ;
#21585 = CARTESIAN_POINT ( 'NONE',  ( -5.857861475075242019, -1.837656413297739766, -10.62323088900000378 ) ) ;
#21586 = CARTESIAN_POINT ( 'NONE',  ( -1.151230282303595587, -4.494053275198272246, -27.04882611459999353 ) ) ;
#21587 = CARTESIAN_POINT ( 'NONE',  ( 3.063912144317538111, -1.789060389098976911, 0.000000000000000000 ) ) ;
#21588 = ADVANCED_FACE ( 'NONE', ( #27157 ), #27840, .F. ) ;
#21589 = CARTESIAN_POINT ( 'NONE',  ( -3.507110123170089189, -0.4740316117955202246, -90.91470530330329325 ) ) ;
#21590 = CARTESIAN_POINT ( 'NONE',  ( 19.99486320633338465, 19.99999931165986311, 0.1511489130000265302 ) ) ;
#21591 = CARTESIAN_POINT ( 'NONE',  ( 12.59933368536904297, 25.69710080669531038, -59.52534974837554671 ) ) ;
#21592 = CARTESIAN_POINT ( 'NONE',  ( -4.184186767956295405, -1.312611723764782523, -10.02323088899999881 ) ) ;
#21593 = LINE ( 'NONE', #1930, #17244 ) ;
#21594 = CARTESIAN_POINT ( 'NONE',  ( -24.25742564193969031, -13.58028021372842531, 4.319317663000004970 ) ) ;
#21595 = CARTESIAN_POINT ( 'NONE',  ( -9.414213562409999625, -14.63015244271202420, -76.33162510583964888 ) ) ;
#21596 = ORIENTED_EDGE ( 'NONE', *, *, #11873, .F. ) ;
#21597 = ADVANCED_FACE ( 'NONE', ( #29815 ), #9949, .T. ) ;
#21598 = DIRECTION ( 'NONE',  ( -0.000000000000000000, -0.000000000000000000, -1.000000000000000000 ) ) ;
#21599 = CARTESIAN_POINT ( 'NONE',  ( -12.48073050767949965, -32.00000000000000000, -30.16865675522091905 ) ) ;
#21600 = CIRCLE ( 'NONE', #25092, 2.100000000000000089 ) ;
#21601 = VERTEX_POINT ( 'NONE', #3861 ) ;
#21602 = CARTESIAN_POINT ( 'NONE',  ( 23.74292845513278039, -13.87604159523734282, 6.099999999630012937 ) ) ;
#21603 = CARTESIAN_POINT ( 'NONE',  ( 22.41293933140000050, 16.47772227400000489, 222.9999999789999947 ) ) ;
#21604 = ORIENTED_EDGE ( 'NONE', *, *, #8997, .T. ) ;
#21605 = ORIENTED_EDGE ( 'NONE', *, *, #16694, .F. ) ;
#21606 = VERTEX_POINT ( 'NONE', #1663 ) ;
#21607 = CLOSED_SHELL ( 'NONE', ( #24275, #29237, #8654, #4969, #17850, #21202, #21628, #10140, #6685, #31032, #16698, #13640, #26975, #22403, #26096, #17713, #15055 ) ) ;
#21608 = ORIENTED_EDGE ( 'NONE', *, *, #19651, .T. ) ;
#21609 = CARTESIAN_POINT ( 'NONE',  ( 9.999999999959413799, -28.79128384721942524, -25.96367195644973336 ) ) ;
#21610 = CARTESIAN_POINT ( 'NONE',  ( 23.69119887980000172, 20.94188554260000146, 229.0000000000000000 ) ) ;
#21611 = CARTESIAN_POINT ( 'NONE',  ( -7.871622393891488656, -5.774860021632473028, -27.47894970137238957 ) ) ;
#21612 = EDGE_LOOP ( 'NONE', ( #20160, #2462, #109, #16408 ) ) ;
#21613 = CARTESIAN_POINT ( 'NONE',  ( 0.000000000000000000, 20.99999999999999645, -45.10000000000000142 ) ) ;
#21614 = LINE ( 'NONE', #4468, #14169 ) ;
#21615 = CARTESIAN_POINT ( 'NONE',  ( 18.92356420714367360, 19.72862907665551546, 0.1494310229999962214 ) ) ;
#21616 = CARTESIAN_POINT ( 'NONE',  ( 4.440892098500000496E-16, -0.1455297029551360921, -71.05965357398815740 ) ) ;
#21617 = CARTESIAN_POINT ( 'NONE',  ( 2.940048186824491872, -4.025564021813598181, -0.6999991271805777737 ) ) ;
#21618 = VERTEX_POINT ( 'NONE', #29974 ) ;
#21619 = CARTESIAN_POINT ( 'NONE',  ( -24.41841039498785193, -14.69667350221323865, 3.899998581000013509 ) ) ;
#21620 = CARTESIAN_POINT ( 'NONE',  ( -2.227024806490494946, -3.476280271252722542, -18.20544088820000184 ) ) ;
#21621 = DIRECTION ( 'NONE',  ( 0.000000000000000000, 0.000000000000000000, 1.000000000000000000 ) ) ;
#21622 = ADVANCED_FACE ( 'NONE', ( #20538, #13451 ), #23069, .T. ) ;
#21623 = CARTESIAN_POINT ( 'NONE',  ( -27.50000000000000000, 3.367667473009999970E-15, 143.2809019210000088 ) ) ;
#21624 = ORIENTED_EDGE ( 'NONE', *, *, #740, .T. ) ;
#21625 = CARTESIAN_POINT ( 'NONE',  ( 8.000000000489755791, -29.44934466748925672, -30.17621036715362592 ) ) ;
#21626 = CARTESIAN_POINT ( 'NONE',  ( 13.12132034340000075, 21.69999999990000106, -69.22132034359999864 ) ) ;
#21627 = CARTESIAN_POINT ( 'NONE',  ( 26.80000000000000071, -6.394884621839999216E-14, 230.6999999999999886 ) ) ;
#21628 = ADVANCED_FACE ( 'NONE', ( #11103 ), #6377, .T. ) ;
#21629 = DIRECTION ( 'NONE',  ( -0.6941258031311203780, -0.7198537139083029945, 0.000000000000000000 ) ) ;
#21630 = EDGE_CURVE ( 'NONE', #61, #16882, #18333, .T. ) ;
#21631 = CARTESIAN_POINT ( 'NONE',  ( 5.384875807261761516, 2.601783486389667832, -66.85315453642499506 ) ) ;
#21632 = FACE_OUTER_BOUND ( 'NONE', #19935, .T. ) ;
#21634 = EDGE_CURVE ( 'NONE', #27430, #1290, #729, .T. ) ;
#21633 = CARTESIAN_POINT ( 'NONE',  ( -13.92227941755939113, 21.69999999994631423, -67.88484171643710852 ) ) ;
#21635 = VERTEX_POINT ( 'NONE', #6058 ) ;
#21636 = DIRECTION ( 'NONE',  ( 0.000000000000000000, 0.000000000000000000, 1.000000000000000000 ) ) ;
#21637 = DIRECTION ( 'NONE',  ( 0.000000000000000000, 0.000000000000000000, 1.000000000000000000 ) ) ;
#21638 = B_SPLINE_CURVE_WITH_KNOTS ( 'NONE', 5,
 ( #19753, #9843, #29491, #5113, #29032, #10000, #4964, #19599, #10464 ),
 .UNSPECIFIED., .F., .F.,
 ( 6, 3, 6 ),
 ( 0.000000000000000000, 6.585924280900000483, 11.50063931930000116 ),
 .UNSPECIFIED. ) ;
#21639 = VECTOR ( 'NONE', #27669, 1000.000000000000000 ) ;
#21640 = CARTESIAN_POINT ( 'NONE',  ( 1.635351980402913297, -4.635989411471753030, -68.10000000002500542 ) ) ;
#21641 = CARTESIAN_POINT ( 'NONE',  ( -4.639785291165150483, -1.934394008134929788, -68.10000000002501963 ) ) ;
#21642 = EDGE_LOOP ( 'NONE', ( #11117, #18912, #12845, #1083 ) ) ;
#21643 = CARTESIAN_POINT ( 'NONE',  ( 26.49973092449999967, 5.074550867610000182, 230.6999999999999886 ) ) ;
#21644 = MANIFOLD_SOLID_BREP ( 'PartBody', #6526 ) ;
#21645 = ORIENTED_EDGE ( 'NONE', *, *, #13898, .F. ) ;
#21646 = CARTESIAN_POINT ( 'NONE',  ( 8.000000000313141513, -13.45181286506001506, -44.64612647231290765 ) ) ;
#21647 = CARTESIAN_POINT ( 'NONE',  ( -5.434147616959247529, -3.211087428728324866, -68.32382590962500046 ) ) ;
#21648 = AXIS2_PLACEMENT_3D ( 'NONE', #23743, #18687, #21375 ) ;
#21649 = EDGE_LOOP ( 'NONE', ( #26197, #13658, #14710, #20271 ) ) ;
#21650 = CARTESIAN_POINT ( 'NONE',  ( -5.430430790592723156, -2.746024268427175841, -28.56472909259999327 ) ) ;
#21651 = CARTESIAN_POINT ( 'NONE',  ( -2.033405199220553516, -0.5436710271403359940, 226.6412452697799154 ) ) ;
#21652 = CARTESIAN_POINT ( 'NONE',  ( -4.541600168151700423, -0.1148504950298639971, -53.55673954922500002 ) ) ;
#21653 = DIRECTION ( 'NONE',  ( -1.000000000000000000, 0.000000000000000000, 0.000000000000000000 ) ) ;
#21654 = LINE ( 'NONE', #28577, #1495 ) ;
#21655 = CARTESIAN_POINT ( 'NONE',  ( 24.34123158960000310, -14.82477075300000102, 224.0987030360000176 ) ) ;
#21656 = UNCERTAINTY_MEASURE_WITH_UNIT (LENGTH_MEASURE( 1.000000000000000082E-05 ), #620, 'distance_accuracy_value', 'NONE');
#21657 = CARTESIAN_POINT ( 'NONE',  ( -310556.1348510272801, 168981.9135473513743, -353320.2493487302563 ) ) ;
#21658 = CARTESIAN_POINT ( 'NONE',  ( -17.20085693451147790, -21.99999999999968736, -30.75107028161901468 ) ) ;
#21659 = EDGE_LOOP ( 'NONE', ( #7089, #30420, #25639, #15695, #7017, #3178 ) ) ;
#21660 = DIRECTION ( 'NONE',  ( -9.982533390641031007E-25, -1.000000000000000000, 2.257145581550764975E-12 ) ) ;
#21661 = CARTESIAN_POINT ( 'NONE',  ( 1.071233845142131713, -26.77863813576653484, 225.2880959822963973 ) ) ;
#21662 = CARTESIAN_POINT ( 'NONE',  ( -8.249724945169999657, 8.807467740899999953, 231.9999989789999972 ) ) ;
#21663 = CARTESIAN_POINT ( 'NONE',  ( -27.79999999990000248, 4.328052761030000362, 223.3999999999999773 ) ) ;
#21664 = DIRECTION ( 'NONE',  ( 1.000000000000000000, 0.000000000000000000, 0.000000000000000000 ) ) ;
#21665 = CARTESIAN_POINT ( 'NONE',  ( 10.69999999999999929, -130.0000000000000000, -41.24671599790000442 ) ) ;
#21666 = LINE ( 'NONE', #23881, #21256 ) ;
#21668 = EDGE_CURVE ( 'NONE', #11176, #17105, #21445, .T. ) ;
#21667 = CARTESIAN_POINT ( 'NONE',  ( -1.087555936180296001, -26.77834284442311130, 225.2180515729460240 ) ) ;
#21669 = CARTESIAN_POINT ( 'NONE',  ( -25.05552767696902450, 13.58331698520493269, 3.920132093000017193 ) ) ;
#21670 = CARTESIAN_POINT ( 'NONE',  ( -4.960227444680000097, -16.90556345619999945, 230.0904314459999966 ) ) ;
#21671 = VECTOR ( 'NONE', #16932, 1000.000000000000000 ) ;
#21672 = CARTESIAN_POINT ( 'NONE',  ( 9.631484144028339855, 21.69999999997851603, -53.61927559727671166 ) ) ;
#21673 = CARTESIAN_POINT ( 'NONE',  ( -18.95046173579999760, -18.95046173579999760, 115.0000000000000000 ) ) ;
#21674 = DIRECTION ( 'NONE',  ( -1.000000000000000000, -2.587524353642439916E-24, -2.257144471329210308E-12 ) ) ;
#21675 = ORIENTED_EDGE ( 'NONE', *, *, #27570, .T. ) ;
#21676 = CARTESIAN_POINT ( 'NONE',  ( 7.560966790798962833, 3.155924488616837387, -42.35622221269955645 ) ) ;
#21677 = B_SPLINE_CURVE_WITH_KNOTS ( 'NONE', 5,
 ( #2100, #4309, #27744, #23514, #30588, #11693, #25717, #18305, #13905, #21292, #1948, #6188, #11542, #9017, #18460 ),
 .UNSPECIFIED., .F., .F.,
 ( 6, 3, 3, 3, 6 ),
 ( 0.000000000000000000, 0.1000000000022904789, 0.3999999999977094656, 0.7000000000005727196, 1.000000000000000000 ),
 .UNSPECIFIED. ) ;
#21678 = ORIENTED_EDGE ( 'NONE', *, *, #3309, .F. ) ;
#21679 = CARTESIAN_POINT ( 'NONE',  ( 24.91921101730000032, -13.83103916669999833, 226.0027513979999867 ) ) ;
#21680 = EDGE_CURVE ( 'NONE', #8971, #19758, #15288, .T. ) ;
#21681 = CARTESIAN_POINT ( 'NONE',  ( -5.545418199629476241, -2.237997381628727300, -59.38491726642499202 ) ) ;
#21682 = ORIENTED_EDGE ( 'NONE', *, *, #4497, .T. ) ;
#21683 = EDGE_LOOP ( 'NONE', ( #25474, #16951, #30423, #2075 ) ) ;
#21684 = DIRECTION ( 'NONE',  ( 0.000000000000000000, 0.3420201433259318358, -0.9396926207858125046 ) ) ;
#21685 = VERTEX_POINT ( 'NONE', #29012 ) ;
#21686 = DIRECTION ( 'NONE',  ( 0.000000000000000000, 0.000000000000000000, 1.000000000000000000 ) ) ;
#21687 = EDGE_CURVE ( 'NONE', #24188, #14200, #1942, .T. ) ;
#21688 = CARTESIAN_POINT ( 'NONE',  ( -23.77307140041805411, 14.41181874028064591, 4.999998581000003384 ) ) ;
#21689 = CARTESIAN_POINT ( 'NONE',  ( -25.38146355678814814, 12.59839640969361696, 1.000000000000000888 ) ) ;
#21690 = AXIS2_PLACEMENT_3D ( 'NONE', #23491, #1928, #21121 ) ;
#21691 = CARTESIAN_POINT ( 'NONE',  ( 11.88666889350000133, 2.326897762900000277, 231.9999991140000191 ) ) ;
#21692 = B_SPLINE_CURVE_WITH_KNOTS ( 'NONE', 3,
 ( #9115, #18563, #30379, #4254, #6448, #13849 ),
 .UNSPECIFIED., .F., .F.,
 ( 4, 2, 4 ),
 ( 0.000000000000000000, 0.5000000000000000000, 1.000000000000000000 ),
 .UNSPECIFIED. ) ;
#21693 = DIRECTION ( 'NONE',  ( -1.000000000000000000, 5.665498452320000818E-16, 0.000000000000000000 ) ) ;
#21694 = CARTESIAN_POINT ( 'NONE',  ( -2.365148379994555849, -4.164425085035065699, -5.747565142700007179 ) ) ;
#21695 = CARTESIAN_POINT ( 'NONE',  ( -27.79539923781770128, -0.5057481688779147389, 8.000000000000007105 ) ) ;
#21696 = VERTEX_POINT ( 'NONE', #28707 ) ;
#21697 = CARTESIAN_POINT ( 'NONE',  ( -2.744417411265728912, -4.298957096598221561, -44.10000000002499121 ) ) ;
#21698 = CARTESIAN_POINT ( 'NONE',  ( -4.893571841042398063, 0.6806285466628937408, -20.18909460729999950 ) ) ;
#21699 = CARTESIAN_POINT ( 'NONE',  ( 1.630907769230000026, 5.558498091359999727, 229.6412452697800006 ) ) ;
#21700 = CARTESIAN_POINT ( 'NONE',  ( -17.62526668104891314, 11.76353838341477953, 0.000000000000000000 ) ) ;
#21701 = DIRECTION ( 'NONE',  ( 1.000000000000000000, -0.000000000000000000, 0.000000000000000000 ) ) ;
#21702 = CYLINDRICAL_SURFACE ( 'NONE', #1106, 1.700000000000000178 ) ;
#21703 = CARTESIAN_POINT ( 'NONE',  ( -18.15338440918069907, 19.92139857694655802, 0.007026247000024854472 ) ) ;
#21704 = CARTESIAN_POINT ( 'NONE',  ( -10.69999999999999929, -121.9099955515000033, -31.42347851140000259 ) ) ;
#21705 = DIRECTION ( 'NONE',  ( 5.962915006522623408E-16, 0.4383711467890811231, 0.8987940462991652613 ) ) ;
#21706 = DIRECTION ( 'NONE',  ( 0.000000000000000000, 1.000000000000000000, 0.000000000000000000 ) ) ;
#21707 = EDGE_CURVE ( 'NONE', #11113, #5951, #18794, .T. ) ;
#21708 = DIRECTION ( 'NONE',  ( 0.6941258031311203780, 0.7198537139083029945, 0.000000000000000000 ) ) ;
#21709 = AXIS2_PLACEMENT_3D ( 'NONE', #28467, #23761, #16812 ) ;
#21710 = ORIENTED_EDGE ( 'NONE', *, *, #14693, .F. ) ;
#21711 = CARTESIAN_POINT ( 'NONE',  ( -4.607598934103576127, 1.311847319348407481, -32.23908078970000446 ) ) ;
#21712 = CARTESIAN_POINT ( 'NONE',  ( -7.999999999650483140, -14.85786197181147372, -37.78376919401149792 ) ) ;
#21713 = ORIENTED_EDGE ( 'NONE', *, *, #19604, .T. ) ;
#21714 = CARTESIAN_POINT ( 'NONE',  ( 24.24391315721468487, -12.98049462758916661, 4.325031651118865561 ) ) ;
#21715 = CARTESIAN_POINT ( 'NONE',  ( -2.393684743089945055, 3.904820337558672083, -45.45531229042499888 ) ) ;
#21716 = ORIENTED_EDGE ( 'NONE', *, *, #28276, .T. ) ;
#21717 = VERTEX_POINT ( 'NONE', #2439 ) ;
#21718 = DIRECTION ( 'NONE',  ( 0.000000000000000000, 0.000000000000000000, 1.000000000000000000 ) ) ;
#21719 = ORIENTED_EDGE ( 'NONE', *, *, #3307, .F. ) ;
#21720 = CARTESIAN_POINT ( 'NONE',  ( -0.03526712872449999647, -28.50022367440000082, 223.9000014189999774 ) ) ;
#21721 = EDGE_LOOP ( 'NONE', ( #18254, #10771 ) ) ;
#21722 = CARTESIAN_POINT ( 'NONE',  ( -20.26572724632349320, -21.15151735177849091, 1.000000000000000888 ) ) ;
#21723 = EDGE_CURVE ( 'NONE', #10448, #21281, #20315, .T. ) ;
#21724 = CARTESIAN_POINT ( 'NONE',  ( 25.80996960090668679, 10.85703805089278617, 8.000000000000007105 ) ) ;
#21725 = CARTESIAN_POINT ( 'NONE',  ( 1.013280384041870263, 4.005003068705073943, -35.69999999999998153 ) ) ;
#21726 = CARTESIAN_POINT ( 'NONE',  ( 18.21075248917225409, 19.99999500955443921, -0.6817400023187817348 ) ) ;
#21727 = CARTESIAN_POINT ( 'NONE',  ( -3.937802700299847469, 0.01361741897907296078, -0.6999999999999991784 ) ) ;
#21728 = DIRECTION ( 'NONE',  ( 0.000000000000000000, 0.000000000000000000, -1.000000000000000000 ) ) ;
#21729 = VECTOR ( 'NONE', #15964, 1000.000000000000000 ) ;
#21730 = CARTESIAN_POINT ( 'NONE',  ( 0.000000000000000000, 21.70000000000000284, -45.10000000000000142 ) ) ;
#21731 = CARTESIAN_POINT ( 'NONE',  ( -2.564224011386423641, 5.541743391105337757, -7.731725184300000997 ) ) ;
#21732 = CARTESIAN_POINT ( 'NONE',  ( 2.695668638436317543, -3.937035225248731951, -26.19542313650000054 ) ) ;
#21733 = CARTESIAN_POINT ( 'NONE',  ( 10.82908725742651512, -27.76276047461856322, 193.2171415880000040 ) ) ;
#21734 = CARTESIAN_POINT ( 'NONE',  ( 10.69999999930000101, -27.00000000000000000, -25.39999999999999858 ) ) ;
#21735 = ADVANCED_FACE ( 'NONE', ( #12028 ), #11719, .F. ) ;
#21736 = CARTESIAN_POINT ( 'NONE',  ( 24.61381495442905276, 14.36755986797187923, 6.042472827000016977 ) ) ;
#21737 = CARTESIAN_POINT ( 'NONE',  ( -16.99800964883880638, 12.09718744067793317, -0.6999999999999783062 ) ) ;
#21738 = CARTESIAN_POINT ( 'NONE',  ( 1.666001924310420268, -20.50171922679867720, -27.47981258258537807 ) ) ;
#21739 = CARTESIAN_POINT ( 'NONE',  ( -1.184025259985572953, -4.532227402022651397, -12.55022317840000312 ) ) ;
#21740 = EDGE_CURVE ( 'NONE', #28642, #29484, #21834, .T. ) ;
#21741 = CARTESIAN_POINT ( 'NONE',  ( 0.8794532062938354988, -27.78659480101258694, 6.042323509000024906 ) ) ;
#21742 = FACE_OUTER_BOUND ( 'NONE', #13978, .T. ) ;
#21743 = CARTESIAN_POINT ( 'NONE',  ( -17.49999999969999820, -22.00000000000000000, -31.28675134614999820 ) ) ;
#21744 = VERTEX_POINT ( 'NONE', #28402 ) ;
#21745 = EDGE_CURVE ( 'NONE', #6537, #409, #25959, .T. ) ;
#21746 = CARTESIAN_POINT ( 'NONE',  ( 1.632956991020356519, -28.45346066249067007, 4.791883387999989807 ) ) ;
#21747 = CARTESIAN_POINT ( 'NONE',  ( -27.50000000000000000, 3.367667473009999970E-15, 211.8027756369999679 ) ) ;
#21748 = ORIENTED_EDGE ( 'NONE', *, *, #19458, .T. ) ;
#21749 = B_SPLINE_CURVE_WITH_KNOTS ( 'NONE', 5,
 ( #5372, #14980, #24577, #17479, #3011, #17626 ),
 .UNSPECIFIED., .F., .F.,
 ( 6, 6 ),
 ( 77.28585173369999950, 94.75474465359999954 ),
 .UNSPECIFIED. ) ;
#21750 = CARTESIAN_POINT ( 'NONE',  ( 25.20859211119999799, -13.29584934979999922, 225.3105417090000060 ) ) ;
#21751 = CARTESIAN_POINT ( 'NONE',  ( 23.94466869970572986, 15.45669658583985751, 4.319305385000027364 ) ) ;
#21753 = ORIENTED_EDGE ( 'NONE', *, *, #9046, .F. ) ;
#21752 = CIRCLE ( 'NONE', #6670, 2.999999999999999556 ) ;
#21754 = ORIENTED_EDGE ( 'NONE', *, *, #2792, .T. ) ;
#21755 = B_SPLINE_SURFACE_WITH_KNOTS ( 'NONE', 5, 5, ( 
 ( #14242, #29014, #7460, #24002, #17057, #5096, #24296, #9352, #28560 ),
 ( #9518, #19115, #2746, #21947, #28709, #7155, #16738, #88, #9667 ),
 ( #1153, #15319, #13100, #26811, #17817, #26969, #24920, #3347, #5257 ),
 ( #7765, #10137, #22409, #19581, #14867, #7912, #27123, #15015, #5404 ),
 ( #17516, #24611, #17363, #5556, #27273, #3196, #2894, #15158, #7611 ),
 ( #24458, #27425, #3045, #12954, #22564, #12486, #704, #12636, #19738 ) ),
 .UNSPECIFIED., .F., .F., .F.,
 ( 6, 6 ),
 ( 6, 3, 6 ),
 ( 0.000000000000000000, 23.96001935709999842 ),
 ( 8.011061266649999624, 8.811950030160000225, 9.612838793659999936 ),
 .UNSPECIFIED. ) ;
#21756 = VERTEX_POINT ( 'NONE', #12176 ) ;
#21757 =( NAMED_UNIT ( * ) SI_UNIT ( $, .STERADIAN. ) SOLID_ANGLE_UNIT ( ) );
#21758 = ORIENTED_EDGE ( 'NONE', *, *, #7521, .F. ) ;
#21759 = CARTESIAN_POINT ( 'NONE',  ( -14.89999999913999851, -22.00000000000000000, -25.51324865424999899 ) ) ;
#21760 = EDGE_CURVE ( 'NONE', #7767, #2713, #7312, .T. ) ;
#21761 = CARTESIAN_POINT ( 'NONE',  ( -5.361385120500000490, 31.61859227569999931, 229.0000000000000000 ) ) ;
#21762 = CARTESIAN_POINT ( 'NONE',  ( 17.18658402238548533, 9.900182044515950963, -0.6999999999999784173 ) ) ;
#21763 = ORIENTED_EDGE ( 'NONE', *, *, #20256, .F. ) ;
#21764 = CARTESIAN_POINT ( 'NONE',  ( -25.45799949038170240, 12.81261085762170815, 5.208434320000010942 ) ) ;
#21765 = DIRECTION ( 'NONE',  ( 0.000000000000000000, 0.000000000000000000, -1.000000000000000000 ) ) ;
#21766 = CARTESIAN_POINT ( 'NONE',  ( -17.20085693451561681, -32.00000000000027711, -26.04892971879526442 ) ) ;
#21767 = CARTESIAN_POINT ( 'NONE',  ( 24.32472724076343695, -13.45989056521276872, 6.099998581000020792 ) ) ;
#21768 = CARTESIAN_POINT ( 'NONE',  ( 3.843992482562140989, -2.627063339010873300, -0.6999999999867967393 ) ) ;
#21769 = ORIENTED_EDGE ( 'NONE', *, *, #20885, .T. ) ;
#21770 = ADVANCED_FACE ( 'NONE', ( #2290 ), #16735, .T. ) ;
#21771 = LINE ( 'NONE', #17754, #16512 ) ;
#21772 = CARTESIAN_POINT ( 'NONE',  ( -4.278952157217901231, -0.8066629416743145153, -16.09949426530000238 ) ) ;
#21773 = DIRECTION ( 'NONE',  ( -1.000000000000000000, 0.000000000000000000, 0.000000000000000000 ) ) ;
#21774 = DIRECTION ( 'NONE',  ( -4.428977494234582379E-12, -0.8987940462991651502, 0.4383711467890810676 ) ) ;
#21775 = CIRCLE ( 'NONE', #23280, 2.100000000000000089 ) ;
#21776 = CARTESIAN_POINT ( 'NONE',  ( -12.31092893605830696, -29.21179069622078117, -32.89652473824072842 ) ) ;
#21777 = CARTESIAN_POINT ( 'NONE',  ( 12.84292916307208543, 21.69999999994266915, -69.49962415800092685 ) ) ;
#21778 = CARTESIAN_POINT ( 'NONE',  ( 28.49528339128749366, 0.5184828350247212558, 1.000000000000000888 ) ) ;
#21779 = DIRECTION ( 'NONE',  ( 0.000000000000000000, 0.000000000000000000, -1.000000000000000000 ) ) ;
#21780 = CARTESIAN_POINT ( 'NONE',  ( 0.5814717383643280835, -5.541158915576414046, -67.77495035202500162 ) ) ;
#21781 = EDGE_CURVE ( 'NONE', #28642, #19036, #8659, .T. ) ;
#21782 = CARTESIAN_POINT ( 'NONE',  ( 24.58947386300000204, 13.65571127169999954, 229.7313205199999686 ) ) ;
#21783 = CARTESIAN_POINT ( 'NONE',  ( -7.957586915840000330, 16.45834648369999798, 230.6999999999999886 ) ) ;
#21784 = ORIENTED_EDGE ( 'NONE', *, *, #10020, .T. ) ;
#21785 = DIRECTION ( 'NONE',  ( 0.000000000000000000, -1.000000000000000000, 0.000000000000000000 ) ) ;
#21786 = B_SPLINE_CURVE_WITH_KNOTS ( 'NONE', 3,
 ( #6198, #28221, #25723, #4158, #13277, #1958, #3845, #1492, #11236, #20995, #18469, #15635, #8707, #30598, #25411, #18313, #11086, #4316 ),
 .UNSPECIFIED., .F., .F.,
 ( 4, 2, 2, 2, 2, 1, 1, 2, 2, 4 ),
 ( 0.000000000000000000, 0.1250000000000101585, 0.1875000000000161815, 0.2500000000000222045, 0.3750000000000344724, 0.4375000000000404676, 0.4687500000000434097, 0.4843750000000421885, 0.5000000000000409672, 1.000000000000000000 ),
 .UNSPECIFIED. ) ;
#21787 = DIRECTION ( 'NONE',  ( 7.759996349202911684E-13, 0.9341647027306021478, 0.3568421334038983650 ) ) ;
#21788 = CARTESIAN_POINT ( 'NONE',  ( 9.999999999941215023, -27.47344925854523368, -16.99201750777429965 ) ) ;
#21789 = VERTEX_POINT ( 'NONE', #26657 ) ;
#21790 = CONICAL_SURFACE ( 'NONE', #28315, 12.22526471199999598, 1.243158134259999770 ) ;
#21791 = CARTESIAN_POINT ( 'NONE',  ( 1.609514238142041975, 3.181902231760902477, -88.52261276241718235 ) ) ;
#21792 = CIRCLE ( 'NONE', #25820, 3.199999983039998774 ) ;
#21793 = ORIENTED_EDGE ( 'NONE', *, *, #23384, .T. ) ;
#21794 = FACE_OUTER_BOUND ( 'NONE', #28517, .T. ) ;
#21795 = EDGE_CURVE ( 'NONE', #7318, #4812, #15812, .T. ) ;
#21796 = CARTESIAN_POINT ( 'NONE',  ( -0.9992285280876744835, -5.354791469827751449, -68.70745670422499529 ) ) ;
#21797 = EDGE_LOOP ( 'NONE', ( #5643, #15018, #20971, #8939 ) ) ;
#21798 = CARTESIAN_POINT ( 'NONE',  ( -4.215937884789282108, -1.105999120962573246, -25.54656121680000425 ) ) ;
#21799 = CARTESIAN_POINT ( 'NONE',  ( 10.69999999989999928, -45.00000000000000000, -7.274962170899998526 ) ) ;
#21800 = EDGE_CURVE ( 'NONE', #2111, #1677, #2891, .T. ) ;
#21801 = CARTESIAN_POINT ( 'NONE',  ( -2.571638601809290936, 3.775240214263654526, -48.05391720702499470 ) ) ;
#21802 = CARTESIAN_POINT ( 'NONE',  ( 8.700000000242635423, -24.33830582822444200, -26.96109716006106893 ) ) ;
#21803 = CARTESIAN_POINT ( 'NONE',  ( 1.100000000000000089, -27.47799119300000115, 225.0000000000000000 ) ) ;
#21804 = CARTESIAN_POINT ( 'NONE',  ( 8.700000000277906764, -15.94902145836247342, -35.53273252485295330 ) ) ;
#21805 = CARTESIAN_POINT ( 'NONE',  ( 0.000000000000000000, 0.000000000000000000, 36.39444872359999295 ) ) ;
#21806 = B_SPLINE_CURVE_WITH_KNOTS ( 'NONE', 3,
 ( #9232, #25779, #28440, #4211, #6872, #30174, #25629, #9083, #23111, #28279, #27971, #11608, #4527, #4368, #16474, #30338, #18678, #23260, #23583, #16014, #2017, #3902, #4059, #8604, #26088, #21205 ),
 .UNSPECIFIED., .F., .F.,
 ( 4, 2, 2, 1, 1, 2, 2, 2, 2, 2, 1, 1, 2, 2, 4 ),
 ( 0.000000000000000000, 0.1249999999999832911, 0.1874999999999727440, 0.2187499999999673594, 0.2343749999999648337, 0.2421874999999636124, 0.2499999999999623634, 0.4999999999999558131, 0.6249999999999522604, 0.6874999999999497069, 0.7187499999999472644, 0.7343749999999473754, 0.7421874999999487077, 0.7499999999999501510, 1.000000000000000000 ),
 .UNSPECIFIED. ) ;
#21807 = AXIS2_PLACEMENT_3D ( 'NONE', #30293, #18331, #7150 ) ;
#21808 = CARTESIAN_POINT ( 'NONE',  ( -17.38167868480947931, -22.00021832957186163, -26.99851627150150080 ) ) ;
#21809 = ORIENTED_EDGE ( 'NONE', *, *, #2101, .T. ) ;
#21810 = CARTESIAN_POINT ( 'NONE',  ( -15.86234340635861173, 10.46359668131463216, -1.384526174263989162E-13 ) ) ;
#21811 = CARTESIAN_POINT ( 'NONE',  ( -9.000000000000000000, 20.99999999999999645, -64.10000000019999788 ) ) ;
#21812 = CIRCLE ( 'NONE', #17255, 2.999999999999999556 ) ;
#21813 = VECTOR ( 'NONE', #12914, 1000.000000000000000 ) ;
#21814 = CARTESIAN_POINT ( 'NONE',  ( -9.117807398470000990, -8.314605678609998662, 232.6627643349999914 ) ) ;
#21815 = CARTESIAN_POINT ( 'NONE',  ( -26.95773186790000153, 8.656139628340000058, 227.5999999999999943 ) ) ;
#21816 = CARTESIAN_POINT ( 'NONE',  ( -12.30800288698999978, -29.39779533043000015, -32.78913491261000246 ) ) ;
#21817 = CIRCLE ( 'NONE', #18773, 27.50000000000000000 ) ;
#21818 = CARTESIAN_POINT ( 'NONE',  ( -4.000000000000000000, -31.83942647549183746, -80.46693306215520636 ) ) ;
#21819 = TOROIDAL_SURFACE ( 'NONE', #13772, 29.80000000000000071, 3.000000000000000000 ) ;
#21820 = CARTESIAN_POINT ( 'NONE',  ( 24.60666973299075977, -12.93650480179744200, 224.8530246344855357 ) ) ;
#21821 = CARTESIAN_POINT ( 'NONE',  ( -4.785279987111795030, -31.71089578012187360, 0.7595836940000044724 ) ) ;
#21822 = CARTESIAN_POINT ( 'NONE',  ( -6.394884621839999216E-14, -26.80000000000000071, 226.0999999999999943 ) ) ;
#21823 = DIRECTION ( 'NONE',  ( 1.445602896647338719E-15, 1.000000000000000000, 0.000000000000000000 ) ) ;
#21824 = PLANE ( 'NONE',  #5571 ) ;
#21825 = CARTESIAN_POINT ( 'NONE',  ( 10.33059233208003214, -6.304462385806647973, 232.0000002394077399 ) ) ;
#21826 = CARTESIAN_POINT ( 'NONE',  ( 17.14656078602323319, -7.900182044548062166, -0.6999999999999784173 ) ) ;
#21827 = CARTESIAN_POINT ( 'NONE',  ( 24.75645985066559263, 14.12045945726143970, 5.901294549000013490 ) ) ;
#21828 = VERTEX_POINT ( 'NONE', #15013 ) ;
#21829 = CARTESIAN_POINT ( 'NONE',  ( 19.80526555972147307, 19.50877392102524155, 2.200000000000007283 ) ) ;
#21830 = SHAPE_REPRESENTATION_RELATIONSHIP ( 'NONE' , 'NONE' ,  #8955, #6893 ) ;
#21831 = ORIENTED_EDGE ( 'NONE', *, *, #2727, .T. ) ;
#21832 = CARTESIAN_POINT ( 'NONE',  ( 24.55535052759999814, -13.03386662210000146, 225.5069763079999916 ) ) ;
#21833 = VECTOR ( 'NONE', #23179, 999.9999999999998863 ) ;
#21834 = B_SPLINE_CURVE_WITH_KNOTS ( 'NONE', 1,
 ( #23845, #18952 ),
 .UNSPECIFIED., .F., .F.,
 ( 2, 2 ),
 ( -3.500000000000000000, 3.500000000000000000 ),
 .UNSPECIFIED. ) ;
#21835 = CARTESIAN_POINT ( 'NONE',  ( -5.325262776966551037, 2.643762325382846612, -56.79877225282499609 ) ) ;
#21836 = AXIS2_PLACEMENT_3D ( 'NONE', #16441, #7002, #11570 ) ;
#21837 = ORIENTED_EDGE ( 'NONE', *, *, #17750, .T. ) ;
#21838 = AXIS2_PLACEMENT_3D ( 'NONE', #11996, #28519, #23811 ) ;
#21839 = AXIS2_PLACEMENT_3D ( 'NONE', #3890, #1539, #14812 ) ;
#21840 = EDGE_CURVE ( 'NONE', #4684, #12935, #19736, .T. ) ;
#21841 = TOROIDAL_SURFACE ( 'NONE', #9240, 29.80000000000000071, 3.000000000000000000 ) ;
#21842 = EDGE_LOOP ( 'NONE', ( #16150, #6651, #3243, #25978 ) ) ;
#21843 = CARTESIAN_POINT ( 'NONE',  ( 8.700000000232995134, -27.30967745505199673, -25.39025505876632494 ) ) ;
#21844 = EDGE_CURVE ( 'NONE', #14134, #27320, #12635, .T. ) ;
#21845 = ORIENTED_EDGE ( 'NONE', *, *, #17326, .F. ) ;
#21846 = CARTESIAN_POINT ( 'NONE',  ( 8.000000000248304488, -25.92947504235655032, -31.20249033167290165 ) ) ;
#21847 = CARTESIAN_POINT ( 'NONE',  ( -24.37165444408190851, 14.77472139917419369, 4.999998581000003384 ) ) ;
#21848 = CARTESIAN_POINT ( 'NONE',  ( 3.686970300939999667, 0.4978338539504151838, -70.82548838946271985 ) ) ;
#21849 = B_SPLINE_CURVE_WITH_KNOTS ( 'NONE', 5,
 ( #17602, #29568, #1250, #10846, #22958, #20432, #27363, #15703, #1406, #30029, #18059, #8460 ),
 .UNSPECIFIED., .F., .F.,
 ( 6, 3, 3, 6 ),
 ( 1.224410003600000074, 1.456394985740000037, 2.184590823429999773, 2.448622002460000058 ),
 .UNSPECIFIED. ) ;
#21851 = CARTESIAN_POINT ( 'NONE',  ( 9.738910687886868089, -24.96785170200598358, 186.7828584120000244 ) ) ;
#21850 = B_SPLINE_CURVE_WITH_KNOTS ( 'NONE', 3,
 ( #29806, #13442, #22735, #8394, #8239, #13126 ),
 .UNSPECIFIED., .F., .F.,
 ( 4, 2, 4 ),
 ( 0.000000000000000000, 0.5000000000000000000, 1.000000000000000000 ),
 .UNSPECIFIED. ) ;
#21852 = APPLICATION_CONTEXT ( 'automotive_design' ) ;
#21853 = LINE ( 'NONE', #7055, #24007 ) ;
#21854 = CARTESIAN_POINT ( 'NONE',  ( 5.459923716313909381, 2.263110678531865094, -10.49261350019999561 ) ) ;
#21855 = CARTESIAN_POINT ( 'NONE',  ( 27.29823224880000154, -6.039613253960000872E-14, 230.6577119970000069 ) ) ;
#21856 = VERTEX_POINT ( 'NONE', #8062 ) ;
#21857 = CARTESIAN_POINT ( 'NONE',  ( 0.1973057990048258659, -5.030289273761288982, -44.10000000002499121 ) ) ;
#21858 = CARTESIAN_POINT ( 'NONE',  ( -24.97472003774791816, -13.73006752753317450, 4.791638085000021974 ) ) ;
#21859 = CARTESIAN_POINT ( 'NONE',  ( 0.6713911862884133219, -5.438992117826878747, -19.37054674910000074 ) ) ;
#21860 = CARTESIAN_POINT ( 'NONE',  ( -0.9498500758684573775, -27.78406401609443321, 225.5583478121612870 ) ) ;
#21861 = CARTESIAN_POINT ( 'NONE',  ( 0.9131176273315529945, -27.48533474125000353, 225.6425104791852618 ) ) ;
#21862 = B_SPLINE_SURFACE_WITH_KNOTS ( 'NONE', 5, 1, ( 
 ( #26930, #12296 ),
 ( #4907, #12442 ),
 ( #2851, #10249 ),
 ( #5205, #29275 ),
 ( #5516, #7269 ),
 ( #26464, #21594 ),
 ( #43, #24108 ),
 ( #26767, #14820 ),
 ( #7718, #17321 ),
 ( #9938, #7418 ),
 ( #24417, #22060 ),
 ( #16858, #2548 ),
 ( #9623, #21909 ),
 ( #7569, #19224 ),
 ( #12135, #511 ) ),
 .UNSPECIFIED., .F., .F., .F.,
 ( 6, 3, 3, 3, 6 ),
 ( 2, 2 ),
 ( 0.000000000000000000, 0.5239010162240000934, 1.047802032450000143, 1.571703048670000102, 1.746336720750000016 ),
 ( -0.7000000000009999335, 2.556017480449999863E-06 ),
 .UNSPECIFIED. ) ;
#21863 = VECTOR ( 'NONE', #16627, 1000.000000000000000 ) ;
#21864 = CARTESIAN_POINT ( 'NONE',  ( -24.60699806910000120, -12.93667933180000063, 224.8957833819999621 ) ) ;
#21865 = CIRCLE ( 'NONE', #22837, 4.100000000000000533 ) ;
#21866 = CARTESIAN_POINT ( 'NONE',  ( -15.73624015604650772, 11.16458205270512138, -0.6999999999999783062 ) ) ;
#21867 = CARTESIAN_POINT ( 'NONE',  ( 3.001777156698443250, -4.698362801289899693, -43.08966640442498885 ) ) ;
#21868 = CARTESIAN_POINT ( 'NONE',  ( -10.69999999999999929, -121.2050733649000023, -31.31359859269999646 ) ) ;
#21869 = CARTESIAN_POINT ( 'NONE',  ( -24.36725163763869162, -13.38201776504303986, 4.999998581000003384 ) ) ;
#21870 = CARTESIAN_POINT ( 'NONE',  ( -24.41841039498785193, -14.69667350221323865, 6.099998581000020792 ) ) ;
#21871 = CARTESIAN_POINT ( 'NONE',  ( -24.06944413539999772, 13.35197612260000000, 230.0000000000000000 ) ) ;
#21872 = EDGE_CURVE ( 'NONE', #5618, #20193, #5554, .T. ) ;
#21873 = LINE ( 'NONE', #19504, #18770 ) ;
#21875 = ORIENTED_EDGE ( 'NONE', *, *, #25863, .F. ) ;
#21874 = PRESENTATION_LAYER_ASSIGNMENT (  '', '', ( #272 ) ) ;
#21876 = CARTESIAN_POINT ( 'NONE',  ( 3.157381476932436648, -2.999772911539579034, -30.55126389019999777 ) ) ;
#21877 = AXIS2_PLACEMENT_3D ( 'NONE', #16425, #1650, #2114 ) ;
#21878 = CARTESIAN_POINT ( 'NONE',  ( 10.69999999999999929, -120.5233595624000174, -31.26042064949999855 ) ) ;
#21879 = MECHANICAL_DESIGN_GEOMETRIC_PRESENTATION_REPRESENTATION (  '', ( #278 ), #2754 ) ;
#21880 = ORIENTED_EDGE ( 'NONE', *, *, #28848, .F. ) ;
#21881 = DIRECTION ( 'NONE',  ( -0.8366600265365546907, -0.4922897737059920287, 0.2401057656541278063 ) ) ;
#21882 = CARTESIAN_POINT ( 'NONE',  ( -4.251243323665415907, -4.132078999800212316, -47.68083066912500101 ) ) ;
#21883 = ORIENTED_EDGE ( 'NONE', *, *, #17697, .F. ) ;
#21884 = EDGE_LOOP ( 'NONE', ( #27739, #11223, #4130, #27701 ) ) ;
#21885 = FILL_AREA_STYLE_COLOUR ( '', #12839 ) ;
#21886 = ORIENTED_EDGE ( 'NONE', *, *, #14447, .T. ) ;
#21887 = CARTESIAN_POINT ( 'NONE',  ( -7.999999999728448330, -26.04217715522926824, -25.54542481146843613 ) ) ;
#21888 = ORIENTED_EDGE ( 'NONE', *, *, #26679, .T. ) ;
#21889 = DIRECTION ( 'NONE',  ( 1.000000000000000000, -1.224606353819999582E-16, 0.000000000000000000 ) ) ;
#21890 = CARTESIAN_POINT ( 'NONE',  ( -5.191868678539384163, -9.773567673788013721, -36.05008753148776179 ) ) ;
#21891 = DIRECTION ( 'NONE',  ( 0.000000000000000000, 0.000000000000000000, -1.000000000000000000 ) ) ;
#21892 = CARTESIAN_POINT ( 'NONE',  ( 0.8241976871332568066, 4.093728295075581336, -35.70000000000000284 ) ) ;
#21893 = FACE_OUTER_BOUND ( 'NONE', #7113, .T. ) ;
#21894 = CARTESIAN_POINT ( 'NONE',  ( -24.30808044443811156, 13.48997716914403533, 6.099998581000020792 ) ) ;
#21895 = CARTESIAN_POINT ( 'NONE',  ( -22.69912944659995446, -14.24746549235085524, 5.486606152533540559 ) ) ;
#21896 = CARTESIAN_POINT ( 'NONE',  ( -23.58694728389455264, -14.71452256581467388, 224.4414045756103633 ) ) ;
#21897 = EDGE_LOOP ( 'NONE', ( #4886, #30560, #23971, #3463, #31098, #30599, #11185, #6984, #22635, #21461 ) ) ;
#21898 = CARTESIAN_POINT ( 'NONE',  ( 4.880902371519058036, -3.592936783560450653, -8.972776792900004850 ) ) ;
#21899 = CARTESIAN_POINT ( 'NONE',  ( 0.7775660777938816492, 5.461502024334397909, -28.00600711720000291 ) ) ;
#21900 = CARTESIAN_POINT ( 'NONE',  ( 2.347741120694188055, -2.634769306325225102, 0.000000000000000000 ) ) ;
#21901 = AXIS2_PLACEMENT_3D ( 'NONE', #12726, #940, #7998 ) ;
#21902 = CARTESIAN_POINT ( 'NONE',  ( 17.83928249670000099, 20.00000000010000178, -0.6999999995999997005 ) ) ;
#21903 = CARTESIAN_POINT ( 'NONE',  ( 24.45473033137484720, 14.63622297804190175, 6.098654221000004760 ) ) ;
#21904 =( NAMED_UNIT ( * ) SI_UNIT ( $, .STERADIAN. ) SOLID_ANGLE_UNIT ( ) );
#21905 = CARTESIAN_POINT ( 'NONE',  ( 3.938336462418420059, -27.21777852796476793, 20.19589729288204083 ) ) ;
#21906 = CARTESIAN_POINT ( 'NONE',  ( -2.150134890876696847, -3.785840986416655340, -6.685065142700001850 ) ) ;
#21907 = EDGE_CURVE ( 'NONE', #17565, #3121, #10774, .T. ) ;
#21908 = CARTESIAN_POINT ( 'NONE',  ( 1.568292632109252738, -27.75603058367127574, 5.310199493000017590 ) ) ;
#21909 = CARTESIAN_POINT ( 'NONE',  ( -23.85408962131194954, -14.27673465746016213, 3.901342939999996595 ) ) ;
#21910 = CARTESIAN_POINT ( 'NONE',  ( 0.7404173758759277080, -3.499814327641340927, 230.7917081009901210 ) ) ;
#21911 = VERTEX_POINT ( 'NONE', #10293 ) ;
#21912 = EDGE_CURVE ( 'NONE', #24188, #1475, #1551, .T. ) ;
#21913 = CARTESIAN_POINT ( 'NONE',  ( 0.000000000000000000, 0.000000000000000000, 140.0000000000000000 ) ) ;
#21914 = CARTESIAN_POINT ( 'NONE',  ( 16.59519732816799475, 11.95092772887203836, -4.336808689942017243E-16 ) ) ;
#21915 = EDGE_LOOP ( 'NONE', ( #20921, #29867, #20631, #715 ) ) ;
#21916 = B_SPLINE_CURVE_WITH_KNOTS ( 'NONE', 3,
 ( #27499, #12721, #27201, #22791, #5640, #19964 ),
 .UNSPECIFIED., .F., .F.,
 ( 4, 2, 4 ),
 ( 0.000000000000000000, 0.5000000000000000000, 1.000000000000000000 ),
 .UNSPECIFIED. ) ;
#21917 = DIRECTION ( 'NONE',  ( 0.000000000000000000, 0.000000000000000000, 1.000000000000000000 ) ) ;
#21918 = CARTESIAN_POINT ( 'NONE',  ( 7.999999999489469715, -115.5185322950121929, 21.06548255655121338 ) ) ;
#21919 = VERTEX_POINT ( 'NONE', #29474 ) ;
#21920 = CARTESIAN_POINT ( 'NONE',  ( -4.859832392515191835, 0.02388181653997099169, -44.10000000002499121 ) ) ;
#21921 = EDGE_LOOP ( 'NONE', ( #27860, #3472, #7426, #26506, #24757, #3124, #12375, #29963, #18102, #14567 ) ) ;
#21922 = VERTEX_POINT ( 'NONE', #17812 ) ;
#21923 = ORIENTED_EDGE ( 'NONE', *, *, #8309, .T. ) ;
#21924 = CARTESIAN_POINT ( 'NONE',  ( 26.80000000000000071, 7.105427357599999217E-15, 36.78285841090000474 ) ) ;
#21925 = DIRECTION ( 'NONE',  ( 1.181300906760215537E-13, 0.9986295347541825906, 0.05233595625040957794 ) ) ;
#21926 = EDGE_CURVE ( 'NONE', #6451, #23742, #29886, .T. ) ;
#21927 = CARTESIAN_POINT ( 'NONE',  ( -7.999999999683591767, -17.13607329101123611, -33.32374753170036286 ) ) ;
#21928 = EDGE_LOOP ( 'NONE', ( #16639, #25791, #5104, #24466, #15615 ) ) ;
#21929 = DIRECTION ( 'NONE',  ( -0.5000000000001894040, 0.8660254037843291286, 0.000000000000000000 ) ) ;
#21930 = CARTESIAN_POINT ( 'NONE',  ( -17.48420900742980422, -31.99983740011833788, -27.95389062477287823 ) ) ;
#21931 = CARTESIAN_POINT ( 'NONE',  ( 10.69999999992358575, -25.00000000000000711, -8.544674958192336689 ) ) ;
#21932 = EDGE_LOOP ( 'NONE', ( #26481, #12420, #22297, #21023, #28325 ) ) ;
#21933 = CARTESIAN_POINT ( 'NONE',  ( 4.180014548479816128, -1.737364395512316362, -16.93372516810000405 ) ) ;
#21934 = CARTESIAN_POINT ( 'NONE',  ( 18.24356172924623820, -9.267172192657799457, -0.6999999999999784173 ) ) ;
#21935 = CARTESIAN_POINT ( 'NONE',  ( 0.000000000000000000, 0.000000000000000000, 115.0000000000000000 ) ) ;
#21936 = CARTESIAN_POINT ( 'NONE',  ( 4.638687372182204172, -18.11047956030077799, -28.64609809500778326 ) ) ;
#21937 = CARTESIAN_POINT ( 'NONE',  ( 0.5537481963838299936, -28.49486543565701169, 3.899998581000013509 ) ) ;
#21938 = LINE ( 'NONE', #22090, #14808 ) ;
#21939 = DIRECTION ( 'NONE',  ( 0.000000000000000000, -0.9128796883888953273, 0.4082287037029528887 ) ) ;
#21940 = DIRECTION ( 'NONE',  ( 0.000000000000000000, -1.000000000000000000, 0.000000000000000000 ) ) ;
#21941 = LINE ( 'NONE', #699, #8729 ) ;
#21942 = DIRECTION ( 'NONE',  ( 0.000000000000000000, 0.000000000000000000, 1.000000000000000000 ) ) ;
#21943 = ORIENTED_EDGE ( 'NONE', *, *, #2908, .F. ) ;
#21944 = CARTESIAN_POINT ( 'NONE',  ( 2.776548632478544665, -3.583402058917912747, -52.10430438132500086 ) ) ;
#21945 = CARTESIAN_POINT ( 'NONE',  ( 26.79556473285982321, 0.4875557887249620803, 0.000000000000000000 ) ) ;
#21946 = EDGE_CURVE ( 'NONE', #17896, #931, #16912, .T. ) ;
#21947 = CARTESIAN_POINT ( 'NONE',  ( -27.32958467830413340, 4.204436669847241070, 0.08279779300002232389 ) ) ;
#21948 = CARTESIAN_POINT ( 'NONE',  ( -3.151262587278881089, -4.016474153426608851, -68.10000000002501963 ) ) ;
#21949 = EDGE_LOOP ( 'NONE', ( #28222, #9689, #9566, #3554 ) ) ;
#21950 = CARTESIAN_POINT ( 'NONE',  ( 10.69999999996928963, -24.00000000000000711, -28.79379052057399946 ) ) ;
#21951 = B_SPLINE_SURFACE_WITH_KNOTS ( 'NONE', 5, 1, ( 
 ( #19288, #10427 ),
 ( #2458, #10578 ),
 ( #20173, #7891 ),
 ( #17642, #20019 ),
 ( #17498, #28881 ),
 ( #26523, #7172 ),
 ( #26217, #4654 ),
 ( #21655, #16915 ),
 ( #9535, #7330 ),
 ( #24744, #27255 ),
 ( #104, #12934 ),
 ( #24904, #16760 ),
 ( #21494, #19877 ),
 ( #11891, #14262 ),
 ( #12050, #4963 ) ),
 .UNSPECIFIED., .F., .F., .F.,
 ( 6, 3, 3, 3, 6 ),
 ( 2, 2 ),
 ( 0.000000000000000000, 0.5238999881929999880, 1.047799976380000109, 1.571699964580000053, 1.746333293980000034 ),
 ( -0.7000000000009999335, 2.555864960449999711E-06 ),
 .UNSPECIFIED. ) ;
#21952 = ORIENTED_EDGE ( 'NONE', *, *, #17662, .T. ) ;
#21953 = CARTESIAN_POINT ( 'NONE',  ( 0.000000000000000000, -1.776356839399999804E-15, 227.6412452697800006 ) ) ;
#21954 = CARTESIAN_POINT ( 'NONE',  ( -4.475180390489594373, -2.644424941261572126, -69.07382590962501467 ) ) ;
#21955 = EDGE_CURVE ( 'NONE', #26866, #18702, #30481, .T. ) ;
#21956 = ORIENTED_EDGE ( 'NONE', *, *, #29890, .F. ) ;
#21957 = CARTESIAN_POINT ( 'NONE',  ( 0.1047326596782457986, -5.131546142535936994, -25.35638333260000010 ) ) ;
#21958 = DIRECTION ( 'NONE',  ( 0.000000000000000000, 0.000000000000000000, -1.000000000000000000 ) ) ;
#21959 = ADVANCED_FACE ( 'NONE', ( #3043 ), #19580, .F. ) ;
#21960 = EDGE_CURVE ( 'NONE', #2058, #22456, #15807, .T. ) ;
#21961 = CARTESIAN_POINT ( 'NONE',  ( 1.082264403401735020, -4.420062499635217357, -64.70397119102501904 ) ) ;
#21962 = CARTESIAN_POINT ( 'NONE',  ( 1.976074114793839431, -0.3084332875059770385, 226.6412452697749984 ) ) ;
#21963 = CARTESIAN_POINT ( 'NONE',  ( 17.85685193652881964, -9.868837085878030990, -0.6999999999999784173 ) ) ;
#21964 = CARTESIAN_POINT ( 'NONE',  ( -26.80000000069999899, 3.281945028329999726E-15, 193.2171415869999862 ) ) ;
#21965 = UNCERTAINTY_MEASURE_WITH_UNIT (LENGTH_MEASURE( 1.000000000000000082E-05 ), #17632, 'distance_accuracy_value', 'NONE');
#21966 = ADVANCED_FACE ( 'NONE', ( #17658 ), #24918, .F. ) ;
#21967 = CARTESIAN_POINT ( 'NONE',  ( 8.700000000296066460, -14.31621543018684761, -40.15015555144486115 ) ) ;
#21968 = CARTESIAN_POINT ( 'NONE',  ( -17.45889703378724178, -22.00009059174836423, -27.51494980511629507 ) ) ;
#21969 = ORIENTED_EDGE ( 'NONE', *, *, #3615, .F. ) ;
#21970 = CARTESIAN_POINT ( 'NONE',  ( 3.333579493031019858, 1.225759174641957827, 227.6757455870668423 ) ) ;
#21971 = CARTESIAN_POINT ( 'NONE',  ( -7.999999999681902452, -14.92844969907143771, -33.25053330396754347 ) ) ;
#21972 = CARTESIAN_POINT ( 'NONE',  ( -8.404590197819999275, 8.972803037040000262, 232.6627643349999914 ) ) ;
#21973 = CARTESIAN_POINT ( 'NONE',  ( -14.39562240800000126, -9.581487064249998298, 225.0000000000000000 ) ) ;
#21974 = CARTESIAN_POINT ( 'NONE',  ( -11.07235429843649754, 4.885731407866478193, 232.0000000000049170 ) ) ;
#21975 = CARTESIAN_POINT ( 'NONE',  ( 10.69999999998643325, -128.7641386039167060, -36.38932005418158866 ) ) ;
#21976 = CARTESIAN_POINT ( 'NONE',  ( -17.46782121558967660, -8.097265036127433646, 0.000000000000000000 ) ) ;
#21977 = EDGE_CURVE ( 'NONE', #21789, #1557, #5707, .T. ) ;
#21978 = CARTESIAN_POINT ( 'NONE',  ( 14.12863464165936378, -27.12057300290972250, -0.5592437529999827461 ) ) ;
#21979 = CARTESIAN_POINT ( 'NONE',  ( -24.83272648880584654, 12.49791454310039640, 4.791562840999991302 ) ) ;
#21980 = CARTESIAN_POINT ( 'NONE',  ( -7.999999999675157625, -13.69798478930254149, -34.44157303844319529 ) ) ;
#21981 = AXIS2_PLACEMENT_3D ( 'NONE', #15331, #30116, #3358 ) ;
#21982 = EDGE_CURVE ( 'NONE', #16634, #1011, #14316, .T. ) ;
#21983 = TOROIDAL_SURFACE ( 'NONE', #12421, 30.50000000000000000, 3.000000000000000000 ) ;
#21984 = CARTESIAN_POINT ( 'NONE',  ( -24.28117756995407106, -12.91036561245694081, 5.556164354347067125 ) ) ;
#21985 = DIRECTION ( 'NONE',  ( 1.000000000000000000, -0.000000000000000000, 0.000000000000000000 ) ) ;
#21986 = ORIENTED_EDGE ( 'NONE', *, *, #18040, .F. ) ;
#21987 = ADVANCED_FACE ( 'NONE', ( #30098 ), #20815, .F. ) ;
#21988 = CARTESIAN_POINT ( 'NONE',  ( 10.99289321870000080, -24.65831413369999936, -1.692893218799999877 ) ) ;
#21989 = DIRECTION ( 'NONE',  ( 0.000000000000000000, -0.3420201433259318358, 0.9396926207858125046 ) ) ;
#21990 = CARTESIAN_POINT ( 'NONE',  ( -5.463799992266447525, -1.435916617982112342, -56.45102360502500005 ) ) ;
#21991 = ORIENTED_EDGE ( 'NONE', *, *, #2583, .F. ) ;
#21992 = B_SPLINE_CURVE_WITH_KNOTS ( 'NONE', 5,
 ( #9505, #28700, #17048, #26649, #7603, #5088 ),
 .UNSPECIFIED., .F., .F.,
 ( 6, 6 ),
 ( 0.000000000000000000, 2.319814960330000009 ),
 .UNSPECIFIED. ) ;
#21993 = ORIENTED_EDGE ( 'NONE', *, *, #11254, .F. ) ;
#21994 = AXIS2_PLACEMENT_3D ( 'NONE', #27828, #5652, #8465 ) ;
#21995 = FACE_OUTER_BOUND ( 'NONE', #9008, .T. ) ;
#21996 = ORIENTED_EDGE ( 'NONE', *, *, #17377, .F. ) ;
#21997 = EDGE_LOOP ( 'NONE', ( #21190, #22992, #15850, #12922 ) ) ;
#21998 = CARTESIAN_POINT ( 'NONE',  ( 8.000000000250929943, -24.65281347431490033, -30.30937277425890386 ) ) ;
#21999 = PLANE ( 'NONE',  #29571 ) ;
#22000 = CARTESIAN_POINT ( 'NONE',  ( -19.80535357367646654, 19.50875577052770993, 3.799999999999998046 ) ) ;
#22001 = CIRCLE ( 'NONE', #5411, 3.200000000000002398 ) ;
#22002 = LINE ( 'NONE', #12235, #28896 ) ;
#22003 = DIRECTION ( 'NONE',  ( 1.000000000000000000, -0.000000000000000000, -2.257150022439999944E-12 ) ) ;
#22004 = CARTESIAN_POINT ( 'NONE',  ( 1.888485499342153151, 5.773790730162923879, -11.07047964830000453 ) ) ;
#22005 = CARTESIAN_POINT ( 'NONE',  ( 27.04041630560000087, -7.083781863679999624, 230.6999999999999886 ) ) ;
#22006 = ORIENTED_EDGE ( 'NONE', *, *, #10616, .F. ) ;
#22007 = CARTESIAN_POINT ( 'NONE',  ( 2.863877650502555383, -3.477044625946443812, -44.10000000002499831 ) ) ;
#22008 = DIRECTION ( 'NONE',  ( 1.000000000000000000, -9.219999999999999084E-13, 4.710999999999999616E-12 ) ) ;
#22009 = B_SPLINE_CURVE_WITH_KNOTS ( 'NONE', 4,
 ( #1762, #11353, #20949, #30553, #23478 ),
 .UNSPECIFIED., .F., .F.,
 ( 5, 5 ),
 ( -1.139969040210000006, 1.139969040210000006 ),
 .UNSPECIFIED. ) ;
#22010 = CARTESIAN_POINT ( 'NONE',  ( 5.516020573121914516, 0.1374401492888292498, -21.67661200059999871 ) ) ;
#22011 = CARTESIAN_POINT ( 'NONE',  ( -7.105427357599999217E-15, 7.105427357599999217E-15, 86.39444872449999480 ) ) ;
#22012 = LINE ( 'NONE', #2650, #958 ) ;
#22013 = EDGE_CURVE ( 'NONE', #30146, #16227, #6019, .T. ) ;
#22014 = DIRECTION ( 'NONE',  ( 0.000000000000000000, 0.3420201433259318913, -0.9396926207858126157 ) ) ;
#22015 = DIRECTION ( 'NONE',  ( 0.000000000000000000, 0.000000000000000000, -1.000000000000000000 ) ) ;
#22016 = CARTESIAN_POINT ( 'NONE',  ( -0.6751951171115599948, 5.935132877056520151, -47.78410749642499411 ) ) ;
#22017 = B_SPLINE_SURFACE_WITH_KNOTS ( 'NONE', 5, 1, ( 
 ( #6833, #26042 ),
 ( #19686, #12293 ),
 ( #1817, #12437 ),
 ( #17318, #22057 ),
 ( #508, #29271 ),
 ( #25892, #4327 ),
 ( #23533, #11563 ),
 ( #18786, #29585 ),
 ( #1266, #25020 ),
 ( #3002, #27525 ),
 ( #22362, #5820 ),
 ( #12594, #12907 ),
 ( #25175, #12747 ),
 ( #20450, #30046 ),
 ( #8321, #24713 ) ),
 .UNSPECIFIED., .F., .F., .F.,
 ( 6, 3, 3, 3, 6 ),
 ( 2, 2 ),
 ( 0.000000000000000000, 0.5239017171269999551, 1.047803434249999999, 1.571705151379999998, 1.746339057089999924 ),
 ( -0.7000000000009999335, 2.556331299420000144E-06 ),
 .UNSPECIFIED. ) ;
#22018 = PRESENTATION_LAYER_ASSIGNMENT (  '', '', ( #19498 ) ) ;
#22019 = ADVANCED_FACE ( 'NONE', ( #30422 ), #30397, .T. ) ;
#22020 = DIRECTION ( 'NONE',  ( -0.7071067811865467956, 0.6644630243886068266, 0.2418447626481644297 ) ) ;
#22021 = EDGE_CURVE ( 'NONE', #17004, #11358, #22559, .T. ) ;
#22022 = DIRECTION ( 'NONE',  ( 1.000000000000000000, -3.981190377366772282E-12, 1.940577328459388338E-12 ) ) ;
#22023 = CARTESIAN_POINT ( 'NONE',  ( -24.98081131316241255, -13.71897606304888662, 4.999998581000003384 ) ) ;
#22024 = CARTESIAN_POINT ( 'NONE',  ( -21.44011192940000399, 17.18091426960000234, 229.9751246980000019 ) ) ;
#22025 = ADVANCED_FACE ( 'NONE', ( #3501 ), #29938, .F. ) ;
#22026 = VECTOR ( 'NONE', #58, 1000.000000000000000 ) ;
#22027 = CARTESIAN_POINT ( 'NONE',  ( 9.000000000000000000, 19.99999999999999645, -43.39999999999999858 ) ) ;
#22028 = EDGE_LOOP ( 'NONE', ( #16752, #11559, #1145, #9648 ) ) ;
#22029 = CARTESIAN_POINT ( 'NONE',  ( 3.499930668453409055, 4.992711500635231836, -29.21106724380000230 ) ) ;
#22030 = VERTEX_POINT ( 'NONE', #15617 ) ;
#22031 = CARTESIAN_POINT ( 'NONE',  ( 24.63375101525831212, -12.88633855020851904, 4.098596794000014754 ) ) ;
#22032 = CARTESIAN_POINT ( 'NONE',  ( -0.6751951171115599948, 5.935132877056520151, -48.26410749632500341 ) ) ;
#22033 = VERTEX_POINT ( 'NONE', #27573 ) ;
#22034 = ORIENTED_EDGE ( 'NONE', *, *, #22523, .T. ) ;
#22035 = DIRECTION ( 'NONE',  ( 0.9591247405308765961, 0.2829836251474255882, 0.000000000000000000 ) ) ;
#22036 = ORIENTED_EDGE ( 'NONE', *, *, #7405, .T. ) ;
#22037 = CARTESIAN_POINT ( 'NONE',  ( 19.20676039538625446, 20.00032347732748761, 230.4273714388203587 ) ) ;
#22038 = APPLICATION_CONTEXT ( 'automotive_design' ) ;
#22039 = ORIENTED_EDGE ( 'NONE', *, *, #22345, .F. ) ;
#22040 = DIRECTION ( 'NONE',  ( -3.924189347185961537E-12, 0.4082287037029530552, 0.9128796883888952163 ) ) ;
#22041 = CARTESIAN_POINT ( 'NONE',  ( -9.000000000000000000, -130.0000000000000000, -43.75000000037299941 ) ) ;
#22042 = DIRECTION ( 'NONE',  ( 0.000000000000000000, -0.9396926207858125046, -0.3420201433259318358 ) ) ;
#22043 = CARTESIAN_POINT ( 'NONE',  ( 0.7743111960048394415, 4.722446211719187659, -35.69999999999998863 ) ) ;
#22044 = VECTOR ( 'NONE', #6855, 1000.000000000000000 ) ;
#22045 = CARTESIAN_POINT ( 'NONE',  ( -12.75378086759999796, -32.00000000058999916, -25.51324865459000080 ) ) ;
#22046 = CARTESIAN_POINT ( 'NONE',  ( -24.29138540600951046, 13.52003710149997140, 6.098655051000018368 ) ) ;
#22047 = LINE ( 'NONE', #3139, #13729 ) ;
#22048 = CARTESIAN_POINT ( 'NONE',  ( -23.50695067597005661, -14.84192170558070956, 224.8529579040860256 ) ) ;
#22049 = AXIS2_PLACEMENT_3D ( 'NONE', #11805, #28638, #9435 ) ;
#22050 = CARTESIAN_POINT ( 'NONE',  ( 5.399570250832249840, -0.9558082389699539272, -9.771482634699999892 ) ) ;
#22051 = CARTESIAN_POINT ( 'NONE',  ( 0.8594151385421661127, 6.036396974313712249, -28.40600711719999794 ) ) ;
#22052 = DIRECTION ( 'NONE',  ( -1.000000000000000000, 0.000000000000000000, -2.257144470970000261E-12 ) ) ;
#22053 = AXIS2_PLACEMENT_3D ( 'NONE', #21499, #11898, #31099 ) ;
#22054 = CARTESIAN_POINT ( 'NONE',  ( 24.00289804085882039, -14.02635914341071732, 5.901399682999991292 ) ) ;
#22055 = CARTESIAN_POINT ( 'NONE',  ( 9.414213562409999625, -15.31419272936388687, -74.45223986426802298 ) ) ;
#22056 = CARTESIAN_POINT ( 'NONE',  ( 5.414213562369999622, -31.28896728272270877, -80.26658230080884948 ) ) ;
#22057 = CARTESIAN_POINT ( 'NONE',  ( 1.063086518149999993, -27.77985718819999761, 225.3101849020000031 ) ) ;
#22058 = CARTESIAN_POINT ( 'NONE',  ( 0.1708583496781435063, 4.358252033550405358, -7.937690181100000686 ) ) ;
#22059 = CARTESIAN_POINT ( 'NONE',  ( 24.68173674080000168, -14.25001227039999918, 223.9000014189999774 ) ) ;
#22060 = CARTESIAN_POINT ( 'NONE',  ( -23.94167924027569327, -14.12976891190553452, 3.920144560000005107 ) ) ;
#22061 = CARTESIAN_POINT ( 'NONE',  ( 16.06675444873834380, 10.97998838177521286, -1.000005633855494125E-09 ) ) ;
#22062 = ORIENTED_EDGE ( 'NONE', *, *, #8047, .T. ) ;
#22063 = AXIS2_PLACEMENT_3D ( 'NONE', #9846, #16763, #17227 ) ;
#22064 = CARTESIAN_POINT ( 'NONE',  ( 11.00000000000000000, 27.10555629988041204, -61.14106941751904856 ) ) ;
#22065 = CARTESIAN_POINT ( 'NONE',  ( 13.12132034340000075, 20.99999999990000887, -69.22132034359999864 ) ) ;
#22066 = EDGE_LOOP ( 'NONE', ( #11691, #12413, #10600, #30507 ) ) ;
#22067 = CARTESIAN_POINT ( 'NONE',  ( 1.053429626907578687, 1.822228222601957714, 226.6412452697800290 ) ) ;
#22068 = EDGE_LOOP ( 'NONE', ( #15726, #7694, #8576, #30353, #7231, #21093, #20551, #25881, #10881, #1595, #12140, #4912, #2125, #8430, #22995, #22598, #10493 ) ) ;
#22069 = CARTESIAN_POINT ( 'NONE',  ( -4.689472217220681749, 0.6986887510282764335, -44.10000000002499831 ) ) ;
#22070 = ORIENTED_EDGE ( 'NONE', *, *, #29448, .F. ) ;
#22071 = ORIENTED_EDGE ( 'NONE', *, *, #30225, .T. ) ;
#22072 = SHAPE_DEFINITION_REPRESENTATION ( #6632, #17403 ) ;
#22073 = ORIENTED_EDGE ( 'NONE', *, *, #15387, .F. ) ;
#22074 = VECTOR ( 'NONE', #6007, 1000.000000000000114 ) ;
#22075 = DIRECTION ( 'NONE',  ( 0.000000000000000000, 0.000000000000000000, 1.000000000000000000 ) ) ;
#22076 = EDGE_CURVE ( 'NONE', #24506, #11396, #26859, .T. ) ;
#22077 = CARTESIAN_POINT ( 'NONE',  ( -9.993285220779425160, -25.61999708228226069, 186.3944487260000074 ) ) ;
#22078 = VERTEX_POINT ( 'NONE', #20497 ) ;
#22079 = DIRECTION ( 'NONE',  ( 7.759996349202911684E-13, 0.9341647027306021478, 0.3568421334038983650 ) ) ;
#22080 = CARTESIAN_POINT ( 'NONE',  ( -17.33922399257544456, -31.99968944003585136, -30.05453958706431195 ) ) ;
#22081 = CARTESIAN_POINT ( 'NONE',  ( 9.999999999959999997, -24.87868334570000073, -26.27868334529999927 ) ) ;
#22082 = EDGE_LOOP ( 'NONE', ( #3980, #14308, #28986, #14162, #8000, #1122 ) ) ;
#22083 = EDGE_CURVE ( 'NONE', #2003, #7240, #28177, .T. ) ;
#22084 = CARTESIAN_POINT ( 'NONE',  ( -8.000000000000000000, -15.86465192213301556, -74.65259062561435144 ) ) ;
#22085 = CARTESIAN_POINT ( 'NONE',  ( -2.449727287106972184, -3.823908298404834483, -17.76794088820000894 ) ) ;
#22086 = DIRECTION ( 'NONE',  ( -0.9316362575375349842, 0.3633921898465292122, -0.000000000000000000 ) ) ;
#22087 = CARTESIAN_POINT ( 'NONE',  ( -8.699999999719173260, -29.89939565891263484, -27.53479725668291422 ) ) ;
#22088 = CARTESIAN_POINT ( 'NONE',  ( -12.49429647968976198, -27.86501451498057946, -33.67401726951144525 ) ) ;
#22089 = DIRECTION ( 'NONE',  ( 3.092054264588954770E-24, -1.000000000000000000, 2.257145581552149937E-12 ) ) ;
#22090 = CARTESIAN_POINT ( 'NONE',  ( 7.312007425309012376, -6.582071621154941710, -34.26887834076562456 ) ) ;
#22091 = AXIS2_PLACEMENT_3D ( 'NONE', #16607, #7018, #26375 ) ;
#22092 = CARTESIAN_POINT ( 'NONE',  ( 0.000000000000000000, -15.18061163548115466, -76.53197586718597734 ) ) ;
#22093 = CARTESIAN_POINT ( 'NONE',  ( 26.93395386830000149, -3.298349104060000254E-15, 192.2432411359999946 ) ) ;
#22094 = CARTESIAN_POINT ( 'NONE',  ( 27.71720220719999972, 4.680497606070000316, 229.4485730569999760 ) ) ;
#22095 = DIRECTION ( 'NONE',  ( -5.962915006522622422E-16, -0.4383711467890810676, -0.8987940462991651502 ) ) ;
#22096 = ORIENTED_EDGE ( 'NONE', *, *, #25369, .F. ) ;
#22097 = CARTESIAN_POINT ( 'NONE',  ( 6.136659917679837761, 0.6935318534637759935, -55.01771407622499765 ) ) ;
#22098 = CARTESIAN_POINT ( 'NONE',  ( -12.41448843475970065, -25.69155578914772775, -23.38193380457397552 ) ) ;
#22099 = CARTESIAN_POINT ( 'NONE',  ( -3.456418106924722622, 2.806794219390951195, -38.84813418131775364 ) ) ;
#22100 = CARTESIAN_POINT ( 'NONE',  ( -4.322343509448423049, 1.111455317196624160, -68.10000000002501963 ) ) ;
#22101 = ADVANCED_FACE ( 'NONE', ( #15934 ), #27729, .F. ) ;
#22102 = ORIENTED_EDGE ( 'NONE', *, *, #3864, .T. ) ;
#22103 = CARTESIAN_POINT ( 'NONE',  ( -1.131542931821497788, -0.1196298886178837062, -98.09067668424567898 ) ) ;
#22104 = ORIENTED_EDGE ( 'NONE', *, *, #18887, .F. ) ;
#22105 = DIRECTION ( 'NONE',  ( 0.9316362575375356503, 0.3633921898465274913, 0.000000000000000000 ) ) ;
#22106 = CARTESIAN_POINT ( 'NONE',  ( -10.00000000045850967, -123.0374659603429706, -31.63552742062627487 ) ) ;
#22107 = EDGE_LOOP ( 'NONE', ( #5445, #20906, #6314, #15637, #22670 ) ) ;
#22108 = CARTESIAN_POINT ( 'NONE',  ( 4.170003719837387379, -2.319039617661839081, -27.86787294500000556 ) ) ;
#22109 = DIRECTION ( 'NONE',  ( 0.000000000000000000, 0.000000000000000000, 1.000000000000000000 ) ) ;
#22110 = AXIS2_PLACEMENT_3D ( 'NONE', #28954, #16528, #26139 ) ;
#22111 = CARTESIAN_POINT ( 'NONE',  ( -24.26970568828705055, 13.25034242773538118, -0.6999999999999784173 ) ) ;
#22112 = DIRECTION ( 'NONE',  ( 0.000000000000000000, 0.000000000000000000, -1.000000000000000000 ) ) ;
#22113 = CARTESIAN_POINT ( 'NONE',  ( -15.49562240950000103, -7.676231176589999983, 5.000000000000000000 ) ) ;
#22114 = EDGE_CURVE ( 'NONE', #24098, #4408, #9003, .T. ) ;
#22115 = LINE ( 'NONE', #5422, #6197 ) ;
#22116 = DIRECTION ( 'NONE',  ( 1.000000000000000000, 0.000000000000000000, 0.000000000000000000 ) ) ;
#22117 = DIRECTION ( 'NONE',  ( 1.000000000000000000, -1.843431230201421806E-12, 2.650498504952891752E-12 ) ) ;
#22118 = VERTEX_POINT ( 'NONE', #6337 ) ;
#22119 = CARTESIAN_POINT ( 'NONE',  ( 14.81460958102601211, -31.99970383011995523, -29.17880065134524870 ) ) ;
#22120 = DIRECTION ( 'NONE',  ( 3.582312748438143944E-12, 0.000000000000000000, -1.000000000000000000 ) ) ;
#22121 = CARTESIAN_POINT ( 'NONE',  ( -8.949800212739999594, -8.161398505059999309, 231.9999989789999972 ) ) ;
#22122 = CARTESIAN_POINT ( 'NONE',  ( -2.100000000000000089, -1.554312234479999851E-15, 227.6412452697800006 ) ) ;
#22123 = CARTESIAN_POINT ( 'NONE',  ( 7.105427357599999217E-15, 8.881784197000000993E-16, 229.6412452697800006 ) ) ;
#22124 = CARTESIAN_POINT ( 'NONE',  ( 3.760007715734309475, -21.02717377737872795, -30.56133709588283409 ) ) ;
#22125 = CARTESIAN_POINT ( 'NONE',  ( 3.405583316338488320, -2.569273692377948226, -0.6999999999999992895 ) ) ;
#22126 = CARTESIAN_POINT ( 'NONE',  ( 13.12132034340000075, 20.99999999990000887, -69.22132034359999864 ) ) ;
#22127 = CARTESIAN_POINT ( 'NONE',  ( -8.700000000035505110, -116.0414483704498139, 19.89613934350620639 ) ) ;
#22128 = ADVANCED_FACE ( 'NONE', ( #1623 ), #28879, .T. ) ;
#22129 = DIRECTION ( 'NONE',  ( -1.000000000000000000, 0.000000000000000000, 0.000000000000000000 ) ) ;
#22130 = CARTESIAN_POINT ( 'NONE',  ( -7.999999999674482609, -13.63932521616414029, -34.57331013702438582 ) ) ;
#22131 = CIRCLE ( 'NONE', #30670, 2.000000000000000000 ) ;
#22132 = EDGE_CURVE ( 'NONE', #19797, #19325, #22162, .T. ) ;
#22133 = CARTESIAN_POINT ( 'NONE',  ( -8.310304230308167561, -25.47941657935495741, 23.30551580194968153 ) ) ;
#22134 = CARTESIAN_POINT ( 'NONE',  ( 1.026682380765238767, -3.915376921412372369, -68.10000000002500542 ) ) ;
#22135 = ORIENTED_EDGE ( 'NONE', *, *, #27513, .T. ) ;
#22136 = AXIS2_PLACEMENT_3D ( 'NONE', #136, #12536, #7510 ) ;
#22137 = LINE ( 'NONE', #15360, #4223 ) ;
#22138 = CARTESIAN_POINT ( 'NONE',  ( 24.87112161019999945, -13.91739822849999975, 226.0424756639999941 ) ) ;
#22139 = CARTESIAN_POINT ( 'NONE',  ( 3.449241269337446791, -4.803451378176493591, -61.52197827312500067 ) ) ;
#22140 = ORIENTED_EDGE ( 'NONE', *, *, #9513, .T. ) ;
#22141 = ITEM_DEFINED_TRANSFORMATION ( 'NONE', 'NONE', #24385,  #17722 ) ;
#22142 = ORIENTED_EDGE ( 'NONE', *, *, #10971, .F. ) ;
#22144 = EDGE_CURVE ( 'NONE', #25501, #16559, #16563, .T. ) ;
#22143 = CARTESIAN_POINT ( 'NONE',  ( -25.90993013099999942, 13.08108041899999918, 229.0000000000000000 ) ) ;
#22145 = ORIENTED_EDGE ( 'NONE', *, *, #5389, .F. ) ;
#22146 = ORIENTED_EDGE ( 'NONE', *, *, #22849, .T. ) ;
#22147 = CARTESIAN_POINT ( 'NONE',  ( -0.1113126277255015173, -0.6952657331094624915, -40.47787123679744070 ) ) ;
#22148 = CARTESIAN_POINT ( 'NONE',  ( -24.27467683362817397, 13.55001165674122987, 3.904029272000009154 ) ) ;
#22149 = DIRECTION ( 'NONE',  ( 0.000000000000000000, 0.000000000000000000, -1.000000000000000000 ) ) ;
#22150 = CARTESIAN_POINT ( 'NONE',  ( 12.26718592479999970, -0.8151587190580000808, 232.6627648150000027 ) ) ;
#22151 = CARTESIAN_POINT ( 'NONE',  ( 24.93720649360215802, -13.79881813812812297, 6.099998581000020792 ) ) ;
#22152 = CARTESIAN_POINT ( 'NONE',  ( 4.262818619062177738, -0.7545854518158021662, -8.771482634699998115 ) ) ;
#22153 = CARTESIAN_POINT ( 'NONE',  ( -27.66290831536081285, -7.787312998891453120, 8.000000000000007105 ) ) ;
#22154 = ORIENTED_EDGE ( 'NONE', *, *, #28930, .T. ) ;
#22155 = CARTESIAN_POINT ( 'NONE',  ( 2.741601039609154356, -3.445256072409449200, -44.10000000002498410 ) ) ;
#22156 = CARTESIAN_POINT ( 'NONE',  ( 24.83401022448529005, 13.98326749045440032, 4.239871879999995485 ) ) ;
#22157 = ADVANCED_FACE ( 'NONE', ( #14050 ), #24265, .T. ) ;
#22158 = AXIS2_PLACEMENT_3D ( 'NONE', #18428, #27874, #16382 ) ;
#22159 = CARTESIAN_POINT ( 'NONE',  ( -6.202057249109299342, 1.908294659314309305, -22.92289663400000421 ) ) ;
#22160 = CARTESIAN_POINT ( 'NONE',  ( -12.60902638015870281, -26.54211788905850611, -33.90886144134552183 ) ) ;
#22161 = CARTESIAN_POINT ( 'NONE',  ( -0.5944614571882205212, -27.79380703160649446, 4.999998581000003384 ) ) ;
#22162 = B_SPLINE_CURVE_WITH_KNOTS ( 'NONE', 5,
 ( #23340, #11373, #27421, #26007, #6958, #4448, #16400, #26582, #26728, #2659, #1935, #5022, #6642, #5166, #18913 ),
 .UNSPECIFIED., .F., .F.,
 ( 6, 3, 3, 3, 6 ),
 ( 0.000000000000000000, 0.09999999999828211583, 0.3999999999988547161, 0.6999999999994273026, 1.000000000000000000 ),
 .UNSPECIFIED. ) ;
#22163 = CARTESIAN_POINT ( 'NONE',  ( 26.62724484483131349, -3.508068424019962883, 86.78285841101670428 ) ) ;
#22164 = DIRECTION ( 'NONE',  ( 0.000000000000000000, -1.000000000000000000, 0.000000000000000000 ) ) ;
#22165 = CARTESIAN_POINT ( 'NONE',  ( -3.362912017748242999, 4.936852587875802278, -47.57391720692498893 ) ) ;
#22166 = CARTESIAN_POINT ( 'NONE',  ( -7.999999999948583351, -112.9248453963972452, 6.301092398322726496 ) ) ;
#22167 = CARTESIAN_POINT ( 'NONE',  ( 6.000000000000000000, -23.16799891216055940, -79.43914708545641190 ) ) ;
#22168 = CARTESIAN_POINT ( 'NONE',  ( -18.50402760634471377, 20.00005619007534463, 230.6403179726253541 ) ) ;
#22169 = CARTESIAN_POINT ( 'NONE',  ( -21.93401131390000103, 17.57670095970000190, 229.4485730019999892 ) ) ;
#22170 = LINE ( 'NONE', #26432, #8728 ) ;
#22171 = ORIENTED_EDGE ( 'NONE', *, *, #24267, .T. ) ;
#22172 = CARTESIAN_POINT ( 'NONE',  ( 0.8594151385421661127, 6.036396974313712249, -29.00600711719999936 ) ) ;
#22173 = ORIENTED_EDGE ( 'NONE', *, *, #7586, .F. ) ;
#22174 = CARTESIAN_POINT ( 'NONE',  ( 23.81569860410000317, -13.75000000000000000, 3.900000000369999942 ) ) ;
#22175 = CARTESIAN_POINT ( 'NONE',  ( 4.315256771988532414, 1.538274589489400990, -45.92627377572499370 ) ) ;
#22176 = EDGE_LOOP ( 'NONE', ( #5401, #21952, #4923, #12071 ) ) ;
#22177 = ORIENTED_EDGE ( 'NONE', *, *, #18466, .T. ) ;
#22178 = APPLICATION_PROTOCOL_DEFINITION ( 'draft international standard', 'automotive_design', 1998, #11779 ) ;
#22179 = AXIS2_PLACEMENT_3D ( 'NONE', #1265, #10864, #30045 ) ;
#22180 = ORIENTED_EDGE ( 'NONE', *, *, #21187, .F. ) ;
#22181 = ADVANCED_FACE ( 'NONE', ( #5939, #3422 ), #27491, .T. ) ;
#22182 = ORIENTED_EDGE ( 'NONE', *, *, #24808, .T. ) ;
#22183 = CARTESIAN_POINT ( 'NONE',  ( 10.00000000070000183, -120.5233595624000174, -31.26042064949999855 ) ) ;
#22184 = DIRECTION ( 'NONE',  ( 0.000000000000000000, 0.000000000000000000, 1.000000000000000000 ) ) ;
#22185 = CARTESIAN_POINT ( 'NONE',  ( -27.50000000000000000, 3.552713678799999608E-15, 193.6055512750000105 ) ) ;
#22186 = CARTESIAN_POINT ( 'NONE',  ( -27.92857142860000152, 3.552713678799999608E-15, 87.93968498540000667 ) ) ;
#22187 = EDGE_CURVE ( 'NONE', #24425, #26590, #11791, .T. ) ;
#22188 = EDGE_CURVE ( 'NONE', #21516, #27585, #1235, .T. ) ;
#22189 = DIRECTION ( 'NONE',  ( 1.000000000000000000, 0.000000000000000000, 0.000000000000000000 ) ) ;
#22190 = CARTESIAN_POINT ( 'NONE',  ( -5.064516463719014538, -0.8477338316829075016, -0.6999999999999992895 ) ) ;
#22191 = CARTESIAN_POINT ( 'NONE',  ( 0.8228371056950706253, -6.016286819831330845, 0.2268759520000010466 ) ) ;
#22192 = CARTESIAN_POINT ( 'NONE',  ( 17.14656078599760392, 12.09981795542235439, -0.6999999999999784173 ) ) ;
#22193 = ORIENTED_EDGE ( 'NONE', *, *, #25681, .T. ) ;
#22194 = CARTESIAN_POINT ( 'NONE',  ( -2.320012200738846619, 5.013958306206127702, -8.731725184300000109 ) ) ;
#22195 = CARTESIAN_POINT ( 'NONE',  ( 2.635706879431563898, 5.544231365240147369, -32.15113063600000487 ) ) ;
#22196 = FACE_OUTER_BOUND ( 'NONE', #18505, .T. ) ;
#22197 = B_SPLINE_CURVE_WITH_KNOTS ( 'NONE', 5,
 ( #24034, #9553, #29054, #124, #24184, #23733, #11759, #440, #16781 ),
 .UNSPECIFIED., .F., .F.,
 ( 6, 3, 6 ),
 ( 0.000000000000000000, 0.6973066786029999964, 1.117931991990000151 ),
 .UNSPECIFIED. ) ;
#22198 = CARTESIAN_POINT ( 'NONE',  ( 4.276011752470107119, -42.94729992904354532, -9.547410993441516780 ) ) ;
#22199 = CARTESIAN_POINT ( 'NONE',  ( 8.523495768347459034, -15.81573655486863750, -74.63478688793190940 ) ) ;
#22200 = CARTESIAN_POINT ( 'NONE',  ( -28.49528339128749366, -0.5184828350247703277, 1.000000000000000888 ) ) ;
#22201 = CARTESIAN_POINT ( 'NONE',  ( 9.499999999611546286, -18.04864474152872589, -34.59380650643552713 ) ) ;
#22202 = CARTESIAN_POINT ( 'NONE',  ( 1.566980368899947962, 4.067530462867743779, -26.09462237480000724 ) ) ;
#22203 = VECTOR ( 'NONE', #18828, 1000.000000000000000 ) ;
#22204 = CARTESIAN_POINT ( 'NONE',  ( -10.35000000039999968, 19.99999999999999645, -2.399999999999999467 ) ) ;
#22205 = DIRECTION ( 'NONE',  ( -1.000000000000000000, 0.000000000000000000, -6.771000000000000128E-12 ) ) ;
#22206 = CARTESIAN_POINT ( 'NONE',  ( 3.550686847520000117E-05, -28.50022181210000127, 223.9000014189999774 ) ) ;
#22207 = B_SPLINE_CURVE_WITH_KNOTS ( 'NONE', 3,
 ( #24368, #19646, #312, #29081, #21861, #12554, #149, #5013, #29230, #7669 ),
 .UNSPECIFIED., .F., .F.,
 ( 4, 2, 2, 2, 4 ),
 ( 0.000000000000000000, 0.2500000000000000555, 0.5000000000000001110, 0.7500000000000002220, 1.000000000000000000 ),
 .UNSPECIFIED. ) ;
#22208 = ORIENTED_EDGE ( 'NONE', *, *, #22523, .F. ) ;
#22209 = VECTOR ( 'NONE', #21925, 1000.000000000000000 ) ;
#22210 = VECTOR ( 'NONE', #6357, 1000.000000000000000 ) ;
#22211 = CARTESIAN_POINT ( 'NONE',  ( 0.000000000000000000, 21.70000000000000284, -44.10000000017312516 ) ) ;
#22212 = DIRECTION ( 'NONE',  ( 0.000000000000000000, 0.000000000000000000, 1.000000000000000000 ) ) ;
#22213 = VERTEX_POINT ( 'NONE', #22479 ) ;
#22214 = DIRECTION ( 'NONE',  ( 1.000000000000000000, 0.000000000000000000, 0.000000000000000000 ) ) ;
#22215 = CARTESIAN_POINT ( 'NONE',  ( 7.760746006746995107, -115.2611165973680585, 21.64111469539790633 ) ) ;
#22216 = EDGE_LOOP ( 'NONE', ( #29295, #17175, #30220, #9830 ) ) ;
#22217 = CARTESIAN_POINT ( 'NONE',  ( -4.514398736596065831, 1.028232895072677344, -44.10000000002497700 ) ) ;
#22218 = ORIENTED_EDGE ( 'NONE', *, *, #23329, .T. ) ;
#22219 = ORIENTED_EDGE ( 'NONE', *, *, #2903, .F. ) ;
#22220 = VERTEX_POINT ( 'NONE', #25143 ) ;
#22221 = CARTESIAN_POINT ( 'NONE',  ( 25.04666666270000164, 13.90965967079999999, 230.2432540810000319 ) ) ;
#22222 = STYLED_ITEM ( 'NONE', ( #4688 ), #540 ) ;
#22223 = AXIS2_PLACEMENT_3D ( 'NONE', #20288, #15415, #25330 ) ;
#22224 = FACE_OUTER_BOUND ( 'NONE', #9913, .T. ) ;
#22225 = CARTESIAN_POINT ( 'NONE',  ( -7.999999999656285610, -17.88204346701441239, -37.14367873950658350 ) ) ;
#22226 = ORIENTED_EDGE ( 'NONE', *, *, #21221, .T. ) ;
#22227 = CARTESIAN_POINT ( 'NONE',  ( -24.50349639151496106, 13.13224293120369524, 6.042507865999996675 ) ) ;
#22228 = EDGE_CURVE ( 'NONE', #6120, #7813, #5478, .T. ) ;
#22229 = CARTESIAN_POINT ( 'NONE',  ( -28.68577477009351995, 9.950727454193893706, 8.000000000000007105 ) ) ;
#22230 = EDGE_CURVE ( 'NONE', #13706, #5024, #13341, .T. ) ;
#22231 = CARTESIAN_POINT ( 'NONE',  ( -17.45889703378360025, -31.99990940826297958, -29.28505019524934738 ) ) ;
#22232 = CARTESIAN_POINT ( 'NONE',  ( -19.80535357377644701, 19.50875577052588739, 3.000000106999994642 ) ) ;
#22233 = DIRECTION ( 'NONE',  ( -0.8783853955697265015, 0.4779530278697008971, -2.498001805408841824E-13 ) ) ;
#22234 = CARTESIAN_POINT ( 'NONE',  ( 3.931047123110464891, -1.876836795983964912, -20.38180150030001059 ) ) ;
#22235 = CARTESIAN_POINT ( 'NONE',  ( 5.229687933670000177, -30.84198039099999633, 228.9999999970000317 ) ) ;
#22236 = B_SPLINE_CURVE_WITH_KNOTS ( 'NONE', 5,
 ( #8874, #19104, #23684, #18784, #21004, #16120, #11404, #4625, #25889 ),
 .UNSPECIFIED., .F., .F.,
 ( 6, 3, 6 ),
 ( 0.000000000000000000, 6.585791987179998586, 10.75845896890000120 ),
 .UNSPECIFIED. ) ;
#22237 = DIRECTION ( 'NONE',  ( 0.000000000000000000, -0.000000000000000000, 1.000000000000000000 ) ) ;
#22238 = CARTESIAN_POINT ( 'NONE',  ( 23.24663841809999809, -14.69162354060000020, 225.0000000000000000 ) ) ;
#22239 = LINE ( 'NONE', #230, #18817 ) ;
#22240 = DIRECTION ( 'NONE',  ( -0.7071067811865476838, -1.595945597898661315E-12, -0.7071067811865473507 ) ) ;
#22241 = CARTESIAN_POINT ( 'NONE',  ( -10.69999999999999929, -24.87868251500000127, -30.52131748510000264 ) ) ;
#22242 = CARTESIAN_POINT ( 'NONE',  ( 17.83931934289999788, 20.00000000000000000, 230.0000000000000000 ) ) ;
#22243 = DIRECTION ( 'NONE',  ( -1.000000000000000000, 0.000000000000000000, -6.771000000000000128E-12 ) ) ;
#22244 = EDGE_LOOP ( 'NONE', ( #10498, #13104, #16838, #8278, #27588, #22208 ) ) ;
#22245 = CARTESIAN_POINT ( 'NONE',  ( 2.752605500604612843, 3.655072764488278558, -54.22619010302500442 ) ) ;
#22246 = CIRCLE ( 'NONE', #16704, 27.23548387080000310 ) ;
#22247 = DIRECTION ( 'NONE',  ( 0.000000000000000000, -0.9396926207858125046, -0.3420201433259318358 ) ) ;
#22248 = CARTESIAN_POINT ( 'NONE',  ( -1.293947800127978276, 4.175463484465264052, -39.51567878486299179 ) ) ;
#22249 = CARTESIAN_POINT ( 'NONE',  ( -4.172593481851767372, 0.2499177695104123076, -68.10000000002499121 ) ) ;
#22250 = VERTEX_POINT ( 'NONE', #15538 ) ;
#22251 = EDGE_CURVE ( 'NONE', #12444, #15899, #9421, .T. ) ;
#22252 = CARTESIAN_POINT ( 'NONE',  ( 24.25955693097017019, -12.95188430892189402, 5.642510479405106416 ) ) ;
#22253 =( NAMED_UNIT ( * ) SI_UNIT ( $, .STERADIAN. ) SOLID_ANGLE_UNIT ( ) );
#22254 = EDGE_LOOP ( 'NONE', ( #30489, #10998, #15100, #17026 ) ) ;
#22255 = FACE_OUTER_BOUND ( 'NONE', #25540, .T. ) ;
#22256 =( REPRESENTATION_RELATIONSHIP ('NONE','NONE', #2712, #527 ) REPRESENTATION_RELATIONSHIP_WITH_TRANSFORMATION ( #26554 )SHAPE_REPRESENTATION_RELATIONSHIP( ) );
#22257 = DIRECTION ( 'NONE',  ( 0.000000000000000000, 0.000000000000000000, 1.000000000000000000 ) ) ;
#22258 = ORIENTED_EDGE ( 'NONE', *, *, #24279, .T. ) ;
#22259 = CARTESIAN_POINT ( 'NONE',  ( -0.4966384047618531139, 4.769028251466922441, -26.82653409330000116 ) ) ;
#22260 = DIRECTION ( 'NONE',  ( -1.000000000000000000, 0.000000000000000000, 0.000000000000000000 ) ) ;
#22261 = CARTESIAN_POINT ( 'NONE',  ( 16.10001530785001123, 10.69382497330225767, -0.000000000000000000 ) ) ;
#22262 = CARTESIAN_POINT ( 'NONE',  ( 1.057488903014505443E-10, -103.0613381315276484, 16.56805218638653798 ) ) ;
#22263 = VECTOR ( 'NONE', #5204, 1000.000000000000000 ) ;
#22264 = CARTESIAN_POINT ( 'NONE',  ( -9.999999999559999964, 21.35000000040000145, -64.10000000000000853 ) ) ;
#22265 = DIRECTION ( 'NONE',  ( -1.000000000000000000, 4.717926049406357368E-15, -2.251139438558545733E-12 ) ) ;
#22266 = ORIENTED_EDGE ( 'NONE', *, *, #16369, .T. ) ;
#22267 = CARTESIAN_POINT ( 'NONE',  ( -26.80000000069999899, 3.281945028329999726E-15, 43.21714158909999526 ) ) ;
#22268 = PLANE ( 'NONE',  #27082 ) ;
#22269 = ORIENTED_EDGE ( 'NONE', *, *, #23096, .T. ) ;
#22270 = CARTESIAN_POINT ( 'NONE',  ( 17.64448518804794830, -20.25643828355104148, 36.78285841153859792 ) ) ;
#22271 = CARTESIAN_POINT ( 'NONE',  ( 23.70218820213038313, -12.50899637856321256, 224.5770195905794537 ) ) ;
#22272 = CARTESIAN_POINT ( 'NONE',  ( -11.76358722600000029, -3.726270779419999624, 232.6627643349999914 ) ) ;
#22273 = DIRECTION ( 'NONE',  ( 1.000000000000000000, -3.981000000000000101E-12, 1.940999999999999908E-12 ) ) ;
#22274 = B_SPLINE_CURVE_WITH_KNOTS ( 'NONE', 5,
 ( #10317, #1337, #17536, #17990, #20524, #30125, #8554, #3217, #6203, #29498, #12827, #7935, #22429, #27145, #5580 ),
 .UNSPECIFIED., .F., .F.,
 ( 6, 3, 3, 3, 6 ),
 ( 0.000000000000000000, 0.2000000000000000111, 0.3999999999986155186, 0.6999999999975770049, 1.000000000000000000 ),
 .UNSPECIFIED. ) ;
#22275 = CARTESIAN_POINT ( 'NONE',  ( -10.33059293845328241, 6.304462755849592703, 232.0000000000049738 ) ) ;
#22276 = CARTESIAN_POINT ( 'NONE',  ( -5.600170770410507259, -31.11415510469601031, -80.20295587141983162 ) ) ;
#22277 = CARTESIAN_POINT ( 'NONE',  ( 2.553054491426671291, -3.139702421570553792, -0.6999999999999992895 ) ) ;
#22278 = CARTESIAN_POINT ( 'NONE',  ( -4.499842235593497719, -29.81936866046843093, -0.6999999999999784173 ) ) ;
#22279 = CARTESIAN_POINT ( 'NONE',  ( 0.1477568879585779427, -27.50000000000000711, 3.900000000000001688 ) ) ;
#22280 = VECTOR ( 'NONE', #3777, 1000.000000000000000 ) ;
#22281 = DIRECTION ( 'NONE',  ( -1.000000000000000000, 0.000000000000000000, 0.000000000000000000 ) ) ;
#22282 = CARTESIAN_POINT ( 'NONE',  ( -7.999999999678859552, -14.17437075046522210, -33.74882213760563587 ) ) ;
#22283 = AXIS2_PLACEMENT_3D ( 'NONE', #13881, #14041, #21120 ) ;
#22284 = ADVANCED_FACE ( 'NONE', ( #27651 ), #4269, .F. ) ;
#22285 =( GEOMETRIC_REPRESENTATION_CONTEXT ( 3 ) GLOBAL_UNCERTAINTY_ASSIGNED_CONTEXT ( ( #3062 ) ) GLOBAL_UNIT_ASSIGNED_CONTEXT ( ( #18882, #17402, #10025 ) ) REPRESENTATION_CONTEXT ( 'NONE', 'WORKASPACE' ) );
#22286 = CARTESIAN_POINT ( 'NONE',  ( -25.90058877277587612, -6.940365930346072965, 93.21714158835418118 ) ) ;
#22287 = CARTESIAN_POINT ( 'NONE',  ( 0.4478609109052260062, -28.49673184309145668, 6.098651241000007772 ) ) ;
#22288 = CIRCLE ( 'NONE', #26315, 7.354069295110000404 ) ;
#22289 = EDGE_LOOP ( 'NONE', ( #27125, #9363, #9786, #20945 ) ) ;
#22290 = EDGE_CURVE ( 'NONE', #24157, #5864, #21865, .T. ) ;
#22291 = CARTESIAN_POINT ( 'NONE',  ( -24.60699806910000120, -12.93667933180000063, 225.0000014190000002 ) ) ;
#22292 = LINE ( 'NONE', #19930, #4409 ) ;
#22293 = CARTESIAN_POINT ( 'NONE',  ( -5.941465883516308999, 0.03012783874251079297, -63.05122063482500039 ) ) ;
#22294 = ORIENTED_EDGE ( 'NONE', *, *, #16546, .T. ) ;
#22295 = ORIENTED_EDGE ( 'NONE', *, *, #25276, .T. ) ;
#22296 = CARTESIAN_POINT ( 'NONE',  ( 8.700000000283306889, -21.59962967316020865, -40.40111538753404830 ) ) ;
#22297 = ORIENTED_EDGE ( 'NONE', *, *, #6762, .T. ) ;
#22298 = EDGE_LOOP ( 'NONE', ( #9014, #16483, #9476, #4685 ) ) ;
#22299 = EDGE_CURVE ( 'NONE', #29242, #25227, #29315, .T. ) ;
#22300 = VECTOR ( 'NONE', #15276, 1000.000000000000000 ) ;
#22301 = CARTESIAN_POINT ( 'NONE',  ( 8.999999999770000869, 21.70000000000000284, -45.10000000000000142 ) ) ;
#22302 = VECTOR ( 'NONE', #9587, 1000.000000000000000 ) ;
#22303 = CARTESIAN_POINT ( 'NONE',  ( -12.29999999982333492, -28.51085694111270286, -31.02135916526277981 ) ) ;
#22304 = CARTESIAN_POINT ( 'NONE',  ( -26.62724484483129928, -3.508068424019927356, 143.2171415880000040 ) ) ;
#22305 = AXIS2_PLACEMENT_3D ( 'NONE', #4951, #29019, #2446 ) ;
#22306 = CARTESIAN_POINT ( 'NONE',  ( -23.56862142526452786, 14.78130733048562995, 8.000000000000007105 ) ) ;
#22307 = CARTESIAN_POINT ( 'NONE',  ( 25.12046395012763256, -13.46291002078069887, 6.042507865999996675 ) ) ;
#22308 = DIRECTION ( 'NONE',  ( 0.000000000000000000, 1.000000000000000000, 0.000000000000000000 ) ) ;
#22309 = VERTEX_POINT ( 'NONE', #10986 ) ;
#22310 = CARTESIAN_POINT ( 'NONE',  ( 2.603364185612058179, -3.472772091317404275, -44.10000000002499121 ) ) ;
#22311 = CARTESIAN_POINT ( 'NONE',  ( 24.47278418934676836, 14.60601539428441598, 3.904031772999999816 ) ) ;
#22312 = CARTESIAN_POINT ( 'NONE',  ( -1.782928038406565774, 3.983823234458339080, -22.73780126169999605 ) ) ;
#22313 = DIRECTION ( 'NONE',  ( 1.000000000000000000, 0.000000000000000000, 0.000000000000000000 ) ) ;
#22314 = FACE_OUTER_BOUND ( 'NONE', #2387, .T. ) ;
#22315 = PRESENTATION_STYLE_ASSIGNMENT (( #17725 ) ) ;
#22316 = CARTESIAN_POINT ( 'NONE',  ( -10.69999999999999929, -43.95328087560000085, -27.24755286599999948 ) ) ;
#22317 = CARTESIAN_POINT ( 'NONE',  ( 1.760648636159114933, 4.990344452800529851, -44.74079303332499791 ) ) ;
#22318 = B_SPLINE_CURVE_WITH_KNOTS ( 'NONE', 3,
 ( #24587, #29609, #15136, #29452, #24736, #5686 ),
 .UNSPECIFIED., .F., .F.,
 ( 4, 2, 4 ),
 ( 0.000000000000000000, 0.5000000000000000000, 1.000000000000000000 ),
 .UNSPECIFIED. ) ;
#22319 = CARTESIAN_POINT ( 'NONE',  ( 4.638687372183705193, -19.12054368226126400, -31.49126272761206025 ) ) ;
#22320 = CARTESIAN_POINT ( 'NONE',  ( 9.544994065185530729, -25.04267878452545304, 203.8307228059247507 ) ) ;
#22321 = CARTESIAN_POINT ( 'NONE',  ( -18.23049700918086202, 20.00000270586327389, 230.6797159284481324 ) ) ;
#22322 = ADVANCED_FACE ( 'NONE', ( #30501 ), #23428, .F. ) ;
#22323 = CARTESIAN_POINT ( 'NONE',  ( -26.80000000000000071, -7.460698725479998033E-14, 230.0000000000000000 ) ) ;
#22324 = AXIS2_PLACEMENT_3D ( 'NONE', #18638, #4016, #4486 ) ;
#22325 = CIRCLE ( 'NONE', #14780, 8.134694044909998922 ) ;
#22326 = CIRCLE ( 'NONE', #30894, 3.199999983039998774 ) ;
#22327 = CARTESIAN_POINT ( 'NONE',  ( -10.14902473071360411, -26.01926976408356396, 42.06031501460000044 ) ) ;
#22328 = ORIENTED_EDGE ( 'NONE', *, *, #29311, .T. ) ;
#22329 = CARTESIAN_POINT ( 'NONE',  ( -2.705882613314523955, 5.963358562559473164, -32.32635571290000343 ) ) ;
#22330 = ORIENTED_EDGE ( 'NONE', *, *, #8095, .T. ) ;
#22331 = CYLINDRICAL_SURFACE ( 'NONE', #23326, 26.80000000000002203 ) ;
#22332 = CARTESIAN_POINT ( 'NONE',  ( 0.6613659943793989138, -4.850238491497672833, -50.16468436622500349 ) ) ;
#22333 = ORIENTED_EDGE ( 'NONE', *, *, #25369, .T. ) ;
#22334 = EDGE_CURVE ( 'NONE', #9128, #21922, #1855, .T. ) ;
#22335 = VERTEX_POINT ( 'NONE', #21055 ) ;
#22336 = DIRECTION ( 'NONE',  ( 0.000000000000000000, 0.000000000000000000, 1.000000000000000000 ) ) ;
#22337 = ORIENTED_EDGE ( 'NONE', *, *, #25218, .T. ) ;
#22338 = ORIENTED_EDGE ( 'NONE', *, *, #28904, .F. ) ;
#22339 = ADVANCED_FACE ( 'NONE', ( #8767 ), #25933, .F. ) ;
#22340 = CARTESIAN_POINT ( 'NONE',  ( 23.95489023949999918, -14.10735628980000023, 226.0798541909999813 ) ) ;
#22341 = DIRECTION ( 'NONE',  ( -1.000000000000000000, 0.000000000000000000, 0.000000000000000000 ) ) ;
#22342 = CARTESIAN_POINT ( 'NONE',  ( 27.79539923781924315, 0.5057481687932352532, 1.000000000000000888 ) ) ;
#22343 = CARTESIAN_POINT ( 'NONE',  ( 2.919513974631230191, 4.160045535825797280, -35.69999999999999574 ) ) ;
#22344 = CARTESIAN_POINT ( 'NONE',  ( -12.46077600684266962, -28.06697140616160269, -23.24287214062465523 ) ) ;
#22345 = EDGE_CURVE ( 'NONE', #13996, #1635, #5255, .T. ) ;
#22346 = CARTESIAN_POINT ( 'NONE',  ( -4.891960740915500594, 0.9743236597107772790, -0.6999999999999992895 ) ) ;
#22347 = DIRECTION ( 'NONE',  ( 0.000000000000000000, 0.000000000000000000, 1.000000000000000000 ) ) ;
#22348 = VECTOR ( 'NONE', #23498, 1000.000000000000000 ) ;
#22349 = DIRECTION ( 'NONE',  ( 1.595945597898660305E-12, -0.7071067811865475727, 0.7071067811865475727 ) ) ;
#22350 = DIRECTION ( 'NONE',  ( -0.4999999999969509945, -0.4151946956549595336, -0.7600087925169251024 ) ) ;
#22351 = AXIS2_PLACEMENT_3D ( 'NONE', #6566, #25468, #13494 ) ;
#22352 = PRODUCT_DEFINITION ( 'UNKNOWN', '', #10838, #29800 ) ;
#22353 = VECTOR ( 'NONE', #27401, 1000.000000000000000 ) ;
#22354 = CARTESIAN_POINT ( 'NONE',  ( -3.222838750790782303, 3.984490938364168233, -14.54102819870000474 ) ) ;
#22355 = CARTESIAN_POINT ( 'NONE',  ( 2.384687176697237732, 5.016209330415857259, -31.15113063599999776 ) ) ;
#22356 = DIRECTION ( 'NONE',  ( 0.000000000000000000, 0.000000000000000000, 1.000000000000000000 ) ) ;
#22357 = B_SPLINE_CURVE_WITH_KNOTS ( 'NONE', 3,
 ( #19848, #20291, #29429, #13054, #8165, #5666 ),
 .UNSPECIFIED., .F., .F.,
 ( 4, 2, 4 ),
 ( 0.000000000000000000, 0.5000000000000000000, 1.000000000000000000 ),
 .UNSPECIFIED. ) ;
#22358 = B_SPLINE_CURVE_WITH_KNOTS ( 'NONE', 3,
 ( #23768, #18409, #25818, #1894, #16514, #27853, #20773, #21092, #2209, #6302 ),
 .UNSPECIFIED., .F., .F.,
 ( 4, 2, 2, 2, 4 ),
 ( 0.000000000000000000, 0.2499999999999998890, 0.4999999999999997780, 0.7499999999999998890, 1.000000000000000000 ),
 .UNSPECIFIED. ) ;
#22359 = CARTESIAN_POINT ( 'NONE',  ( -9.999999999939999995, -25.00000000000000000, -16.71944709739999979 ) ) ;
#22360 = DIRECTION ( 'NONE',  ( -0.000000000000000000, 1.000000000000000000, -2.258510841069999963E-12 ) ) ;
#22361 = FACE_BOUND ( 'NONE', #18266, .T. ) ;
#22362 = CARTESIAN_POINT ( 'NONE',  ( 0.2462945485050000161, -28.49939181889999773, 226.0797949779999954 ) ) ;
#22363 = DIRECTION ( 'NONE',  ( 0.9316362575375356503, 0.3633921898465274913, 0.000000000000000000 ) ) ;
#22364 = FACE_OUTER_BOUND ( 'NONE', #19074, .T. ) ;
#22365 = CARTESIAN_POINT ( 'NONE',  ( -9.738910687886855655, -24.96785170200598714, 115.0000000000000000 ) ) ;
#22366 = CARTESIAN_POINT ( 'NONE',  ( 1.127732790480000080, -28.47784299079999926, 224.8959500220000223 ) ) ;
#22367 = EDGE_CURVE ( 'NONE', #20042, #11709, #21806, .T. ) ;
#22368 = CIRCLE ( 'NONE', #20867, 0.9999999999999982236 ) ;
#22369 = EDGE_LOOP ( 'NONE', ( #22891, #6655 ) ) ;
#22370 = EDGE_CURVE ( 'NONE', #7467, #26555, #18204, .T. ) ;
#22371 = CARTESIAN_POINT ( 'NONE',  ( 18.11692203360697562, -8.427117116353246118, -0.6999999999999784173 ) ) ;
#22372 = CARTESIAN_POINT ( 'NONE',  ( 11.39835558780000113, 19.99999999999999645, -0.7167260558000043691 ) ) ;
#22373 = ORIENTED_EDGE ( 'NONE', *, *, #27076, .F. ) ;
#22374 = DIRECTION ( 'NONE',  ( 0.000000000000000000, 0.000000000000000000, -1.000000000000000000 ) ) ;
#22375 = CARTESIAN_POINT ( 'NONE',  ( 7.734594132576882330, -115.2493501891094780, 21.66742669895628026 ) ) ;
#22376 = ORIENTED_EDGE ( 'NONE', *, *, #17891, .T. ) ;
#22377 = DIRECTION ( 'NONE',  ( -1.000000000000000000, 0.000000000000000000, 0.000000000000000000 ) ) ;
#22378 = AXIS2_PLACEMENT_3D ( 'NONE', #7275, #12142, #16702 ) ;
#22379 = EDGE_LOOP ( 'NONE', ( #934, #17018, #4081, #18588 ) ) ;
#22380 = EDGE_CURVE ( 'NONE', #18081, #16790, #6260, .T. ) ;
#22381 = ORIENTED_EDGE ( 'NONE', *, *, #17127, .T. ) ;
#22382 = EDGE_LOOP ( 'NONE', ( #25676, #13420, #3908, #16177 ) ) ;
#22383 = CARTESIAN_POINT ( 'NONE',  ( -16.81341597756113515, 9.900182044522454206, -0.6999999999999784173 ) ) ;
#22384 = LINE ( 'NONE', #17635, #29222 ) ;
#22385 = CARTESIAN_POINT ( 'NONE',  ( 24.49999999470000134, -3.000285566199999922E-15, 40.00000000070000539 ) ) ;
#22386 = CARTESIAN_POINT ( 'NONE',  ( -3.378474373710000034, -11.51459555979999827, 232.0000000000000000 ) ) ;
#22387 = CARTESIAN_POINT ( 'NONE',  ( -19.80526803560000104, 19.50877411510000314, 228.1999999999999886 ) ) ;
#22388 = DIRECTION ( 'NONE',  ( 0.000000000000000000, -1.000000000000000000, 0.000000000000000000 ) ) ;
#22389 = CARTESIAN_POINT ( 'NONE',  ( 9.499999999614264112, -13.84939817494163350, -36.47165854346829406 ) ) ;
#22390 = AXIS2_PLACEMENT_3D ( 'NONE', #839, #12939, #27411 ) ;
#22391 = AXIS2_PLACEMENT_3D ( 'NONE', #12109, #23777, #26283 ) ;
#22392 = CARTESIAN_POINT ( 'NONE',  ( 10.34999999979999963, -25.00000000000000000, -2.400000000399998612 ) ) ;
#22393 = CARTESIAN_POINT ( 'NONE',  ( 3.956700543085260424, -2.628121156294163541, -0.9587547302000037908 ) ) ;
#22394 = CARTESIAN_POINT ( 'NONE',  ( 1.265035515811502309, -4.453021097817297047, -21.29535708919999593 ) ) ;
#22395 = FACE_OUTER_BOUND ( 'NONE', #10880, .T. ) ;
#22396 = CARTESIAN_POINT ( 'NONE',  ( 23.89354037824641708, 14.21129111442623660, 6.099998580999996811 ) ) ;
#22397 = CARTESIAN_POINT ( 'NONE',  ( 23.67167941920536833, -13.99714051965694850, 226.0719093208177526 ) ) ;
#22398 = CARTESIAN_POINT ( 'NONE',  ( -7.999999999660042604, -18.28443193496838504, -36.42483736938474692 ) ) ;
#22399 = CARTESIAN_POINT ( 'NONE',  ( -6.585786437629999490, -16.41511111490214603, -74.85294138696069410 ) ) ;
#22400 = CARTESIAN_POINT ( 'NONE',  ( -3.040504020835836041, -1.733590291693717145, -0.6999999999999784173 ) ) ;
#22401 = CARTESIAN_POINT ( 'NONE',  ( -11.69999999989999928, -24.11120071630000083, -1.399999999999998579 ) ) ;
#22402 = DIRECTION ( 'NONE',  ( -0.000000000000000000, 1.000000000000000000, -2.255973188440000244E-12 ) ) ;
#22403 = ADVANCED_FACE ( 'NONE', ( #11455 ), #15862, .T. ) ;
#22404 = ORIENTED_EDGE ( 'NONE', *, *, #130, .T. ) ;
#22405 = CARTESIAN_POINT ( 'NONE',  ( 0.8945918243927786229, -4.819150861182647461, -58.34125695792499045 ) ) ;
#22406 = CARTESIAN_POINT ( 'NONE',  ( -8.699999999683917906, -16.84112679184576677, -33.19732076807623145 ) ) ;
#22407 = DIRECTION ( 'NONE',  ( 0.000000000000000000, -2.257157423930000049E-12, -1.000000000000000000 ) ) ;
#22408 = EDGE_CURVE ( 'NONE', #28115, #14021, #28934, .T. ) ;
#22409 = CARTESIAN_POINT ( 'NONE',  ( -24.31698661571731890, 13.27613583500951755, 0.02487588100000270863 ) ) ;
#22410 = CARTESIAN_POINT ( 'NONE',  ( -4.289535850812038476, 1.058007967770713487, -68.10000000002500542 ) ) ;
#22411 = EDGE_CURVE ( 'NONE', #23813, #15558, #4769, .T. ) ;
#22412 = ORIENTED_EDGE ( 'NONE', *, *, #25620, .F. ) ;
#22413 = ORIENTED_EDGE ( 'NONE', *, *, #11105, .F. ) ;
#22414 = CARTESIAN_POINT ( 'NONE',  ( -3.181902231748757526, 1.609514238137835118, -88.52261276242234089 ) ) ;
#22415 = B_SPLINE_CURVE_WITH_KNOTS ( 'NONE', 5,
 ( #29234, #24214, #7224, #10207, #14472, #17432, #28770, #19807, #21704, #7533, #21868, #29393, #7830, #16972, #316 ),
 .UNSPECIFIED., .F., .F.,
 ( 6, 3, 3, 3, 6 ),
 ( 10.75845896890000120, 13.17160131670000034, 18.65982209409999726, 20.85462969119999954, 21.51695459200000116 ),
 .UNSPECIFIED. ) ;
#22416 = VERTEX_POINT ( 'NONE', #2328 ) ;
#22418 = DIRECTION ( 'NONE',  ( 3.924189347185962345E-12, -0.4082287037029530552, -0.9128796883888953273 ) ) ;
#22417 = B_SPLINE_CURVE_WITH_KNOTS ( 'NONE', 1,
 ( #26431, #29236 ),
 .UNSPECIFIED., .F., .F.,
 ( 2, 2 ),
 ( -2.557520719980000135E-06, 0.7000000000009999335 ),
 .UNSPECIFIED. ) ;
#22419 = CARTESIAN_POINT ( 'NONE',  ( -10.82908725742657374, -27.76276047461854546, 93.21714158839999698 ) ) ;
#22420 = ORIENTED_EDGE ( 'NONE', *, *, #25149, .F. ) ;
#22421 = CARTESIAN_POINT ( 'NONE',  ( -4.150389416700803302, 1.923785201099231790, -65.77526299422500244 ) ) ;
#22422 = CARTESIAN_POINT ( 'NONE',  ( -13.73802074570000009, -27.58422840009999888, 229.2930759660000035 ) ) ;
#22423 = PLANE ( 'NONE',  #26232 ) ;
#22424 = CARTESIAN_POINT ( 'NONE',  ( 11.50543345310245513, 20.99999999999807798, -55.48449633255769697 ) ) ;
#22425 = CARTESIAN_POINT ( 'NONE',  ( -27.76135144349999706, 3.399672736839999702E-15, 192.3385858899999903 ) ) ;
#22426 = CARTESIAN_POINT ( 'NONE',  ( -20.30396346370000060, 20.00000000000000000, 227.0000000000000000 ) ) ;
#22427 = ORIENTED_EDGE ( 'NONE', *, *, #10549, .T. ) ;
#22428 = DIRECTION ( 'NONE',  ( 1.000000000000000000, -1.224606353819999829E-16, 0.000000000000000000 ) ) ;
#22429 = CARTESIAN_POINT ( 'NONE',  ( 18.15340080560000047, 19.92139761430000178, 229.9929672670000116 ) ) ;
#22430 = VERTEX_POINT ( 'NONE', #19151 ) ;
#22431 = EDGE_CURVE ( 'NONE', #13180, #3651, #22197, .T. ) ;
#22432 = CARTESIAN_POINT ( 'NONE',  ( 3.072394438959999974, 1.678456730820000020, 227.6468472915199754 ) ) ;
#22433 = CARTESIAN_POINT ( 'NONE',  ( -24.83401023410007724, -13.98326748972919553, 5.760125276000005456 ) ) ;
#22434 = ADVANCED_FACE ( 'NONE', ( #21364 ), #2478, .F. ) ;
#22435 = LINE ( 'NONE', #730, #17794 ) ;
#22436 = DIRECTION ( 'NONE',  ( 0.000000000000000000, 0.000000000000000000, -1.000000000000000000 ) ) ;
#22437 = CARTESIAN_POINT ( 'NONE',  ( -8.160452367545484975, -25.52912514472581051, 206.9265757142945006 ) ) ;
#22438 = CARTESIAN_POINT ( 'NONE',  ( 3.521492630942301361, -2.494370597472697071, -0.6999999999999992895 ) ) ;
#22439 = CARTESIAN_POINT ( 'NONE',  ( 24.03254869350325507, -20.47699196171803848, 0.5017677510000262409 ) ) ;
#22440 = CARTESIAN_POINT ( 'NONE',  ( 8.700000000244115128, -26.99999999999395328, -28.39999999994493862 ) ) ;
#22441 = VERTEX_POINT ( 'NONE', #9863 ) ;
#22442 = LINE ( 'NONE', #19770, #28340 ) ;
#22443 = CARTESIAN_POINT ( 'NONE',  ( 23.69119887980000172, 20.94188554260000146, 229.0000000000000000 ) ) ;
#22444 = B_SPLINE_CURVE_WITH_KNOTS ( 'NONE', 5,
 ( #20523, #30124, #17989, #10615, #27442, #22893, #27601, #29495, #26988, #7934, #17383, #15490, #20065, #24782, #12826 ),
 .UNSPECIFIED., .F., .F.,
 ( 6, 3, 3, 3, 6 ),
 ( 0.000000000000000000, 0.2999999999994273914, 0.5999999999977095877, 0.8999999999937011719, 1.000000000000000000 ),
 .UNSPECIFIED. ) ;
#22445 = CARTESIAN_POINT ( 'NONE',  ( -9.254368700311671248, -25.15168151593200818, 25.15520747740333363 ) ) ;
#22446 = DIRECTION ( 'NONE',  ( 1.000000000000000000, 0.000000000000000000, 0.000000000000000000 ) ) ;
#22447 = EDGE_LOOP ( 'NONE', ( #11617, #17512, #2059, #16942 ) ) ;
#22448 = CARTESIAN_POINT ( 'NONE',  ( 11.69999999989999928, -24.11120071670000087, -0.6999999999999992895 ) ) ;
#22449 = DIRECTION ( 'NONE',  ( 0.000000000000000000, 0.000000000000000000, -1.000000000000000000 ) ) ;
#22450 = FACE_OUTER_BOUND ( 'NONE', #27897, .T. ) ;
#22451 = CARTESIAN_POINT ( 'NONE',  ( 4.855544147916073250, 1.989531035200713838, -61.64141554682499446 ) ) ;
#22452 = ORIENTED_EDGE ( 'NONE', *, *, #9840, .F. ) ;
#22453 = ORIENTED_EDGE ( 'NONE', *, *, #11755, .F. ) ;
#22454 = CARTESIAN_POINT ( 'NONE',  ( 27.24406355354254217, 0.4957164003247201967, 0.08279779300002232389 ) ) ;
#22455 = VERTEX_POINT ( 'NONE', #28741 ) ;
#22456 = VERTEX_POINT ( 'NONE', #26397 ) ;
#22457 = EDGE_CURVE ( 'NONE', #8183, #27584, #20854, .T. ) ;
#22458 = CARTESIAN_POINT ( 'NONE',  ( -12.12499970530000049, 21.69999999919999212, -55.73512393530000253 ) ) ;
#22459 = CARTESIAN_POINT ( 'NONE',  ( 24.93720649360215802, -13.79881813812812297, 3.899998581000013509 ) ) ;
#22460 = CARTESIAN_POINT ( 'NONE',  ( 10.69999999999999929, -120.0000000000000000, -41.24671599705000347 ) ) ;
#22461 = CARTESIAN_POINT ( 'NONE',  ( -24.62904075447892183, 12.95915071291530829, 8.000000000000007105 ) ) ;
#22462 = DIRECTION ( 'NONE',  ( 0.000000000000000000, 0.000000000000000000, 1.000000000000000000 ) ) ;
#22463 = CYLINDRICAL_SURFACE ( 'NONE', #26085, 3.000000000000003997 ) ;
#22464 = ORIENTED_EDGE ( 'NONE', *, *, #25415, .F. ) ;
#22465 = CARTESIAN_POINT ( 'NONE',  ( 2.355191831056934415, -3.552166203893096785, -44.10000000002498410 ) ) ;
#22466 = CARTESIAN_POINT ( 'NONE',  ( -24.86822223968379575, -13.92223202017373573, 4.319317663000004970 ) ) ;
#22467 = EDGE_CURVE ( 'NONE', #19740, #16896, #7278, .T. ) ;
#22468 = MECHANICAL_DESIGN_GEOMETRIC_PRESENTATION_REPRESENTATION (  '', ( #29487 ), #8889 ) ;
#22469 = CARTESIAN_POINT ( 'NONE',  ( -2.942059828035410440, -4.605008556695580957, -22.70891267860000085 ) ) ;
#22470 = LINE ( 'NONE', #617, #8614 ) ;
#22471 = DIRECTION ( 'NONE',  ( -0.000000000000000000, 1.000000000000000000, -2.257145581549999994E-12 ) ) ;
#22472 = AXIS2_PLACEMENT_3D ( 'NONE', #15335, #7929, #5730 ) ;
#22473 = CARTESIAN_POINT ( 'NONE',  ( 25.43121960300669215, -8.635379644106567554, 86.78285841119168253 ) ) ;
#22474 = CARTESIAN_POINT ( 'NONE',  ( -9.738910687886855655, -24.96785170200598714, 115.0000000000000000 ) ) ;
#22475 = CARTESIAN_POINT ( 'NONE',  ( -1.460566089872938900, -4.291843709425553044, -46.99520033292500187 ) ) ;
#22476 = CYLINDRICAL_SURFACE ( 'NONE', #27287, 1.100000000000002309 ) ;
#22477 = DIRECTION ( 'NONE',  ( 1.000000000000000000, 0.000000000000000000, 0.000000000000000000 ) ) ;
#22478 = CARTESIAN_POINT ( 'NONE',  ( -19.98328564520809891, 20.00005048715008726, 229.8503962144677359 ) ) ;
#22479 = CARTESIAN_POINT ( 'NONE',  ( -12.41421356240000051, 25.87105682045942245, -59.46203493729375822 ) ) ;
#22480 = CARTESIAN_POINT ( 'NONE',  ( 0.5057536231481192246, -27.79562098839016571, 6.099998581000020792 ) ) ;
#22481 = ORIENTED_EDGE ( 'NONE', *, *, #18564, .T. ) ;
#22482 = PRODUCT_DEFINITION_SHAPE ( 'NONE', 'NONE',  #31121 ) ;
#22483 = CARTESIAN_POINT ( 'NONE',  ( -1.932773295258167545, 4.259541830411040841, -32.22635571290000911 ) ) ;
#22484 = ORIENTED_EDGE ( 'NONE', *, *, #28630, .T. ) ;
#22485 = EDGE_CURVE ( 'NONE', #29063, #26584, #5273, .T. ) ;
#22486 = CARTESIAN_POINT ( 'NONE',  ( 13.99999999999999822, 21.69999999994720596, -67.49379052020815095 ) ) ;
#22487 = CARTESIAN_POINT ( 'NONE',  ( -4.064488300603595228, -4.392874523441014034, -50.19612412472499585 ) ) ;
#22488 = ORIENTED_EDGE ( 'NONE', *, *, #13092, .T. ) ;
#22489 = ORIENTED_EDGE ( 'NONE', *, *, #15121, .T. ) ;
#22490 = TOROIDAL_SURFACE ( 'NONE', #29018, 24.50000000000000000, 3.200000000000000178 ) ;
#22491 = DIRECTION ( 'NONE',  ( 1.000000000000000000, 0.000000000000000000, 0.000000000000000000 ) ) ;
#22492 = ORIENTED_EDGE ( 'NONE', *, *, #26690, .T. ) ;
#22493 = CIRCLE ( 'NONE', #384, 1.926829268289999231 ) ;
#22494 = ORIENTED_EDGE ( 'NONE', *, *, #19314, .T. ) ;
#22495 = B_SPLINE_CURVE_WITH_KNOTS ( 'NONE', 3,
 ( #16626, #122, #5129, #21672, #24182, #14282 ),
 .UNSPECIFIED., .F., .F.,
 ( 4, 2, 4 ),
 ( 0.000000000000000000, 0.5000000000000000000, 1.000000000000000000 ),
 .UNSPECIFIED. ) ;
#22496 = CARTESIAN_POINT ( 'NONE',  ( -10.32522729140000095, -24.73114799960000099, -1.399999999999998579 ) ) ;
#22497 = CARTESIAN_POINT ( 'NONE',  ( 23.85408961476034051, 14.27673465474052072, 3.901342939999996595 ) ) ;
#22498 = DIRECTION ( 'NONE',  ( -1.000000000000000000, -6.565028073413479156E-24, -2.257144471327815248E-12 ) ) ;
#22499 = FACE_OUTER_BOUND ( 'NONE', #1796, .T. ) ;
#22500 = CARTESIAN_POINT ( 'NONE',  ( 11.20000000009999930, -27.00000000000000000, -28.39999999989999679 ) ) ;
#22501 = CARTESIAN_POINT ( 'NONE',  ( -23.55406855550000245, 16.04544956020000157, 222.0000000000000000 ) ) ;
#22502 = CARTESIAN_POINT ( 'NONE',  ( -3.746730446667854153, 2.137546260429493472, -0.6999999999999992895 ) ) ;
#22503 = DIRECTION ( 'NONE',  ( -7.764622278472185525E-13, -0.9341647027306024809, -0.3568421334038978099 ) ) ;
#22504 = CARTESIAN_POINT ( 'NONE',  ( -3.455669901315109094, -1.014542102293449322, 227.7047085156324044 ) ) ;
#22505 = CARTESIAN_POINT ( 'NONE',  ( -21.71008920740291259, 18.50699696262706695, 5.000000064000004407 ) ) ;
#22506 = ORIENTED_EDGE ( 'NONE', *, *, #20200, .F. ) ;
#22507 = ADVANCED_FACE ( 'NONE', ( #17094 ), #26694, .T. ) ;
#22508 = B_SPLINE_CURVE_WITH_KNOTS ( 'NONE', 3,
 ( #1488, #15950, #8859, #3668, #18461, #30439 ),
 .UNSPECIFIED., .F., .F.,
 ( 4, 2, 4 ),
 ( 0.000000000000000000, 0.5000000000000000000, 1.000000000000000000 ),
 .UNSPECIFIED. ) ;
#22509 = CARTESIAN_POINT ( 'NONE',  ( 3.904508939291361003, -1.994718106397497914, -11.91474735220000092 ) ) ;
#22510 = CARTESIAN_POINT ( 'NONE',  ( 1.882647771056455976, 3.960165260869605408, -32.15113063600000487 ) ) ;
#22511 = VECTOR ( 'NONE', #4465, 1000.000000000000000 ) ;
#22512 = CARTESIAN_POINT ( 'NONE',  ( 16.50835677013856184, 10.10662636436282824, 0.000000000000000000 ) ) ;
#22513 = CYLINDRICAL_SURFACE ( 'NONE', #17241, 10.00000000000000533 ) ;
#22514 = FACE_OUTER_BOUND ( 'NONE', #18764, .T. ) ;
#22515 = CARTESIAN_POINT ( 'NONE',  ( -28.35924375250000296, -1.754620794519999711E-14, 229.7625741969999922 ) ) ;
#22516 = CARTESIAN_POINT ( 'NONE',  ( -10.00000000070000183, -29.30501631370000482, -26.47986984990000181 ) ) ;
#22517 = CARTESIAN_POINT ( 'NONE',  ( 22.63992238019999803, -14.34133587289999845, 225.0000000000000000 ) ) ;
#22518 = CARTESIAN_POINT ( 'NONE',  ( -9.747572777117802900, -14.93176075901369515, -74.31304601042864988 ) ) ;
#22519 = CARTESIAN_POINT ( 'NONE',  ( -6.839399949238186061, -8.490264634313129832, -36.67599624484527965 ) ) ;
#22520 = VECTOR ( 'NONE', #9607, 999.9999999999997726 ) ;
#22521 = EDGE_LOOP ( 'NONE', ( #8185, #15218 ) ) ;
#22522 = ADVANCED_FACE ( 'NONE', ( #28902 ), #23890, .T. ) ;
#22523 = EDGE_CURVE ( 'NONE', #23530, #29115, #24340, .T. ) ;
#22524 = CARTESIAN_POINT ( 'NONE',  ( 23.47637528925218575, 14.89020703997133488, 5.901296968999991677 ) ) ;
#22525 = CARTESIAN_POINT ( 'NONE',  ( 3.072394438959999974, 1.678456730820000020, 230.8356432492296619 ) ) ;
#22526 = ORIENTED_EDGE ( 'NONE', *, *, #21058, .F. ) ;
#22527 = CARTESIAN_POINT ( 'NONE',  ( -7.999999999692643193, -25.56262797781471718, -31.06236252952192700 ) ) ;
#22528 = DIRECTION ( 'NONE',  ( 8.432460690569534438E-06, -1.375682488550163830E-15, -0.9999999999644468840 ) ) ;
#22529 = ORIENTED_EDGE ( 'NONE', *, *, #27492, .F. ) ;
#22530 = CARTESIAN_POINT ( 'NONE',  ( 24.41841038956698640, 14.69667349781389376, 3.899998581000013509 ) ) ;
#22531 = VERTEX_POINT ( 'NONE', #29199 ) ;
#22532 = ORIENTED_EDGE ( 'NONE', *, *, #19923, .T. ) ;
#22533 = CIRCLE ( 'NONE', #25012, 26.80000000000000071 ) ;
#22534 = ADVANCED_FACE ( 'NONE', ( #7646 ), #17243, .F. ) ;
#22535 = VERTEX_POINT ( 'NONE', #5595 ) ;
#22536 = LINE ( 'NONE', #827, #6423 ) ;
#22537 = CARTESIAN_POINT ( 'NONE',  ( -26.05511412830000140, 14.93229958979999950, 222.0000000000000000 ) ) ;
#22538 = CARTESIAN_POINT ( 'NONE',  ( -3.454061855166487671, 0.6016891855815794665, -68.65933259512706854 ) ) ;
#22539 = DIRECTION ( 'NONE',  ( -1.000000000000000000, 0.000000000000000000, 0.000000000000000000 ) ) ;
#22540 = CARTESIAN_POINT ( 'NONE',  ( -20.30396346370000060, 20.00000000000000000, 227.8000000000000114 ) ) ;
#22541 = CARTESIAN_POINT ( 'NONE',  ( 0.2722179827725955126, -28.49915599500044650, 6.079792140000011891 ) ) ;
#22543 = ADVANCED_FACE ( 'NONE', ( #20226 ), #26779, .F. ) ;
#22542 = AXIS2_PLACEMENT_3D ( 'NONE', #15524, #4044, #10818 ) ;
#22544 = CARTESIAN_POINT ( 'NONE',  ( 19.79257030269742756, 19.51192911135138175, 0.8505974720000031297 ) ) ;
#22545 = CARTESIAN_POINT ( 'NONE',  ( -10.00000000000000000, 21.69999999990000106, -70.10000000019999788 ) ) ;
#22546 = ORIENTED_EDGE ( 'NONE', *, *, #11604, .T. ) ;
#22547 = CARTESIAN_POINT ( 'NONE',  ( -2.757905763689965095, 3.954155216896602987, -2.565151354099997505 ) ) ;
#22548 = CARTESIAN_POINT ( 'NONE',  ( 5.503465972402116435, -2.627571514392686769, -20.88180150029999993 ) ) ;
#22549 = DIRECTION ( 'NONE',  ( -4.250489863289427893E-14, -6.005940811918155400E-13, -1.000000000000000000 ) ) ;
#22550 = CARTESIAN_POINT ( 'NONE',  ( 10.00000000000000000, -130.0000000000000000, -42.39999999999999858 ) ) ;
#22551 = CARTESIAN_POINT ( 'NONE',  ( 2.901993252043652660, -2.002183683297082517, -90.77455165165939377 ) ) ;
#22552 = CARTESIAN_POINT ( 'NONE',  ( 22.63992238019999803, -14.34133587289999845, 5.000000000000000000 ) ) ;
#22553 = CARTESIAN_POINT ( 'NONE',  ( -12.47330046629999956, 20.99999999999999645, -55.90292611659999977 ) ) ;
#22554 = EDGE_CURVE ( 'NONE', #22455, #2523, #27459, .T. ) ;
#22555 = VECTOR ( 'NONE', #3881, 1000.000000000000000 ) ;
#22556 = CARTESIAN_POINT ( 'NONE',  ( -3.267430459342683502, -1.335589246056428481, -0.6999999999999783062 ) ) ;
#22557 = CARTESIAN_POINT ( 'NONE',  ( 16.30906683129999735, -8.426343777580001415, 230.6999999999999886 ) ) ;
#22558 = CARTESIAN_POINT ( 'NONE',  ( 23.30309534879319600, -14.60301215399188735, 224.5094458585157327 ) ) ;
#22559 = B_SPLINE_CURVE_WITH_KNOTS ( 'NONE', 3,
 ( #25542, #3825, #18286, #13575, #27893, #5859 ),
 .UNSPECIFIED., .F., .F.,
 ( 4, 2, 4 ),
 ( 0.000000000000000000, 0.2632370136849138675, 0.5264740273698277351 ),
 .UNSPECIFIED. ) ;
#22560 = EDGE_LOOP ( 'NONE', ( #8181, #24542, #13627, #22529 ) ) ;
#22561 = CARTESIAN_POINT ( 'NONE',  ( -5.463799992266447525, -1.435916617982112342, -55.97102360502500318 ) ) ;
#22562 = DIRECTION ( 'NONE',  ( 0.5000000000001898481, -0.8660254037843291286, 0.000000000000000000 ) ) ;
#22563 = CARTESIAN_POINT ( 'NONE',  ( -5.517889265940039145, -2.627421812126006451, -12.97655742010000246 ) ) ;
#22564 = CARTESIAN_POINT ( 'NONE',  ( -18.32611560640161841, 20.54576001036038946, 0.2686742430000332860 ) ) ;
#22565 = AXIS2_PLACEMENT_3D ( 'NONE', #766, #17120, #12244 ) ;
#22566 = CARTESIAN_POINT ( 'NONE',  ( -4.652080607398097811, 0.7875555626376541385, -68.10000000002500542 ) ) ;
#22567 = VERTEX_POINT ( 'NONE', #17853 ) ;
#22568 = EDGE_LOOP ( 'NONE', ( #24887, #14745 ) ) ;
#22569 = CARTESIAN_POINT ( 'NONE',  ( 24.13062658807300664, -13.18986347224536182, 5.913085275126884532 ) ) ;
#22570 =( LENGTH_UNIT ( ) NAMED_UNIT ( * ) SI_UNIT ( .MILLI., .METRE. ) );
#22571 = ORIENTED_EDGE ( 'NONE', *, *, #22912, .F. ) ;
#22572 = CARTESIAN_POINT ( 'NONE',  ( 0.000000000000000000, 0.000000000000000000, 138.3395398250000028 ) ) ;
#22573 = CARTESIAN_POINT ( 'NONE',  ( 1.605176535610508326, -27.75389821387976852, 4.999998581000003384 ) ) ;
#22574 = CARTESIAN_POINT ( 'NONE',  ( -3.351703491987489958, 4.047634511443764183, -62.24933298492499745 ) ) ;
#22575 = CARTESIAN_POINT ( 'NONE',  ( -27.77512470430000135, 2.245670316370000201E-11, 229.2930777930000090 ) ) ;
#22576 = AXIS2_PLACEMENT_3D ( 'NONE', #3564, #10968, #29843 ) ;
#22577 = CARTESIAN_POINT ( 'NONE',  ( -28.12662833602211876, 4.327055432336234020, -0.2432540810000105580 ) ) ;
#22578 = EDGE_CURVE ( 'NONE', #10061, #14789, #742, .T. ) ;
#22579 = LINE ( 'NONE', #8547, #7502 ) ;
#22580 = FILL_AREA_STYLE ('',( #5276 ) ) ;
#22581 = DIRECTION ( 'NONE',  ( 0.000000000000000000, 0.000000000000000000, 1.000000000000000000 ) ) ;
#22582 = VERTEX_POINT ( 'NONE', #2932 ) ;
#22583 = PRODUCT_DEFINITION_CONTEXT ( 'detailed design', #29463, 'design' ) ;
#22584 = ADVANCED_FACE ( 'NONE', ( #1042 ), #18007, .F. ) ;
#22585 = AXIS2_PLACEMENT_3D ( 'NONE', #3999, #1805, #13597 ) ;
#22586 = CARTESIAN_POINT ( 'NONE',  ( 7.908785388650001025, 16.35326433119999834, 231.6999999999999886 ) ) ;
#22587 = EDGE_CURVE ( 'NONE', #1473, #29133, #10903, .T. ) ;
#22588 = VECTOR ( 'NONE', #21765, 1000.000000000000000 ) ;
#22589 = ORIENTED_EDGE ( 'NONE', *, *, #2678, .T. ) ;
#22590 = DIRECTION ( 'NONE',  ( -1.000000000000000000, 5.687697999151106851E-16, -6.771501495036750356E-12 ) ) ;
#22591 = DIRECTION ( 'NONE',  ( 0.000000000000000000, 0.000000000000000000, 1.000000000000000000 ) ) ;
#22592 = FACE_OUTER_BOUND ( 'NONE', #7550, .T. ) ;
#22593 = CARTESIAN_POINT ( 'NONE',  ( 9.999999999961779906, -26.27019589019406709, -25.46727582019148173 ) ) ;
#22594 = CARTESIAN_POINT ( 'NONE',  ( -9.251510797979349832, -25.15273151106422489, 204.8526541494500179 ) ) ;
#22595 = CARTESIAN_POINT ( 'NONE',  ( 3.367430855165096659, -2.595439161230981728, -0.6999999999999992895 ) ) ;
#22596 = CARTESIAN_POINT ( 'NONE',  ( -23.35655559443967988, -15.07705663931308671, 5.680691770000024121 ) ) ;
#22597 = DIRECTION ( 'NONE',  ( -1.000000000000000000, 0.000000000000000000, 0.000000000000000000 ) ) ;
#22598 = ORIENTED_EDGE ( 'NONE', *, *, #13338, .T. ) ;
#22599 = DIRECTION ( 'NONE',  ( -0.000000000000000000, -0.000000000000000000, -1.000000000000000000 ) ) ;
#22600 = LINE ( 'NONE', #20080, #27182 ) ;
#22601 = CARTESIAN_POINT ( 'NONE',  ( 28.50000000000000000, 8.881784197000000993E-16, 222.0000000000000000 ) ) ;
#22602 = CARTESIAN_POINT ( 'NONE',  ( 0.5057536231481192246, -27.79562098839016571, 6.099998581000020792 ) ) ;
#22603 = B_SPLINE_CURVE_WITH_KNOTS ( 'NONE', 5,
 ( #30241, #28766, #30985, #27883, #7220, #9416, #23015, #2505, #15922, #4551, #24066, #28623, #25376, #23171, #18867 ),
 .UNSPECIFIED., .F., .F.,
 ( 6, 3, 3, 3, 6 ),
 ( 0.000000000000000000, 0.09999999999599168410, 0.4000000000011452173, 0.6999999999988546495, 1.000000000000000000 ),
 .UNSPECIFIED. ) ;
#22604 = DIRECTION ( 'NONE',  ( -3.134067079931429195E-12, -0.3568421334038983650, 0.9341647027306021478 ) ) ;
#22605 = VECTOR ( 'NONE', #12424, 1000.000000000000000 ) ;
#22606 = CARTESIAN_POINT ( 'NONE',  ( 7.999999999820811780, -5.927567494231108292, -27.82043365066874685 ) ) ;
#22607 = LINE ( 'NONE', #1045, #18984 ) ;
#22608 = CARTESIAN_POINT ( 'NONE',  ( 4.317698767220935707, -2.252650425851481675, -62.06790713612500099 ) ) ;
#22609 = EDGE_LOOP ( 'NONE', ( #22713, #10197, #1589, #30779 ) ) ;
#22610 = CARTESIAN_POINT ( 'NONE',  ( 18.34331631877363122, 20.00003010481418286, 230.6660856982278176 ) ) ;
#22611 = ORIENTED_EDGE ( 'NONE', *, *, #12289, .T. ) ;
#22612 = CARTESIAN_POINT ( 'NONE',  ( 14.25032083441342934, -27.35421241409322946, 0.9999999950000004745 ) ) ;
#22613 = ORIENTED_EDGE ( 'NONE', *, *, #30993, .T. ) ;
#22614 = LINE ( 'NONE', #29988, #5497 ) ;
#22615 = CARTESIAN_POINT ( 'NONE',  ( 2.020725942269999909, 3.500000000000000000, 229.2412452703699728 ) ) ;
#22616 = CARTESIAN_POINT ( 'NONE',  ( -25.43121960300666728, -8.635379644106548014, 143.2171415880000040 ) ) ;
#22617 = UNCERTAINTY_MEASURE_WITH_UNIT (LENGTH_MEASURE( 1.000000000000000082E-05 ), #10311, 'distance_accuracy_value', 'NONE');
#22618 = CARTESIAN_POINT ( 'NONE',  ( -17.12540385515260866, -26.76244582786289072, -34.03635072686944341 ) ) ;
#22619 = CARTESIAN_POINT ( 'NONE',  ( 10.69999999999999929, -30.00000000000000000, -28.40000000000000213 ) ) ;
#22620 = ADVANCED_FACE ( 'NONE', ( #12032 ), #12177, .F. ) ;
#22621 = CARTESIAN_POINT ( 'NONE',  ( -13.67718144140000014, 20.99999999999999645, -57.16242377749999548 ) ) ;
#22622 = VERTEX_POINT ( 'NONE', #23695 ) ;
#22623 = CARTESIAN_POINT ( 'NONE',  ( 1.126323240140575832, -3.906266603841829443, -44.10000000002498410 ) ) ;
#22624 = CARTESIAN_POINT ( 'NONE',  ( -17.59696597919420213, 10.20816091468181774, -0.6999999989999727834 ) ) ;
#22625 = CARTESIAN_POINT ( 'NONE',  ( 4.266075142677459908, -0.9221078188639819651, -24.29036215650000585 ) ) ;
#22626 = CARTESIAN_POINT ( 'NONE',  ( 23.70259205098650312, -12.50815390746196165, 4.579417934479508290 ) ) ;
#22627 = FACE_OUTER_BOUND ( 'NONE', #27080, .T. ) ;
#22628 = CARTESIAN_POINT ( 'NONE',  ( 0.000000000000000000, 0.000000000000000000, 230.0000000000000000 ) ) ;
#22629 = CARTESIAN_POINT ( 'NONE',  ( -4.848570193085766533, 0.4842359979205582143, -47.62737393802499497 ) ) ;
#22630 = CARTESIAN_POINT ( 'NONE',  ( -2.073454313851444741, -3.273367579595010124, -37.55154403891181403 ) ) ;
#22631 = CARTESIAN_POINT ( 'NONE',  ( -0.5436710233579141738, 2.033405200009645863, 226.6412452697799438 ) ) ;
#22632 = CARTESIAN_POINT ( 'NONE',  ( 10.70000000009999930, -27.00000000000000000, -28.39999999989999679 ) ) ;
#22633 = CARTESIAN_POINT ( 'NONE',  ( -18.95046173579999760, -18.95046173579999760, 43.21714158840000408 ) ) ;
#22634 = CARTESIAN_POINT ( 'NONE',  ( 9.738910687886868089, -24.96785170200598358, 27.99999999999999645 ) ) ;
#22635 = ORIENTED_EDGE ( 'NONE', *, *, #11820, .T. ) ;
#22636 = CARTESIAN_POINT ( 'NONE',  ( 2.635706879431563898, 5.544231365240147369, -32.15113063600000487 ) ) ;
#22637 = ORIENTED_EDGE ( 'NONE', *, *, #26070, .T. ) ;
#22638 = DIRECTION ( 'NONE',  ( 0.000000000000000000, 0.000000000000000000, 1.000000000000000000 ) ) ;
#22639 = CARTESIAN_POINT ( 'NONE',  ( 1.728540313474559387, 5.648005006634932990, -51.94125421262499032 ) ) ;
#22640 = ORIENTED_EDGE ( 'NONE', *, *, #11275, .F. ) ;
#22641 = EDGE_CURVE ( 'NONE', #12690, #11998, #27895, .T. ) ;
#22642 = VERTEX_POINT ( 'NONE', #18955 ) ;
#22643 = CARTESIAN_POINT ( 'NONE',  ( 3.808845017568531777, -24.38903739799846448, -0.05106179917585269845 ) ) ;
#22644 = VERTEX_POINT ( 'NONE', #11721 ) ;
#22645 = EDGE_LOOP ( 'NONE', ( #28227, #56, #7200, #1396 ) ) ;
#22646 = CARTESIAN_POINT ( 'NONE',  ( 24.83401022448529005, 13.98326749045440032, 4.239871879999995485 ) ) ;
#22647 = DIRECTION ( 'NONE',  ( -1.000000000000000000, 5.665498452320000818E-16, 0.000000000000000000 ) ) ;
#22648 = DIRECTION ( 'NONE',  ( -0.7071067811780481493, 0.6644630243965948813, 0.2418447626510653869 ) ) ;
#22649 = CARTESIAN_POINT ( 'NONE',  ( 5.072625435919005586E-16, 3.702906486519338703E-16, 226.6412452697749984 ) ) ;
#22650 = CYLINDRICAL_SURFACE ( 'NONE', #15090, 5.000000000000003553 ) ;
#22651 = CARTESIAN_POINT ( 'NONE',  ( -4.074815451744496109, 2.319135910757860852, -0.6999999999999992895 ) ) ;
#22652 = CARTESIAN_POINT ( 'NONE',  ( 0.8228371056950706253, -6.016286819831330845, -0.3731240480000022619 ) ) ;
#22653 = CARTESIAN_POINT ( 'NONE',  ( -3.147559148823861896, -1.548267634411989002, 227.6488953029183619 ) ) ;
#22654 = CARTESIAN_POINT ( 'NONE',  ( 10.69999999989999928, -25.00000000000000000, -2.399999999999999467 ) ) ;
#22655 = CARTESIAN_POINT ( 'NONE',  ( 1.483810035143914297, 4.536549859444123811, -12.00797964829999742 ) ) ;
#22656 = CARTESIAN_POINT ( 'NONE',  ( 4.556810990865948874, -1.030009251744163468, -32.28377053310000377 ) ) ;
#22657 = ADVANCED_FACE ( 'NONE', ( #30926, #4805 ), #11877, .T. ) ;
#22658 = DIRECTION ( 'NONE',  ( -1.000000000000000000, -1.853796481301025284E-24, -2.257144471330669991E-12 ) ) ;
#22659 = CARTESIAN_POINT ( 'NONE',  ( -24.07583586439999834, -13.90018868249999962, 226.1000014189999945 ) ) ;
#22660 = PLANE ( 'NONE',  #15164 ) ;
#22661 = CARTESIAN_POINT ( 'NONE',  ( -0.4514894588696777289, 4.335480228600245844, -25.88903409329999761 ) ) ;
#22662 = CARTESIAN_POINT ( 'NONE',  ( 18.17095938919667475, 20.37181511208520135, -0.6577119969999878357 ) ) ;
#22663 = LINE ( 'NONE', #1109, #1194 ) ;
#22664 = DIRECTION ( 'NONE',  ( -1.000000000000000000, 0.000000000000000000, 0.000000000000000000 ) ) ;
#22665 = ORIENTED_EDGE ( 'NONE', *, *, #10171, .T. ) ;
#22666 = VERTEX_POINT ( 'NONE', #26201 ) ;
#22667 = CARTESIAN_POINT ( 'NONE',  ( 23.25311087529421172, 15.23597699658644800, 5.310552110000033466 ) ) ;
#22668 = CARTESIAN_POINT ( 'NONE',  ( -24.50000001620000134, 3.000285568850000245E-15, 140.0000000040000145 ) ) ;
#22669 = VECTOR ( 'NONE', #21167, 1000.000000000000227 ) ;
#22670 = ORIENTED_EDGE ( 'NONE', *, *, #5839, .T. ) ;
#22671 = DIRECTION ( 'NONE',  ( 0.000000000000000000, -1.000000000000000000, 0.000000000000000000 ) ) ;
#22672 = CARTESIAN_POINT ( 'NONE',  ( -25.20890834729999952, -13.29605215849999844, 224.6893543200000067 ) ) ;
#22673 = ORIENTED_EDGE ( 'NONE', *, *, #18352, .F. ) ;
#22674 = DIRECTION ( 'NONE',  ( 1.000000000000000000, 0.000000000000000000, 0.000000000000000000 ) ) ;
#22675 = ORIENTED_EDGE ( 'NONE', *, *, #10367, .F. ) ;
#22676 = ADVANCED_FACE ( 'NONE', ( #19423 ), #21755, .T. ) ;
#22677 = ORIENTED_EDGE ( 'NONE', *, *, #12162, .F. ) ;
#22678 = EDGE_LOOP ( 'NONE', ( #5924, #28058, #7892, #20663, #12684 ) ) ;
#22680 = CARTESIAN_POINT ( 'NONE',  ( 26.07656786439999763, 9.132422599079999870, 230.6999999999999886 ) ) ;
#22679 = B_SPLINE_CURVE_WITH_KNOTS ( 'NONE', 3,
 ( #8258, #18009, #17854, #12527, #27615, #17401 ),
 .UNSPECIFIED., .F., .F.,
 ( 4, 2, 4 ),
 ( 0.000000000000000000, 0.5000000000000000000, 1.000000000000000000 ),
 .UNSPECIFIED. ) ;
#22681 = FACE_OUTER_BOUND ( 'NONE', #13175, .T. ) ;
#22682 = CARTESIAN_POINT ( 'NONE',  ( -3.686970300939999667, -0.1862064327014488485, -68.94610314789107974 ) ) ;
#22683 = ORIENTED_EDGE ( 'NONE', *, *, #17508, .T. ) ;
#22684 = CARTESIAN_POINT ( 'NONE',  ( -19.80526803560000104, 19.50877411510000314, 227.3999999999999773 ) ) ;
#22685 = CARTESIAN_POINT ( 'NONE',  ( -24.36725163763869162, -13.38201776504303986, 4.999998581000003384 ) ) ;
#22686 = FACE_OUTER_BOUND ( 'NONE', #30432, .T. ) ;
#22687 = CARTESIAN_POINT ( 'NONE',  ( 26.80000000069999899, -3.281945028320000125E-15, 187.1101814799999943 ) ) ;
#22688 = EDGE_CURVE ( 'NONE', #8060, #24157, #20655, .T. ) ;
#22689 = EDGE_LOOP ( 'NONE', ( #7463, #26401, #3477, #29161 ) ) ;
#22690 = EDGE_CURVE ( 'NONE', #7951, #3809, #16169, .T. ) ;
#22691 = VECTOR ( 'NONE', #4903, 1000.000000000000000 ) ;
#22692 = CARTESIAN_POINT ( 'NONE',  ( 5.530149664617865390, 2.595584118083901881, -2.479170051700001043 ) ) ;
#22693 = CARTESIAN_POINT ( 'NONE',  ( -3.331422745097509797, -2.438398348906448021, -18.37254627010000974 ) ) ;
#22694 = CARTESIAN_POINT ( 'NONE',  ( -1.127665019380000189, -28.47796022459999676, 225.0000014190000002 ) ) ;
#22695 = CARTESIAN_POINT ( 'NONE',  ( 23.96498963411518446, 14.09036522719675411, 6.071979371979260520 ) ) ;
#22696 = CARTESIAN_POINT ( 'NONE',  ( -27.50000000000000000, 3.367667473009999970E-15, 136.3944487260000074 ) ) ;
#22697 = CARTESIAN_POINT ( 'NONE',  ( -28.45771199710000232, 4.798408318400000816, 229.4982322489999831 ) ) ;
#22698 = CARTESIAN_POINT ( 'NONE',  ( -23.81569860410000317, -13.75000000000000000, 223.8999999999999773 ) ) ;
#22699 = EDGE_CURVE ( 'NONE', #10529, #26737, #9039, .T. ) ;
#22700 = CARTESIAN_POINT ( 'NONE',  ( 24.24391315728334817, -12.98049462746314120, 224.3250316511497147 ) ) ;
#22701 = CARTESIAN_POINT ( 'NONE',  ( -26.49971571929999925, -5.074679369350000080, 230.6999999999999886 ) ) ;
#22702 = CARTESIAN_POINT ( 'NONE',  ( 4.646495635265368129, -9.351076805315841511, -32.91834427498756099 ) ) ;
#22703 = VERTEX_POINT ( 'NONE', #17207 ) ;
#22704 = CARTESIAN_POINT ( 'NONE',  ( 4.824840617521342523, -2.656518825645647119, -57.50843849682499354 ) ) ;
#22705 = CARTESIAN_POINT ( 'NONE',  ( -24.26927060885717680, -14.94229635206700380, 6.073751778336542451 ) ) ;
#22706 = B_SPLINE_CURVE_WITH_KNOTS ( 'NONE', 5,
 ( #6315, #28020, #16220, #6464, #28178, #30701 ),
 .UNSPECIFIED., .F., .F.,
 ( 6, 6 ),
 ( 66.69070842060000359, 88.33140247330000250 ),
 .UNSPECIFIED. ) ;
#22707 = CARTESIAN_POINT ( 'NONE',  ( -5.440024667461782037, 2.837840394948672351, -1.418764356299999418 ) ) ;
#22708 = ORIENTED_EDGE ( 'NONE', *, *, #5927, .T. ) ;
#22709 = CARTESIAN_POINT ( 'NONE',  ( -2.998580033872426220, 3.272756371925533703, -39.07539910814716677 ) ) ;
#22710 = EDGE_CURVE ( 'NONE', #10264, #8967, #6495, .T. ) ;
#22711 = CARTESIAN_POINT ( 'NONE',  ( -4.184317568092711603, 0.3509751255880352305, -68.10000000002500542 ) ) ;
#22712 = ORIENTED_EDGE ( 'NONE', *, *, #14737, .F. ) ;
#22713 = ORIENTED_EDGE ( 'NONE', *, *, #10777, .T. ) ;
#22714 = ORIENTED_EDGE ( 'NONE', *, *, #2660, .F. ) ;
#22715 = CARTESIAN_POINT ( 'NONE',  ( 23.86403265466892876, -13.66628296867904346, 6.099999999998879652 ) ) ;
#22716 = CIRCLE ( 'NONE', #17185, 27.92857142860000152 ) ;
#22717 = VERTEX_POINT ( 'NONE', #6180 ) ;
#22718 = CARTESIAN_POINT ( 'NONE',  ( 1.484924240490000047, 1.484924240490000047, 226.6412452697800006 ) ) ;
#22719 = LINE ( 'NONE', #17214, #29035 ) ;
#22720 = CARTESIAN_POINT ( 'NONE',  ( -4.150389416700805079, 1.923785201099232900, -65.37526299422499676 ) ) ;
#22721 = EDGE_CURVE ( 'NONE', #13075, #6979, #23680, .T. ) ;
#22722 = DIRECTION ( 'NONE',  ( 1.000000000000000000, -1.224606353819999829E-16, 0.000000000000000000 ) ) ;
#22723 = B_SPLINE_CURVE_WITH_KNOTS ( 'NONE', 3,
 ( #1057, #3559, #24660, #3094, #5766, #10963, #3251, #12857, #7967, #5917, #5611, #29528 ),
 .UNSPECIFIED., .F., .F.,
 ( 4, 2, 2, 2, 2, 4 ),
 ( 0.000000000000000000, 0.2499999999999658051, 0.3749999999999714673, 0.4999999999999771294, 0.7499999999999885647, 1.000000000000000000 ),
 .UNSPECIFIED. ) ;
#22724 = CARTESIAN_POINT ( 'NONE',  ( -27.29371452669260734, -0.4966198192112916687, -0.6577119969999878357 ) ) ;
#22725 = DIRECTION ( 'NONE',  ( 1.000000000000000000, 0.000000000000000000, 0.000000000000000000 ) ) ;
#22726 = CARTESIAN_POINT ( 'NONE',  ( 8.000000000285856672, -13.61361098174325868, -34.64062768040190576 ) ) ;
#22727 = ORIENTED_EDGE ( 'NONE', *, *, #2406, .F. ) ;
#22728 = CARTESIAN_POINT ( 'NONE',  ( -0.6370991518874399295, 4.292107257743936977, -10.36772091660000861 ) ) ;
#22729 = CARTESIAN_POINT ( 'NONE',  ( 3.858789587625139905, 0.3163803785107239808, 230.6290587881442775 ) ) ;
#22730 = ADVANCED_FACE ( 'NONE', ( #3829 ), #18345, .F. ) ;
#22731 = CARTESIAN_POINT ( 'NONE',  ( 14.56598578705985325, -31.50796871393007947, -31.57082574131231922 ) ) ;
#22732 = AXIS2_PLACEMENT_3D ( 'NONE', #18593, #26151, #23956 ) ;
#22733 = ORIENTED_EDGE ( 'NONE', *, *, #15893, .T. ) ;
#22734 = CARTESIAN_POINT ( 'NONE',  ( 25.00924755590000004, -13.66774366000000107, 224.0987054560000047 ) ) ;
#22735 = CARTESIAN_POINT ( 'NONE',  ( 16.86019302169865952, -7.934232311421240524, -0.6999999999999785283 ) ) ;
#22736 = CARTESIAN_POINT ( 'NONE',  ( 5.361384718770000113, -31.61859215249999977, 222.0000000000000000 ) ) ;
#22737 = CARTESIAN_POINT ( 'NONE',  ( 23.82458380820737531, 13.44211522811278314, 0.000000000000000000 ) ) ;
#22738 = B_SPLINE_CURVE_WITH_KNOTS ( 'NONE', 5,
 ( #25618, #6252, #1381, #13804, #20730, #30329, #13484, #13329, #22772, #15855, #11291, #27803, #8760, #20412, #13647 ),
 .UNSPECIFIED., .F., .F.,
 ( 6, 3, 3, 3, 6 ),
 ( 0.000000000000000000, 0.2999999999999999889, 0.6000000000034357850, 0.8999999999994273692, 1.000000000000000000 ),
 .UNSPECIFIED. ) ;
#22739 = CARTESIAN_POINT ( 'NONE',  ( 16.21708931935714304, -9.573165759297907584, -0.000000000000000000 ) ) ;
#22740 = CARTESIAN_POINT ( 'NONE',  ( -1.078772944755383767, 5.890544393200768170, -60.25324387862499975 ) ) ;
#22741 = CARTESIAN_POINT ( 'NONE',  ( -23.81866442513004856, -14.33570206453694240, 6.099998581000020792 ) ) ;
#22742 = CARTESIAN_POINT ( 'NONE',  ( 22.86552662882814246, -13.97920826333698230, 224.1183286168485722 ) ) ;
#22743 = ORIENTED_EDGE ( 'NONE', *, *, #30860, .F. ) ;
#22744 = CARTESIAN_POINT ( 'NONE',  ( 24.32472894995379420, -13.45989151107506387, 3.899998581000013509 ) ) ;
#22745 = CARTESIAN_POINT ( 'NONE',  ( 27.79999999999999716, -2.355449169040000061E-11, 229.0000000000000000 ) ) ;
#22746 = CARTESIAN_POINT ( 'NONE',  ( -1.599750255664186049, -3.573568845936323068, -68.10000000002501963 ) ) ;
#22747 = EDGE_CURVE ( 'NONE', #7240, #4391, #804, .T. ) ;
#22748 = CARTESIAN_POINT ( 'NONE',  ( 10.98966923329999901, -24.66097101770000322, -1.689678582800002715 ) ) ;
#22749 = EDGE_CURVE ( 'NONE', #17448, #24430, #20875, .T. ) ;
#22750 =( NAMED_UNIT ( * ) PLANE_ANGLE_UNIT ( ) SI_UNIT ( $, .RADIAN. ) );
#22751 = CARTESIAN_POINT ( 'NONE',  ( 14.74466352505797673, -25.67305715492923213, -33.40712347947508931 ) ) ;
#22752 = CARTESIAN_POINT ( 'NONE',  ( 17.93011078765611543, -8.208160914697428368, -0.6999999999999784173 ) ) ;
#22753 = TOROIDAL_SURFACE ( 'NONE', #2170, 29.80000000000000071, 3.000000000000000000 ) ;
#22754 = CARTESIAN_POINT ( 'NONE',  ( -4.543473910928013559, 0.02303893552233737124, -62.97122063472500031 ) ) ;
#22755 = EDGE_LOOP ( 'NONE', ( #28583, #4431 ) ) ;
#22756 = DIRECTION ( 'NONE',  ( -0.7198537139083028835, 0.6941258031311204890, 0.000000000000000000 ) ) ;
#22757 = VERTEX_POINT ( 'NONE', #15938 ) ;
#22758 = CARTESIAN_POINT ( 'NONE',  ( 27.79539923781684507, 0.5057481689249200274, 1.000000000000000888 ) ) ;
#22759 = ORIENTED_EDGE ( 'NONE', *, *, #23671, .F. ) ;
#22760 = DIRECTION ( 'NONE',  ( 0.7071067811865924257, -0.6455034180660765841, 0.2886612846658665466 ) ) ;
#22761 = CARTESIAN_POINT ( 'NONE',  ( 25.45799949673341800, -12.81261086040661645, 4.791562841999996714 ) ) ;
#22762 = CARTESIAN_POINT ( 'NONE',  ( 10.95000000009999930, -27.00000000000000000, -28.39999999989999679 ) ) ;
#22763 = LINE ( 'NONE', #3561, #30905 ) ;
#22764 = CARTESIAN_POINT ( 'NONE',  ( 9.738910687886868089, -24.96785170200598358, 27.99999999999999645 ) ) ;
#22765 = LINE ( 'NONE', #27178, #18543 ) ;
#22766 = ORIENTED_EDGE ( 'NONE', *, *, #25159, .T. ) ;
#22767 = LINE ( 'NONE', #8591, #24046 ) ;
#22768 = CARTESIAN_POINT ( 'NONE',  ( -8.699999999718064814, -24.05685110469877230, -27.69790561507143778 ) ) ;
#22769 = AXIS2_PLACEMENT_3D ( 'NONE', #12024, #23537, #14236 ) ;
#22770 = CARTESIAN_POINT ( 'NONE',  ( -17.93324555108848628, -9.020011617866936504, 0.000000000000000000 ) ) ;
#22771 = CARTESIAN_POINT ( 'NONE',  ( 0.3233900739386466605, 6.101867874933233793, -22.94418644579999977 ) ) ;
#22772 = CARTESIAN_POINT ( 'NONE',  ( -24.43799431770000297, -14.66523353640000060, 226.0028091380000035 ) ) ;
#22773 = MECHANICAL_DESIGN_GEOMETRIC_PRESENTATION_REPRESENTATION (  '', ( #18750 ), #13213 ) ;
#22774 = FACE_OUTER_BOUND ( 'NONE', #10742, .T. ) ;
#22775 = AXIS2_PLACEMENT_3D ( 'NONE', #7982, #6090, #25302 ) ;
#22776 = FACE_OUTER_BOUND ( 'NONE', #15597, .T. ) ;
#22777 = CARTESIAN_POINT ( 'NONE',  ( -23.58385914817347384, -14.71952726119423716, 225.5626237715469529 ) ) ;
#22778 = CARTESIAN_POINT ( 'NONE',  ( 1.728540313474559387, 5.648005006634932990, -50.98125421262499657 ) ) ;
#22779 = CARTESIAN_POINT ( 'NONE',  ( -1.976074114793839431, 0.3084332875059763723, 231.1412452697749984 ) ) ;
#22780 = DIRECTION ( 'NONE',  ( 0.3633921898465272138, -0.9316362575375356503, -1.850371707708593498E-14 ) ) ;
#22781 = CARTESIAN_POINT ( 'NONE',  ( -20.09104791241940546, 19.99996880304969693, 229.7041693757062717 ) ) ;
#22782 = CARTESIAN_POINT ( 'NONE',  ( -25.38111185550165416, -8.615767840674489975, 43.21714158837188080 ) ) ;
#22783 = EDGE_CURVE ( 'NONE', #11991, #22622, #30430, .T. ) ;
#22784 = CARTESIAN_POINT ( 'NONE',  ( 18.26900987441764812, -9.123954215387964695, -4.336808689942017736E-16 ) ) ;
#22785 = EDGE_LOOP ( 'NONE', ( #1080, #16374, #26897, #17962 ) ) ;
#22786 = ADVANCED_FACE ( 'NONE', ( #30259 ), #29942, .F. ) ;
#22788 = B_SPLINE_CURVE_WITH_KNOTS ( 'NONE', 1,
 ( #23909, #30671 ),
 .UNSPECIFIED., .F., .F.,
 ( 2, 2 ),
 ( -2.556819966299999618E-06, 0.7000000000009999335 ),
 .UNSPECIFIED. ) ;
#22787 = CARTESIAN_POINT ( 'NONE',  ( -3.500772897184936561, -3.093025330206538470, -33.83447003410000775 ) ) ;
#22789 = EDGE_CURVE ( 'NONE', #21137, #3582, #30424, .T. ) ;
#22790 = ORIENTED_EDGE ( 'NONE', *, *, #17254, .T. ) ;
#22791 = CARTESIAN_POINT ( 'NONE',  ( -8.699999999678249551, -14.35760254608830522, -33.57685301057431815 ) ) ;
#22792 = CARTESIAN_POINT ( 'NONE',  ( -4.507646854653408752, 2.674235333181991692, -51.58267869292500052 ) ) ;
#22793 = ORIENTED_EDGE ( 'NONE', *, *, #5945, .F. ) ;
#22794 = CIRCLE ( 'NONE', #192, 28.50000000000000000 ) ;
#22795 = SHAPE_DEFINITION_REPRESENTATION ( #5637, #16405 ) ;
#22796 = ORIENTED_EDGE ( 'NONE', *, *, #11925, .T. ) ;
#22797 = B_SPLINE_CURVE_WITH_KNOTS ( 'NONE', 3,
 ( #30570, #23648, #9148, #4443, #19222, #30721, #11982, #2245, #6637, #28807, #4756, #18598 ),
 .UNSPECIFIED., .F., .F.,
 ( 4, 2, 2, 2, 2, 4 ),
 ( 0.000000000000000000, 0.2499999999999998335, 0.4999999999999996669, 0.6250000000000000000, 0.7500000000000003331, 1.000000000000000000 ),
 .UNSPECIFIED. ) ;
#22798 = VERTEX_POINT ( 'NONE', #11067 ) ;
#22799 = PLANE ( 'NONE',  #2722 ) ;
#22800 = CARTESIAN_POINT ( 'NONE',  ( 17.95841148948556310, 10.23646161652002817, 0.000000000000000000 ) ) ;
#22801 = CARTESIAN_POINT ( 'NONE',  ( 5.181945990355393050, 1.017753073738105751, -35.69999999999998863 ) ) ;
#22802 = CARTESIAN_POINT ( 'NONE',  ( -27.79539923781770483, -0.5057481688778011630, 1.000000000000000888 ) ) ;
#22803 = FACE_OUTER_BOUND ( 'NONE', #9314, .T. ) ;
#22804 = CARTESIAN_POINT ( 'NONE',  ( -3.745223230361195643, 2.151215814118476732, -0.6999999999999992895 ) ) ;
#22805 = CARTESIAN_POINT ( 'NONE',  ( 3.206179479465854243, -3.994457159022797299, -2.167821867100002908 ) ) ;
#22806 = CARTESIAN_POINT ( 'NONE',  ( 1.009653006785187435, 1.746192186286544379, 230.8412452699999449 ) ) ;
#22807 = CARTESIAN_POINT ( 'NONE',  ( -10.32522729140000095, -24.79836099970000163, -1.399999999999998579 ) ) ;
#22808 = CARTESIAN_POINT ( 'NONE',  ( -3.941349475653407985, -1.876729865818548282, -13.47655742010000601 ) ) ;
#22809 = CARTESIAN_POINT ( 'NONE',  ( -4.502700345321055231, 3.250786835042839051, -33.46696136359999230 ) ) ;
#22810 = VECTOR ( 'NONE', #27156, 1000.000000000000000 ) ;
#22811 = CARTESIAN_POINT ( 'NONE',  ( -0.7577809307819999285, -5.814680484680000205, 226.6412452697800006 ) ) ;
#22812 = LINE ( 'NONE', #1420, #9266 ) ;
#22813 = CARTESIAN_POINT ( 'NONE',  ( -28.49528339128749010, -0.5184828350248836815, 8.000000000000007105 ) ) ;
#22814 = DIRECTION ( 'NONE',  ( 1.000000000000000000, 0.000000000000000000, 0.000000000000000000 ) ) ;
#22815 = CARTESIAN_POINT ( 'NONE',  ( -3.052438874386664835, 3.509528713898347974, -28.58728588869999143 ) ) ;
#22817 = EDGE_CURVE ( 'NONE', #30998, #25912, #30457, .T. ) ;
#22816 = CIRCLE ( 'NONE', #26835, 2.500000000105230491 ) ;
#22818 = CARTESIAN_POINT ( 'NONE',  ( 22.96035733374347743, -13.82212301974795565, 225.9951937274967690 ) ) ;
#22819 = DIRECTION ( 'NONE',  ( 0.000000000000000000, 0.000000000000000000, -1.000000000000000000 ) ) ;
#22820 = CARTESIAN_POINT ( 'NONE',  ( -27.92857142909999979, 3.420150602519999655E-15, 92.06031501479999690 ) ) ;
#22821 = VERTEX_POINT ( 'NONE', #16246 ) ;
#22822 = ORIENTED_EDGE ( 'NONE', *, *, #17270, .F. ) ;
#22823 = CARTESIAN_POINT ( 'NONE',  ( 24.29089620522634263, 14.90695587088477581, 6.079851352999988023 ) ) ;
#22824 = CARTESIAN_POINT ( 'NONE',  ( 10.49049139470000114, 19.99999999999999645, -1.182260226300003936 ) ) ;
#22825 = B_SPLINE_CURVE_WITH_KNOTS ( 'NONE', 5,
 ( #20720, #14108, #23712, #21345, #30942, #30319, #18359, #5114, #19756 ),
 .UNSPECIFIED., .F., .F.,
 ( 6, 3, 6 ),
 ( 0.000000000000000000, 2.404878242390000143, 3.338999440259999840 ),
 .UNSPECIFIED. ) ;
#22826 = ORIENTED_EDGE ( 'NONE', *, *, #26550, .T. ) ;
#22827 = CARTESIAN_POINT ( 'NONE',  ( 0.8979745064769899532, -3.500000000000000444, 227.7113415996607557 ) ) ;
#22828 = CARTESIAN_POINT ( 'NONE',  ( 3.957198906281382822, -0.01292438418519503696, -37.47286552776822788 ) ) ;
#22829 = ORIENTED_EDGE ( 'NONE', *, *, #11315, .T. ) ;
#22830 = CARTESIAN_POINT ( 'NONE',  ( -8.416763499243886670, -26.18199973230928990, 23.07543701367895039 ) ) ;
#22831 = VERTEX_POINT ( 'NONE', #1476 ) ;
#22832 = ORIENTED_EDGE ( 'NONE', *, *, #24628, .F. ) ;
#22833 = SHAPE_REPRESENTATION ( 'Front End Cap', ( #17722 ), #25295 ) ;
#22834 = ORIENTED_EDGE ( 'NONE', *, *, #6151, .T. ) ;
#22835 = CARTESIAN_POINT ( 'NONE',  ( 17.99935157089999649, 20.17941515460000090, 230.6999999999999886 ) ) ;
#22836 = CIRCLE ( 'NONE', #7758, 27.23548387100000312 ) ;
#22838 = CARTESIAN_POINT ( 'NONE',  ( 8.903108651239925564, -22.82508830966962421, 190.0000000000000000 ) ) ;
#22837 = AXIS2_PLACEMENT_3D ( 'NONE', #25305, #11141, #30657 ) ;
#22839 = VERTEX_POINT ( 'NONE', #20665 ) ;
#22840 = DIRECTION ( 'NONE',  ( -1.000000000000000000, 3.981000000000000101E-12, -1.940999999999999908E-12 ) ) ;
#22841 = CIRCLE ( 'NONE', #18300, 3.176829269159998859 ) ;
#22842 = B_SPLINE_CURVE_WITH_KNOTS ( 'NONE', 3,
 ( #15327, #8072, #24770, #1015 ),
 .UNSPECIFIED., .F., .F.,
 ( 4, 4 ),
 ( 0.000000000000000000, 1.000000000000000000 ),
 .UNSPECIFIED. ) ;
#22843 = AXIS2_PLACEMENT_3D ( 'NONE', #30875, #19063, #18746 ) ;
#22844 = CARTESIAN_POINT ( 'NONE',  ( -2.490109544994508539, -4.523857212610923995, -93.52962329550673815 ) ) ;
#22845 = CARTESIAN_POINT ( 'NONE',  ( -4.276011752185619130, -51.11187400311629858, -27.80500476125005704 ) ) ;
#22846 = CARTESIAN_POINT ( 'NONE',  ( -8.699999999648646565, -16.67007951101791363, -37.94887063592300791 ) ) ;
#22847 = CARTESIAN_POINT ( 'NONE',  ( -0.8958568848300000331, -28.48628573779999940, 225.6801695290000112 ) ) ;
#22848 = EDGE_CURVE ( 'NONE', #10260, #15775, #19152, .T. ) ;
#22849 = EDGE_CURVE ( 'NONE', #13901, #6489, #12821, .T. ) ;
#22850 = CARTESIAN_POINT ( 'NONE',  ( -6.055223678858003389, -2.441925613954294860, -0.9971974345000036433 ) ) ;
#22851 = CARTESIAN_POINT ( 'NONE',  ( -4.661300745830698311, -2.852033519371924619, -20.90799200640000777 ) ) ;
#22852 = LINE ( 'NONE', #11200, #10329 ) ;
#22853 = AXIS2_PLACEMENT_3D ( 'NONE', #30910, #21465, #17043 ) ;
#22854 = CARTESIAN_POINT ( 'NONE',  ( -0.8360625281005691356, -27.48733646094163063, 5.718668015287994955 ) ) ;
#22855 =( GEOMETRIC_REPRESENTATION_CONTEXT ( 3 ) GLOBAL_UNCERTAINTY_ASSIGNED_CONTEXT ( ( #8084 ) ) GLOBAL_UNIT_ASSIGNED_CONTEXT ( ( #18925, #16561, #2560 ) ) REPRESENTATION_CONTEXT ( 'NONE', 'WORKASPACE' ) );
#22856 = CARTESIAN_POINT ( 'NONE',  ( 0.3014737666566600360, -5.198467272794965233, -93.29359154310911606 ) ) ;
#22857 = CARTESIAN_POINT ( 'NONE',  ( -28.04325408110000240, 8.622238390189998484E-15, 230.2432540810000319 ) ) ;
#22858 = CARTESIAN_POINT ( 'NONE',  ( -27.79999999999999716, -2.354540544949999935E-11, 222.0000000000000000 ) ) ;
#22859 = CARTESIAN_POINT ( 'NONE',  ( -0.5944614571882205212, -27.79380703160649446, 4.999998581000003384 ) ) ;
#22860 = ADVANCED_FACE ( 'NONE', ( #2253 ), #5065, .F. ) ;
#22862 = CARTESIAN_POINT ( 'NONE',  ( -27.79999999999999716, 2.356514983149999809E-11, 222.0000000000000000 ) ) ;
#22861 = B_SPLINE_CURVE_WITH_KNOTS ( 'NONE', 3,
 ( #16733, #28235, #23690, #25737, #28400, #11410, #16586, #26196, #18950, #9512 ),
 .UNSPECIFIED., .F., .F.,
 ( 4, 2, 2, 2, 4 ),
 ( 0.000000000000000000, 0.2500000000000000000, 0.5000000000000000000, 0.7500000000000000000, 1.000000000000000000 ),
 .UNSPECIFIED. ) ;
#22863 = CARTESIAN_POINT ( 'NONE',  ( 2.797823115279999939, -26.80098304230000039, 230.6999999999999886 ) ) ;
#22864 = CARTESIAN_POINT ( 'NONE',  ( 5.835777567934348653, -7.528575091604372105, -33.80723775348178606 ) ) ;
#22865 = AXIS2_PLACEMENT_3D ( 'NONE', #14435, #9703, #9231 ) ;
#22866 = VERTEX_POINT ( 'NONE', #1940 ) ;
#22867 = CARTESIAN_POINT ( 'NONE',  ( -4.535753307212162078, -3.367775055652930227, -56.27895058492499913 ) ) ;
#22868 = CARTESIAN_POINT ( 'NONE',  ( 20.30405755279999980, 20.00000000000000000, 229.0000000000000000 ) ) ;
#22869 = EDGE_LOOP ( 'NONE', ( #10839, #23186, #2065, #21063, #9162 ) ) ;
#22870 = VECTOR ( 'NONE', #10258, 1000.000000000000114 ) ;
#22871 = CARTESIAN_POINT ( 'NONE',  ( -5.853056545089267537, 1.703994407032248581, -16.30443125759999745 ) ) ;
#22872 = ORIENTED_EDGE ( 'NONE', *, *, #24498, .T. ) ;
#22873 = CARTESIAN_POINT ( 'NONE',  ( 26.84464185210000053, -3.287411897800000213E-15, 137.4375040469999760 ) ) ;
#22874 = DIRECTION ( 'NONE',  ( 5.962915006522623408E-16, 0.4383711467890811231, 0.8987940462991652613 ) ) ;
#22875 = ORIENTED_EDGE ( 'NONE', *, *, #27460, .T. ) ;
#22876 = EDGE_CURVE ( 'NONE', #18537, #10995, #13553, .T. ) ;
#22877 = B_SPLINE_CURVE_WITH_KNOTS ( 'NONE', 3,
 ( #26250, #19474, #21843, #9714, #26865, #14296 ),
 .UNSPECIFIED., .F., .F.,
 ( 4, 2, 4 ),
 ( 0.000000000000000000, 0.5000000000000000000, 1.000000000000000000 ),
 .UNSPECIFIED. ) ;
#22878 = ORIENTED_EDGE ( 'NONE', *, *, #24709, .T. ) ;
#22879 = VERTEX_POINT ( 'NONE', #26013 ) ;
#22880 = CARTESIAN_POINT ( 'NONE',  ( 0.000000000000000000, 0.000000000000000000, 90.00000000000000000 ) ) ;
#22881 = ORIENTED_EDGE ( 'NONE', *, *, #5949, .T. ) ;
#22882 = FACE_OUTER_BOUND ( 'NONE', #5881, .T. ) ;
#22883 = FACE_OUTER_BOUND ( 'NONE', #6520, .T. ) ;
#22884 = CARTESIAN_POINT ( 'NONE',  ( 2.994727039187459194, -3.426347720743798231, -64.09605006312500564 ) ) ;
#22885 = CARTESIAN_POINT ( 'NONE',  ( -23.04052943119999952, -20.36665827710000087, 229.4485687169999721 ) ) ;
#22886 = CARTESIAN_POINT ( 'NONE',  ( -10.00000000045683990, -24.07808196999473438, -29.18524365307840895 ) ) ;
#22887 = CARTESIAN_POINT ( 'NONE',  ( 10.06419936220000011, 19.99999999999999645, -43.74658025403999773 ) ) ;
#22888 = B_SPLINE_CURVE_WITH_KNOTS ( 'NONE', 3,
 ( #14052, #7272, #31036, #28515, #4134, #2091 ),
 .UNSPECIFIED., .F., .F.,
 ( 4, 2, 4 ),
 ( 0.000000000000000000, 0.5000000000000000000, 1.000000000000000000 ),
 .UNSPECIFIED. ) ;
#22889 = CARTESIAN_POINT ( 'NONE',  ( 2.020725942159999899, -3.500000000000000000, 230.8412452700000017 ) ) ;
#22890 = DIRECTION ( 'NONE',  ( -6.181333986565961785E-12, 0.4082287037029530552, 0.9128796883888953273 ) ) ;
#22891 = ORIENTED_EDGE ( 'NONE', *, *, #22587, .T. ) ;
#22892 = CARTESIAN_POINT ( 'NONE',  ( 1.888485499342153151, 5.773790730162923879, -10.47047964830000133 ) ) ;
#22893 = CARTESIAN_POINT ( 'NONE',  ( 24.49145441566124148, -14.57548795709913847, 4.319167818000013703 ) ) ;
#22894 = PRODUCT_DEFINITION_SHAPE ( 'NONE', 'NONE',  #8875 ) ;
#22895 = CARTESIAN_POINT ( 'NONE',  ( 14.76418395427435115, -30.55463420411378905, -32.12123367718280775 ) ) ;
#22896 = ORIENTED_EDGE ( 'NONE', *, *, #23830, .T. ) ;
#22897 = CARTESIAN_POINT ( 'NONE',  ( 24.26025373720000289, -13.57556515269999942, 223.9575271749999672 ) ) ;
#22898 = CARTESIAN_POINT ( 'NONE',  ( 27.50000000000000000, -3.367667472999999580E-15, 230.0000000000000000 ) ) ;
#22899 = CARTESIAN_POINT ( 'NONE',  ( 0.000000000000000000, 0.000000000000000000, 115.0000000000000000 ) ) ;
#22900 = EDGE_CURVE ( 'NONE', #13409, #16204, #6285, .T. ) ;
#22901 = B_SPLINE_CURVE_WITH_KNOTS ( 'NONE', 3,
 ( #13698, #28012, #6455, #3791, #1592, #28169, #25668, #18089, #11180, #30542 ),
 .UNSPECIFIED., .F., .F.,
 ( 4, 2, 2, 2, 4 ),
 ( 0.000000000000000000, 0.2500000000000000000, 0.5000000000000000000, 0.7500000000000000000, 1.000000000000000000 ),
 .UNSPECIFIED. ) ;
#22902 = CARTESIAN_POINT ( 'NONE',  ( 26.60345577955319030, 9.630787818574999548, 0.5514269530000337483 ) ) ;
#22903 = CARTESIAN_POINT ( 'NONE',  ( 8.000000000467634820, -18.45959768780296173, -35.96628083219813021 ) ) ;
#22904 = CARTESIAN_POINT ( 'NONE',  ( -3.130203125555106158, 5.106303518385050033, -45.05531229042499319 ) ) ;
#22905 = CARTESIAN_POINT ( 'NONE',  ( -11.30445666259999982, -24.42656469639999983, -1.476955128299997533 ) ) ;
#22906 = CARTESIAN_POINT ( 'NONE',  ( 2.910383045670000247E-11, 21.70000000000000284, -60.10000000000000142 ) ) ;
#22907 = PRODUCT_DEFINITION_FORMATION_WITH_SPECIFIED_SOURCE ( 'ANY', '', #3799, .NOT_KNOWN. ) ;
#22908 = ORIENTED_EDGE ( 'NONE', *, *, #22876, .F. ) ;
#22909 =( LENGTH_UNIT ( ) NAMED_UNIT ( * ) SI_UNIT ( .MILLI., .METRE. ) );
#22910 = CARTESIAN_POINT ( 'NONE',  ( 27.79999999999999716, -2.355691128989999990E-11, 226.2000000000000171 ) ) ;
#22911 = CARTESIAN_POINT ( 'NONE',  ( 2.793573553951601340, -3.441440452430771568, -68.10000000002499121 ) ) ;
#22912 = EDGE_CURVE ( 'NONE', #9163, #14716, #16865, .T. ) ;
#22913 = EDGE_CURVE ( 'NONE', #13351, #19505, #9389, .T. ) ;
#22914 = DIRECTION ( 'NONE',  ( -0.9316362575375349842, 0.3633921898465292122, -0.000000000000000000 ) ) ;
#22915 = CARTESIAN_POINT ( 'NONE',  ( -4.226820258076031678, 0.7562225394961105129, -44.10000000002500542 ) ) ;
#22916 = CARTESIAN_POINT ( 'NONE',  ( 14.77468706462266823, -23.51133457270864469, -32.15902938297210767 ) ) ;
#22917 = DIRECTION ( 'NONE',  ( 0.000000000000000000, 1.000000000000000000, 0.000000000000000000 ) ) ;
#22918 = ADVANCED_FACE ( 'NONE', ( #4598 ), #21135, .F. ) ;
#22919 = CARTESIAN_POINT ( 'NONE',  ( 3.609030021535462041, -4.129188278801706247, -65.29605006312499427 ) ) ;
#22920 = VERTEX_POINT ( 'NONE', #28673 ) ;
#22921 = CARTESIAN_POINT ( 'NONE',  ( -8.699999999731478084, -27.30911655878985300, -25.39023929165498572 ) ) ;
#22922 = EDGE_CURVE ( 'NONE', #24004, #16204, #4765, .T. ) ;
#22923 = VERTEX_POINT ( 'NONE', #26319 ) ;
#22924 = CARTESIAN_POINT ( 'NONE',  ( -19.75038721057206104, -20.61365289012606539, 0.02487544599999447215 ) ) ;
#22925 = EDGE_LOOP ( 'NONE', ( #25992, #12765, #6725, #13902, #2864, #23167, #20152 ) ) ;
#22926 = CARTESIAN_POINT ( 'NONE',  ( -23.82471740849593544, -15.64077206322649083, 4.791628272000025390 ) ) ;
#22927 = CARTESIAN_POINT ( 'NONE',  ( 25.44662323365202639, -12.83524168329857318, 4.689351482000003735 ) ) ;
#22928 = CARTESIAN_POINT ( 'NONE',  ( 2.374791981039476862, 2.610414167372405281, 0.000000000000000000 ) ) ;
#22929 = CARTESIAN_POINT ( 'NONE',  ( -27.83860952016654622, 1.869044697291038615, 8.000000000000007105 ) ) ;
#22930 = EDGE_CURVE ( 'NONE', #18537, #29947, #24778, .T. ) ;
#22931 = CARTESIAN_POINT ( 'NONE',  ( -12.41253550772600889, -21.99999999999999645, -27.03345770352192545 ) ) ;
#22932 = FACE_OUTER_BOUND ( 'NONE', #22289, .T. ) ;
#22933 = ORIENTED_EDGE ( 'NONE', *, *, #12057, .F. ) ;
#22934 = CARTESIAN_POINT ( 'NONE',  ( 18.82264457159015691, 10.97998838177520931, 0.05106179917585291356 ) ) ;
#22935 = CARTESIAN_POINT ( 'NONE',  ( 27.92857142909999979, -3.420150602509999660E-15, 137.9396849850000137 ) ) ;
#22936 = CYLINDRICAL_SURFACE ( 'NONE', #13290, 1.700000000000000178 ) ;
#22937 = CARTESIAN_POINT ( 'NONE',  ( -2.215775945506506250, -3.162163484183925899, 230.6362108339131680 ) ) ;
#22938 = CARTESIAN_POINT ( 'NONE',  ( 6.585786437629999490, -15.73107082825028336, -76.73232662853232000 ) ) ;
#22939 = DIRECTION ( 'NONE',  ( 0.7071067811870488384, 0.000000000000000000, 0.7071067811860461960 ) ) ;
#22940 = CARTESIAN_POINT ( 'NONE',  ( 8.700000000248305554, -25.92947359976189503, -31.20249410819006286 ) ) ;
#22941 = CARTESIAN_POINT ( 'NONE',  ( -19.53673505992006554, -20.39066108913833020, 0.000000000000000000 ) ) ;
#22942 = CARTESIAN_POINT ( 'NONE',  ( -5.649653782182448403, -1.974543963569185046, -50.40743646232499486 ) ) ;
#22943 = EDGE_CURVE ( 'NONE', #5895, #5911, #9631, .T. ) ;
#22944 = CARTESIAN_POINT ( 'NONE',  ( -17.28128630822742196, 12.01496581067445213, -1.400000000000002132 ) ) ;
#22945 = CARTESIAN_POINT ( 'NONE',  ( -20.30396346370000060, 20.00000000000000000, 229.0000000000000000 ) ) ;
#22946 = CARTESIAN_POINT ( 'NONE',  ( -20.28212397553859603, 20.00001296311320687, 229.2653906922940621 ) ) ;
#22947 = CARTESIAN_POINT ( 'NONE',  ( -10.35000000029999967, -25.00000000000000000, -7.274962170099999348 ) ) ;
#22948 = CARTESIAN_POINT ( 'NONE',  ( 18.05835842962944682, -9.659886890379860702, -4.336808689942018722E-16 ) ) ;
#22949 = ORIENTED_EDGE ( 'NONE', *, *, #27366, .T. ) ;
#22950 = CARTESIAN_POINT ( 'NONE',  ( -4.502700345321055231, 3.250786835042839051, -35.46696136359999940 ) ) ;
#22951 = ORIENTED_EDGE ( 'NONE', *, *, #26517, .T. ) ;
#22952 = CARTESIAN_POINT ( 'NONE',  ( 3.630871288588910506, -4.685987307826644965, -52.98430438132500342 ) ) ;
#22953 = VERTEX_POINT ( 'NONE', #14205 ) ;
#22954 = B_SPLINE_CURVE_WITH_KNOTS ( 'NONE', 3,
 ( #4380, #13986, #25478, #2181, #13668, #23273, #9092, #30815, #28142, #18853, #18691, #28450, #16025, #18540, #1717, #16487, #6581, #11314, #16181, #26100, #3915, #30187, #8619, #18216, #25793, #4228 ),
 .UNSPECIFIED., .F., .F.,
 ( 4, 2, 2, 1, 1, 2, 2, 2, 2, 2, 1, 1, 2, 2, 4 ),
 ( 0.000000000000000000, 0.1250000000000079659, 0.1875000000000115463, 0.2187500000000133504, 0.2343750000000146549, 0.2421875000000145162, 0.2500000000000143774, 0.5000000000000217604, 0.6250000000000255351, 0.6875000000000281997, 0.7187500000000304201, 0.7343750000000323075, 0.7421875000000323075, 0.7500000000000323075, 1.000000000000000000 ),
 .UNSPECIFIED. ) ;
#22955 = ITEM_DEFINED_TRANSFORMATION ( 'NONE', 'NONE', #28916,  #17722 ) ;
#22956 = EDGE_LOOP ( 'NONE', ( #19227, #13503, #2558, #30826 ) ) ;
#22957 = ORIENTED_EDGE ( 'NONE', *, *, #1176, .T. ) ;
#22958 = CARTESIAN_POINT ( 'NONE',  ( -17.75159883754878720, -9.616676199626787991, 0.000000000000000000 ) ) ;
#22959 = CARTESIAN_POINT ( 'NONE',  ( 23.50667118420000179, -14.84174322970000048, 225.0000014190000002 ) ) ;
#22960 = CARTESIAN_POINT ( 'NONE',  ( -9.872542079070584009, -130.0000000000000000, -42.90521570519508288 ) ) ;
#22961 = CIRCLE ( 'NONE', #3359, 2.299999999990001598 ) ;
#22962 = LINE ( 'NONE', #3594, #16458 ) ;
#22963 = CARTESIAN_POINT ( 'NONE',  ( 2.131628207279999844E-14, -1.704192342799999938E-14, 231.6999999999999886 ) ) ;
#22964 = EDGE_CURVE ( 'NONE', #8453, #17781, #1913, .T. ) ;
#22965 = FACE_OUTER_BOUND ( 'NONE', #22066, .T. ) ;
#22966 = CARTESIAN_POINT ( 'NONE',  ( -0.8661127261961210078, -4.701195862525644031, -2.587734013000004829 ) ) ;
#22967 = CARTESIAN_POINT ( 'NONE',  ( -2.449212707639999657E-16, 2.000000000000000000, 230.8412452696274499 ) ) ;
#22968 = CARTESIAN_POINT ( 'NONE',  ( 25.39337327713160519, -12.94027895695280250, 5.560810203903397309 ) ) ;
#22969 = EDGE_CURVE ( 'NONE', #17736, #19467, #27757, .T. ) ;
#22970 = CARTESIAN_POINT ( 'NONE',  ( 0.7763070146520694159, 4.277613328189615594, -14.52400681850000730 ) ) ;
#22971 = CARTESIAN_POINT ( 'NONE',  ( -26.80000000069999899, 3.281945028329999726E-15, 211.6085707940000020 ) ) ;
#22972 = EDGE_CURVE ( 'NONE', #3831, #15866, #19699, .T. ) ;
#22973 = EDGE_CURVE ( 'NONE', #2672, #29525, #29597, .T. ) ;
#22974 = CARTESIAN_POINT ( 'NONE',  ( 5.729936103070000009, -1.681209052119999825, 226.6412452697800006 ) ) ;
#22975 = DIRECTION ( 'NONE',  ( -3.112440860597585673E-12, -0.3322662713817149949, 0.9431856258987901809 ) ) ;
#22976 = CARTESIAN_POINT ( 'NONE',  ( -19.80535397421925481, 19.50875616500616871, 0.9999999989999952543 ) ) ;
#22977 = CARTESIAN_POINT ( 'NONE',  ( -7.999999999636759895, -22.42568788229198873, -40.05522481832764470 ) ) ;
#22978 = CARTESIAN_POINT ( 'NONE',  ( -2.385386868421338402, 2.867855126291142476, 227.7701677845706740 ) ) ;
#22979 = CARTESIAN_POINT ( 'NONE',  ( 24.92980816059056082, 14.06569599973778395, -0.2432540810000105580 ) ) ;
#22980 = DIRECTION ( 'NONE',  ( 0.000000000000000000, -0.4794255386042040601, -0.8775825618903722036 ) ) ;
#22981 = FACE_OUTER_BOUND ( 'NONE', #1624, .T. ) ;
#22982 = ORIENTED_EDGE ( 'NONE', *, *, #22411, .T. ) ;
#22983 = CARTESIAN_POINT ( 'NONE',  ( 23.82471740507292068, 15.64077205896351508, 5.208368893000026034 ) ) ;
#22984 = CARTESIAN_POINT ( 'NONE',  ( 10.00000000020000002, 19.99999999999999645, -2.400000000399998612 ) ) ;
#22985 = ORIENTED_EDGE ( 'NONE', *, *, #21022, .T. ) ;
#22986 = AXIS2_PLACEMENT_3D ( 'NONE', #2071, #30864, #14182 ) ;
#22987 = CARTESIAN_POINT ( 'NONE',  ( 1.636264169889315223, -3.499999999999998668, 227.8479073241728088 ) ) ;
#22988 = CARTESIAN_POINT ( 'NONE',  ( -24.58975347950000057, -12.96948186770000078, 224.6893543200000067 ) ) ;
#22989 = CARTESIAN_POINT ( 'NONE',  ( 1.199321674214643529, -5.002983764577906278, -0.6999981557156819134 ) ) ;
#22990 = ORIENTED_EDGE ( 'NONE', *, *, #18153, .F. ) ;
#22991 = LINE ( 'NONE', #25353, #20527 ) ;
#22992 = ORIENTED_EDGE ( 'NONE', *, *, #12412, .F. ) ;
#22993 = EDGE_LOOP ( 'NONE', ( #14339, #30628, #12689, #14168 ) ) ;
#22994 =( LENGTH_UNIT ( ) NAMED_UNIT ( * ) SI_UNIT ( .MILLI., .METRE. ) );
#22995 = ORIENTED_EDGE ( 'NONE', *, *, #7191, .F. ) ;
#22996 = CARTESIAN_POINT ( 'NONE',  ( 3.659488124655024599, -0.9781774386366028917, -35.69999999999999574 ) ) ;
#22997 = VERTEX_POINT ( 'NONE', #2858 ) ;
#22998 = CARTESIAN_POINT ( 'NONE',  ( -24.07583586439999834, -13.90018868249999962, 226.1000014189999945 ) ) ;
#22999 = VERTEX_POINT ( 'NONE', #12448 ) ;
#23000 = CARTESIAN_POINT ( 'NONE',  ( 1.271866015585619403, 3.874426768252950737, -35.70000000000000284 ) ) ;
#23001 = B_SPLINE_CURVE_WITH_KNOTS ( 'NONE', 3,
 ( #21001, #2115, #18940, #30751, #23055, #23529, #13919, #21154, #18629, #1499, #9179, #28226, #1651, #14078, #18475, #30450, #4476, #26036 ),
 .UNSPECIFIED., .F., .F.,
 ( 4, 2, 2, 2, 2, 2, 2, 2, 4 ),
 ( 0.000000000000000000, 0.1249999999999993061, 0.2499999999999986122, 0.3749999999999986122, 0.4999999999999986677, 0.6249999999999987788, 0.7499999999999991118, 0.8749999999999995559, 1.000000000000000000 ),
 .UNSPECIFIED. ) ;
#23002 = CARTESIAN_POINT ( 'NONE',  ( -5.152255138076724528, 6.459217791357691141, -40.62954018461207539 ) ) ;
#23003 = ORIENTED_EDGE ( 'NONE', *, *, #16155, .T. ) ;
#23004 = CARTESIAN_POINT ( 'NONE',  ( 5.656593618302459880, -26.91642256435905622, 209.2180597379770290 ) ) ;
#23005 = CARTESIAN_POINT ( 'NONE',  ( 4.041451884329999800, 2.701186720849999812E-16, 227.9588918784999976 ) ) ;
#23006 = LINE ( 'NONE', #25202, #3438 ) ;
#23007 = ORIENTED_EDGE ( 'NONE', *, *, #18618, .T. ) ;
#23008 = VECTOR ( 'NONE', #19277, 1000.000000000000000 ) ;
#23009 = CARTESIAN_POINT ( 'NONE',  ( -2.507187057889202819, 3.594686560818132204, -2.127651354099999725 ) ) ;
#23010 = CARTESIAN_POINT ( 'NONE',  ( -4.121720561938956529, -3.673096573571036139, -23.84101932449999950 ) ) ;
#23011 = CARTESIAN_POINT ( 'NONE',  ( 10.99289321870000080, 19.99999999999999645, -1.692893218799999877 ) ) ;
#23012 = AXIS2_PLACEMENT_3D ( 'NONE', #15983, #23701, #4496 ) ;
#23013 = AXIS2_PLACEMENT_3D ( 'NONE', #8981, #6782, #9131 ) ;
#23014 = EDGE_CURVE ( 'NONE', #8508, #10260, #30915, .T. ) ;
#23015 = CARTESIAN_POINT ( 'NONE',  ( 24.54884435365858053, -13.04717673649832044, 6.002806400000004317 ) ) ;
#23016 = CARTESIAN_POINT ( 'NONE',  ( 3.458129700891746428, -0.5397582531192768318, -88.52261276316077954 ) ) ;
#23017 = CARTESIAN_POINT ( 'NONE',  ( -27.48714010850000022, 9.611077580710000845, 229.2404163060000144 ) ) ;
#23018 = CARTESIAN_POINT ( 'NONE',  ( -19.29999999990000248, -28.85405481559000052, -28.92454911413899765 ) ) ;
#23019 = CARTESIAN_POINT ( 'NONE',  ( 9.999999999984520827, -128.8192055971804564, -36.36585972525736565 ) ) ;
#23020 = B_SPLINE_CURVE_WITH_KNOTS ( 'NONE', 3,
 ( #17291, #14786, #29095, #24225, #482, #10064, #26898, #15093, #2667, #12263 ),
 .UNSPECIFIED., .F., .F.,
 ( 4, 2, 2, 2, 4 ),
 ( 0.000000000000000000, 0.2500000000000000000, 0.5000000000000000000, 0.7500000000000000000, 1.000000000000000000 ),
 .UNSPECIFIED. ) ;
#23021 = FACE_BOUND ( 'NONE', #9482, .T. ) ;
#23022 = CARTESIAN_POINT ( 'NONE',  ( 26.63560679380000096, -3.754777938270000170, 230.6999999999999886 ) ) ;
#23023 = CARTESIAN_POINT ( 'NONE',  ( -3.552713678799999608E-15, -3.552713678799999608E-15, 143.2171415880000040 ) ) ;
#23024 = VERTEX_POINT ( 'NONE', #24724 ) ;
#23025 = CARTESIAN_POINT ( 'NONE',  ( -3.468517234904584079, -2.575357395510375902, -55.87895058492500766 ) ) ;
#23026 = CARTESIAN_POINT ( 'NONE',  ( 20.30405755279999980, 20.00000000000000000, 228.1999999569999886 ) ) ;
#23027 = ORIENTED_EDGE ( 'NONE', *, *, #10171, .F. ) ;
#23028 = AXIS2_PLACEMENT_3D ( 'NONE', #11800, #26275, #4720 ) ;
#23029 = CARTESIAN_POINT ( 'NONE',  ( 5.466312515054250198, -2.792605348973308477, -11.91474735220000092 ) ) ;
#23030 = ORIENTED_EDGE ( 'NONE', *, *, #22299, .T. ) ;
#23031 = CARTESIAN_POINT ( 'NONE',  ( -24.32472894358752313, 13.45989150749028873, 3.899998581000013509 ) ) ;
#23032 = DIRECTION ( 'NONE',  ( -1.000000000000000000, 0.000000000000000000, 0.000000000000000000 ) ) ;
#23033 = ORIENTED_EDGE ( 'NONE', *, *, #26186, .T. ) ;
#23034 = EDGE_CURVE ( 'NONE', #9298, #17407, #27368, .T. ) ;
#23035 = ORIENTED_EDGE ( 'NONE', *, *, #2961, .T. ) ;
#23036 = VERTEX_POINT ( 'NONE', #12304 ) ;
#23037 = TOROIDAL_SURFACE ( 'NONE', #23542, 30.50000000000000000, 3.000000000000000000 ) ;
#23038 = CARTESIAN_POINT ( 'NONE',  ( -26.80000000000002203, -1.754055898254307966, 186.7828584129167098 ) ) ;
#23039 = SHAPE_DEFINITION_REPRESENTATION ( #25744, #2712 ) ;
#23040 = VERTEX_POINT ( 'NONE', #12604 ) ;
#23041 = CARTESIAN_POINT ( 'NONE',  ( -8.699999999651764071, -17.54044037066235617, -37.48861203924890617 ) ) ;
#23042 = TOROIDAL_SURFACE ( 'NONE', #22053, 24.50000000000000000, 4.000000000000000000 ) ;
#23043 = FACE_OUTER_BOUND ( 'NONE', #18682, .T. ) ;
#23044 = CARTESIAN_POINT ( 'NONE',  ( -1.746607907818665817, 4.818926816502865584, -68.35099036452500343 ) ) ;
#23045 = ADVANCED_FACE ( 'NONE', ( #7725 ), #8031, .T. ) ;
#23046 = CARTESIAN_POINT ( 'NONE',  ( -22.65095495759999977, -20.02231963160000205, 229.9172003479999660 ) ) ;
#23047 = CARTESIAN_POINT ( 'NONE',  ( 7.312007425309012376, -6.582071621330287670, -34.26887834112514497 ) ) ;
#23048 = LINE ( 'NONE', #5877, #13544 ) ;
#23049 = CARTESIAN_POINT ( 'NONE',  ( 17.16657240421717390, -9.000000000001264766, -0.6999999999999784173 ) ) ;
#23050 = ORIENTED_EDGE ( 'NONE', *, *, #5279, .T. ) ;
#23051 = FACE_BOUND ( 'NONE', #20832, .T. ) ;
#23052 = AXIS2_PLACEMENT_3D ( 'NONE', #27788, #18022, #17866 ) ;
#23053 = CARTESIAN_POINT ( 'NONE',  ( 0.8539377161337347033, 4.705374660993639324, -13.08650681850000730 ) ) ;
#23054 = DIRECTION ( 'NONE',  ( -1.000000000000000000, 1.853796481301025284E-24, -2.257144471330669991E-12 ) ) ;
#23055 = CARTESIAN_POINT ( 'NONE',  ( -10.69999999968668725, -24.44066548255720761, -30.36604956106650377 ) ) ;
#23056 = ORIENTED_EDGE ( 'NONE', *, *, #6937, .F. ) ;
#23057 = CARTESIAN_POINT ( 'NONE',  ( 24.07552037900000030, -13.90000980950000020, 223.9000014189999774 ) ) ;
#23058 = VECTOR ( 'NONE', #30219, 1000.000000000000000 ) ;
#23059 = CARTESIAN_POINT ( 'NONE',  ( -24.75645986059670278, -14.12045945564184279, 5.901294544000013076 ) ) ;
#23060 = CARTESIAN_POINT ( 'NONE',  ( -28.46654375369999812, 1.746771098880000261, 222.0000000000000000 ) ) ;
#23061 = CARTESIAN_POINT ( 'NONE',  ( -23.81866442513186755, -14.33570206443695838, 3.899998581000013509 ) ) ;
#23062 = DIRECTION ( 'NONE',  ( 0.000000000000000000, 0.000000000000000000, -1.000000000000000000 ) ) ;
#23063 = CARTESIAN_POINT ( 'NONE',  ( 5.643028086411650435, 2.011589847869324377, -45.92627377572500080 ) ) ;
#23064 = VECTOR ( 'NONE', #2960, 1000.000000000000227 ) ;
#23065 = CARTESIAN_POINT ( 'NONE',  ( -11.14649459219999983, -24.37257237719999736, -0.7852065530999998710 ) ) ;
#23066 = FACE_OUTER_BOUND ( 'NONE', #4136, .T. ) ;
#23067 = EDGE_LOOP ( 'NONE', ( #9754, #14017 ) ) ;
#23068 = EDGE_CURVE ( 'NONE', #13449, #2398, #21749, .T. ) ;
#23069 = PLANE ( 'NONE',  #27348 ) ;
#23070 = CARTESIAN_POINT ( 'NONE',  ( 22.83442928010000017, 16.43389279790000046, 227.5999999999999943 ) ) ;
#23071 = CARTESIAN_POINT ( 'NONE',  ( 1.895713493160553487, -3.707174971585335488, -68.10000000002500542 ) ) ;
#23072 = CONICAL_SURFACE ( 'NONE', #2474, 0.9999999999991018296, 0.7853981633970000820 ) ;
#23073 = LINE ( 'NONE', #14405, #23825 ) ;
#23074 = CARTESIAN_POINT ( 'NONE',  ( -24.34663841809999951, -12.78636765230000094, 225.0000000000000000 ) ) ;
#23075 =( NAMED_UNIT ( * ) PLANE_ANGLE_UNIT ( ) SI_UNIT ( $, .RADIAN. ) );
#23076 = CARTESIAN_POINT ( 'NONE',  ( 8.000000000281330514, -5.981227587277713198, -27.94042817480428198 ) ) ;
#23077 = DIRECTION ( 'NONE',  ( 0.3633921898465289901, 0.9316362575375348731, -8.673617379884029161E-15 ) ) ;
#23078 = CARTESIAN_POINT ( 'NONE',  ( -5.973670867983248201, -0.3179945487330332332, -65.56421022022500722 ) ) ;
#23079 = VERTEX_POINT ( 'NONE', #27086 ) ;
#23080 = ADVANCED_FACE ( 'NONE', ( #363 ), #5522, .F. ) ;
#23081 = CARTESIAN_POINT ( 'NONE',  ( 20.21755947467096348, 19.99998237122240496, 229.4578303307542910 ) ) ;
#23082 = ORIENTED_EDGE ( 'NONE', *, *, #28825, .T. ) ;
#23083 = B_SPLINE_CURVE_WITH_KNOTS ( 'NONE', 1,
 ( #22480, #27493 ),
 .UNSPECIFIED., .F., .F.,
 ( 2, 2 ),
 ( -2.556331278550000249E-06, 0.7000000000009999335 ),
 .UNSPECIFIED. ) ;
#23085 = CARTESIAN_POINT ( 'NONE',  ( -2.521519673230186775, -3.017545703797773538, -44.16141975532499941 ) ) ;
#23084 = TOROIDAL_SURFACE ( 'NONE', #27095, 24.50000000000000000, 4.000000000000000000 ) ;
#23086 = VERTEX_POINT ( 'NONE', #5829 ) ;
#23087 = CARTESIAN_POINT ( 'NONE',  ( 9.999999999969999109, -82.23832021929999314, -29.25398675779999991 ) ) ;
#23088 = DIRECTION ( 'NONE',  ( 1.734723475976806503E-15, 1.000000000000000000, 0.000000000000000000 ) ) ;
#23089 = DIRECTION ( 'NONE',  ( 1.000000000000000000, -1.843431230201421806E-12, 2.650498504952891752E-12 ) ) ;
#23090 = CARTESIAN_POINT ( 'NONE',  ( -10.69999999999999929, -27.00000000000000000, -28.40000000000000213 ) ) ;
#23091 = CYLINDRICAL_SURFACE ( 'NONE', #1772, 2.500000000000002220 ) ;
#23092 = FACE_OUTER_BOUND ( 'NONE', #27769, .T. ) ;
#23093 = CARTESIAN_POINT ( 'NONE',  ( -24.68204616399999907, -14.25020164319999871, 226.1000014189999945 ) ) ;
#23094 = ORIENTED_EDGE ( 'NONE', *, *, #27196, .T. ) ;
#23095 = CARTESIAN_POINT ( 'NONE',  ( -1.728989203319513779, -3.523396336957824282, -44.10000000002498410 ) ) ;
#23096 = EDGE_CURVE ( 'NONE', #8364, #21606, #17173, .T. ) ;
#23097 = CARTESIAN_POINT ( 'NONE',  ( -1.976074114793839431, 0.3084332875059763723, 226.6412452697749984 ) ) ;
#23098 = CARTESIAN_POINT ( 'NONE',  ( 10.69999999930000101, -30.49251257979999963, -21.04205368479999905 ) ) ;
#23099 = EDGE_CURVE ( 'NONE', #15627, #14439, #9944, .T. ) ;
#23100 = CARTESIAN_POINT ( 'NONE',  ( -3.650178114498183746, 0.6777060490173741902, 230.7147300523249100 ) ) ;
#23101 = DIRECTION ( 'NONE',  ( 1.635844237846128888E-12, 0.6889064844488322903, 0.7248502298298253876 ) ) ;
#23102 = CARTESIAN_POINT ( 'NONE',  ( -10.00000000070000183, -27.00000000000000000, -28.40000000000000213 ) ) ;
#23103 = CARTESIAN_POINT ( 'NONE',  ( -0.9598841924169057016, -27.48329941561060252, 225.5561643546540722 ) ) ;
#23104 = CARTESIAN_POINT ( 'NONE',  ( -17.09439379194196817, 9.921746937126174615, -1.400000000000001910 ) ) ;
#23105 = CARTESIAN_POINT ( 'NONE',  ( -4.064488300603595228, -4.392874523441014034, -49.71612412472499187 ) ) ;
#23106 = VECTOR ( 'NONE', #30152, 1000.000000000000000 ) ;
#23107 = EDGE_CURVE ( 'NONE', #1493, #20367, #7227, .T. ) ;
#23108 = AXIS2_PLACEMENT_3D ( 'NONE', #22845, #5537, #19875 ) ;
#23109 = CARTESIAN_POINT ( 'NONE',  ( -23.25354871329894024, -14.68148953537939860, 5.217924949212490837 ) ) ;
#23110 = CARTESIAN_POINT ( 'NONE',  ( -6.999999999263968320, -5.430118837242332575, -26.70804059545048759 ) ) ;
#23111 = CARTESIAN_POINT ( 'NONE',  ( 2.540292811207268020, -2.599765019149025136, 230.7583807310656994 ) ) ;
#23112 = LINE ( 'NONE', #16327, #27325 ) ;
#23113 = B_SPLINE_CURVE_WITH_KNOTS ( 'NONE', 3,
 ( #4480, #28077, #11712, #28230, #4326, #21005 ),
 .UNSPECIFIED., .F., .F.,
 ( 4, 2, 4 ),
 ( 0.000000000000000000, 0.5000000000000000000, 1.000000000000000000 ),
 .UNSPECIFIED. ) ;
#23114 = ORIENTED_EDGE ( 'NONE', *, *, #19312, .T. ) ;
#23115 = CLOSED_SHELL ( 'NONE', ( #29375, #21353, #25500, #18640, #8665, #17419 ) ) ;
#23116 = CARTESIAN_POINT ( 'NONE',  ( 2.070912548172440637, 4.356181786950492629, -33.08863063599999776 ) ) ;
#23117 = EDGE_CURVE ( 'NONE', #9868, #15244, #27235, .T. ) ;
#23118 = VERTEX_POINT ( 'NONE', #24884 ) ;
#23119 = CARTESIAN_POINT ( 'NONE',  ( -4.213298386699523945, 4.800796338101376293, -53.98587006832499924 ) ) ;
#23120 = EDGE_LOOP ( 'NONE', ( #26901, #711, #15701, #12225 ) ) ;
#23121 = APPLICATION_PROTOCOL_DEFINITION ( 'draft international standard', 'automotive_design', 1998, #12183 ) ;
#23122 = VERTEX_POINT ( 'NONE', #27390 ) ;
#23123 = ORIENTED_EDGE ( 'NONE', *, *, #28126, .T. ) ;
#23124 = DIRECTION ( 'NONE',  ( 1.224606353819999829E-16, 1.000000000000000000, 0.000000000000000000 ) ) ;
#23125 = EDGE_CURVE ( 'NONE', #17663, #27730, #28874, .T. ) ;
#23126 = CARTESIAN_POINT ( 'NONE',  ( 0.3615961171405600028, -27.79823316426096014, 6.099998580999981712 ) ) ;
#23127 = CARTESIAN_POINT ( 'NONE',  ( 9.000000000000000000, 19.99999999999999645, -43.39999999999999858 ) ) ;
#23128 = CARTESIAN_POINT ( 'NONE',  ( -27.79999999970000246, -10.21376199200000201, 222.0000000000000000 ) ) ;
#23129 = CARTESIAN_POINT ( 'NONE',  ( 8.000000000284819279, -13.66682223737133128, -36.55330428412179344 ) ) ;
#23130 = LINE ( 'NONE', #16186, #10924 ) ;
#23131 = CARTESIAN_POINT ( 'NONE',  ( -1.102325287918849650, -5.983340188646091740, -3.525234013000005717 ) ) ;
#23132 = FACE_OUTER_BOUND ( 'NONE', #21642, .T. ) ;
#23133 = FACE_OUTER_BOUND ( 'NONE', #25828, .T. ) ;
#23134 = CARTESIAN_POINT ( 'NONE',  ( -2.183849900456024784, 3.899926742306370819, -17.17761783620000315 ) ) ;
#23135 = CARTESIAN_POINT ( 'NONE',  ( -0.4593365651765490831, 6.553622599173768215, -34.29518930510000274 ) ) ;
#23136 = CARTESIAN_POINT ( 'NONE',  ( 8.999999999770000869, 20.61304188753062050, -44.29887312234927066 ) ) ;
#23137 = CARTESIAN_POINT ( 'NONE',  ( 28.45300238704230367, 0.5177135156027735663, 0.5017677510000262409 ) ) ;
#23138 = CARTESIAN_POINT ( 'NONE',  ( -18.62325121933723437, 19.80375466501974913, 0.06723541799999455115 ) ) ;
#23139 = CARTESIAN_POINT ( 'NONE',  ( -14.92487790170366502, -24.58397533831729476, 8.000000000000007105 ) ) ;
#23140 = CARTESIAN_POINT ( 'NONE',  ( 16.40303402077768169, -9.791839085275103827, 0.000000000000000000 ) ) ;
#23141 = CARTESIAN_POINT ( 'NONE',  ( 22.70120178298296310, -14.24511786442693939, 225.4947892891584047 ) ) ;
#23142 = CIRCLE ( 'NONE', #3024, 26.80000000000000071 ) ;
#23143 = CARTESIAN_POINT ( 'NONE',  ( -2.213834474261364260, -2.749352377424092442, 226.6412452697750268 ) ) ;
#23144 = CARTESIAN_POINT ( 'NONE',  ( 8.700000000236814302, -30.00974564182223503, -28.70967732804903605 ) ) ;
#23145 = CARTESIAN_POINT ( 'NONE',  ( -11.78485145404637002, 21.69999999994150031, -70.02209366220616005 ) ) ;
#23146 = VERTEX_POINT ( 'NONE', #5214 ) ;
#23147 = CARTESIAN_POINT ( 'NONE',  ( 0.9163752123955551943, -3.500000000000000000, 227.7139869426476082 ) ) ;
#23148 = PLANE ( 'NONE',  #8702 ) ;
#23149 = EDGE_CURVE ( 'NONE', #17135, #29716, #23659, .T. ) ;
#23150 = CARTESIAN_POINT ( 'NONE',  ( -28.50000000000000000, 1.776356839399999922E-14, 222.0000000000000000 ) ) ;
#23151 = ORIENTED_EDGE ( 'NONE', *, *, #13098, .F. ) ;
#23152 = CARTESIAN_POINT ( 'NONE',  ( 2.295476649252891743, -3.592865671589301257, -43.96966640442499852 ) ) ;
#23153 = VERTEX_POINT ( 'NONE', #24423 ) ;
#23154 = ORIENTED_EDGE ( 'NONE', *, *, #28989, .T. ) ;
#23155 = EDGE_CURVE ( 'NONE', #4371, #19357, #28167, .T. ) ;
#23156 = ORIENTED_EDGE ( 'NONE', *, *, #24440, .F. ) ;
#23157 = CARTESIAN_POINT ( 'NONE',  ( 18.66688684140000376, 20.92780155799999875, 230.2432540810000319 ) ) ;
#23158 = EDGE_CURVE ( 'NONE', #5717, #23153, #20461, .T. ) ;
#23159 = ORIENTED_EDGE ( 'NONE', *, *, #5145, .T. ) ;
#23160 = CARTESIAN_POINT ( 'NONE',  ( 10.69999999997017071, -29.92227941849945694, -29.18484171379398617 ) ) ;
#23161 = CARTESIAN_POINT ( 'NONE',  ( 8.000000000645886900, -15.87764099349055158, -32.96702544412416813 ) ) ;
#23162 = DIRECTION ( 'NONE',  ( -0.9316362575375349842, 0.3633921898465292122, -0.000000000000000000 ) ) ;
#23163 = CARTESIAN_POINT ( 'NONE',  ( -1.249369445655645006, -5.033661498259376366, -93.21726054315608678 ) ) ;
#23164 = CARTESIAN_POINT ( 'NONE',  ( -27.06563796000000366, 3.314475221609999872E-15, 138.0597313979999967 ) ) ;
#23165 = CARTESIAN_POINT ( 'NONE',  ( 3.849220998203362054, -0.3329536615551556000, 227.8479073241742583 ) ) ;
#23166 = CARTESIAN_POINT ( 'NONE',  ( -0.4820778520819999913, -28.49640832880000119, 226.0025182780000250 ) ) ;
#23167 = ORIENTED_EDGE ( 'NONE', *, *, #27627, .T. ) ;
#23168 = CARTESIAN_POINT ( 'NONE',  ( -1.814319851916122772, 5.833166587536846137, -4.774955258300003891 ) ) ;
#23169 = CARTESIAN_POINT ( 'NONE',  ( 0.1332961122732720383, -6.531058726825651028, -23.81888333260000223 ) ) ;
#23170 = CARTESIAN_POINT ( 'NONE',  ( 10.32522729140000095, -24.73114799960000099, -1.399999999999998579 ) ) ;
#23171 = CARTESIAN_POINT ( 'NONE',  ( 24.83827472153076599, -12.48687851163286133, 5.104216618000034345 ) ) ;
#23172 = CARTESIAN_POINT ( 'NONE',  ( -2.914123423697624116, -2.127246859470591112, -88.52261276302716908 ) ) ;
#23173 = CARTESIAN_POINT ( 'NONE',  ( -2.020725942109999895, 3.500000000090000007, 227.9588918784999976 ) ) ;
#23174 = DIRECTION ( 'NONE',  ( 1.000000000000000000, 0.000000000000000000, 0.000000000000000000 ) ) ;
#23175 = CARTESIAN_POINT ( 'NONE',  ( 9.999999999992681410, -130.0000000001073772, -39.98135229079757380 ) ) ;
#23176 = AXIS2_PLACEMENT_3D ( 'NONE', #23421, #1851, #11451 ) ;
#23177 = CARTESIAN_POINT ( 'NONE',  ( 8.000000000278095769, -14.92844969908619035, -33.25053330389217621 ) ) ;
#23178 = DIRECTION ( 'NONE',  ( 0.000000000000000000, -0.3420201433259318913, 0.9396926207858126157 ) ) ;
#23179 = DIRECTION ( 'NONE',  ( 2.764840495839172918E-12, 0.9128796883888953273, -0.4082287037029531107 ) ) ;
#23180 = ORIENTED_EDGE ( 'NONE', *, *, #5387, .T. ) ;
#23181 = CARTESIAN_POINT ( 'NONE',  ( 3.449241269337446791, -4.803451378176493591, -61.04197827312499669 ) ) ;
#23182 = ORIENTED_EDGE ( 'NONE', *, *, #21008, .T. ) ;
#23183 = CARTESIAN_POINT ( 'NONE',  ( 24.41841038956698640, 14.69667349781389376, 3.899998581000013509 ) ) ;
#23184 = CARTESIAN_POINT ( 'NONE',  ( 1.771049722044198971, -6.234229536879996481, -21.29535708919999593 ) ) ;
#23185 = B_SPLINE_CURVE_WITH_KNOTS ( 'NONE', 5,
 ( #12112, #19361, #7393, #26595, #14644, #2673, #12270, #21887, #7693, #19668, #5343, #5180 ),
 .UNSPECIFIED., .F., .F.,
 ( 6, 3, 3, 6 ),
 ( 3.339306057039999942, 4.810258469309999896, 6.613963844750000654, 6.678484288699999993 ),
 .UNSPECIFIED. ) ;
#23186 = ORIENTED_EDGE ( 'NONE', *, *, #27578, .T. ) ;
#23187 = DIRECTION ( 'NONE',  ( 1.000000000000000000, 0.000000000000000000, 0.000000000000000000 ) ) ;
#23188 = CARTESIAN_POINT ( 'NONE',  ( 3.466821295769682159E-14, -2.890242878314739659E-13, 277.5163816122566800 ) ) ;
#23189 = ORIENTED_EDGE ( 'NONE', *, *, #16848, .F. ) ;
#23190 = VERTEX_POINT ( 'NONE', #10875 ) ;
#23191 = ORIENTED_EDGE ( 'NONE', *, *, #9048, .F. ) ;
#23192 = CARTESIAN_POINT ( 'NONE',  ( -25.43121960300668150, -8.635379644106590646, 186.7828584125833515 ) ) ;
#23193 = EDGE_CURVE ( 'NONE', #27018, #24964, #15006, .T. ) ;
#23194 = VERTEX_POINT ( 'NONE', #3464 ) ;
#23195 = CARTESIAN_POINT ( 'NONE',  ( -8.699999999654988159, -17.99042170907872418, -37.01252660134724692 ) ) ;
#23196 = EDGE_CURVE ( 'NONE', #28212, #13351, #8968, .T. ) ;
#23197 = DIRECTION ( 'NONE',  ( 2.257144471330000330E-12, -0.000000000000000000, -1.000000000000000000 ) ) ;
#23198 = CARTESIAN_POINT ( 'NONE',  ( -0.8929276208064895748, -4.785132802852544387, -67.15745670422499813 ) ) ;
#23199 = CARTESIAN_POINT ( 'NONE',  ( 20.58567524440000085, -20.71744736909999673, 229.4485717599999930 ) ) ;
#23200 = VECTOR ( 'NONE', #27073, 999.9999999999998863 ) ;
#23201 = B_SPLINE_CURVE_WITH_KNOTS ( 'NONE', 3,
 ( #25537, #1000, #25217, #20651, #22700, #27888, #8361, #11208, #4127, #3974 ),
 .UNSPECIFIED., .F., .F.,
 ( 4, 2, 2, 2, 4 ),
 ( 0.000000000000000000, 0.2500000000000000000, 0.5000000000000000000, 0.7500000000000000000, 1.000000000000000000 ),
 .UNSPECIFIED. ) ;
#23202 = CARTESIAN_POINT ( 'NONE',  ( -18.34690887264311243, 20.56908522426308394, -0.5592437529999827461 ) ) ;
#23203 = CARTESIAN_POINT ( 'NONE',  ( 10.70777106509999932, -25.82052991099999772, 222.0000000000000000 ) ) ;
#23204 = CARTESIAN_POINT ( 'NONE',  ( -5.114260856059999583, -17.43050419540000107, 230.6999999999999886 ) ) ;
#23205 = ORIENTED_EDGE ( 'NONE', *, *, #5927, .F. ) ;
#23206 = CARTESIAN_POINT ( 'NONE',  ( -10.00000000020000002, -24.91804464959999876, -26.23931466329999651 ) ) ;
#23207 = CARTESIAN_POINT ( 'NONE',  ( 5.864965375735811115, 0.4191680585659274261, -13.64454535870001095 ) ) ;
#23208 = DIRECTION ( 'NONE',  ( 1.000000000000000000, 0.000000000000000000, 0.000000000000000000 ) ) ;
#23209 = CARTESIAN_POINT ( 'NONE',  ( -28.03861306157277866, -0.5101735396242136344, -0.2432540810000105580 ) ) ;
#23210 = ORIENTED_EDGE ( 'NONE', *, *, #5915, .F. ) ;
#23211 = CARTESIAN_POINT ( 'NONE',  ( 19.41514007621238491, 18.50604284286171364, -1.399999999999998579 ) ) ;
#23212 = CARTESIAN_POINT ( 'NONE',  ( -24.45473033751197178, -14.63622298155413226, 6.098654221000004760 ) ) ;
#23213 = CARTESIAN_POINT ( 'NONE',  ( 28.49999999970000175, -7.466149220240000162, 229.0000000000000000 ) ) ;
#23214 = CARTESIAN_POINT ( 'NONE',  ( 21.92393651381221886, 17.69663393540654539, 0.8585786549999974149 ) ) ;
#23215 = CARTESIAN_POINT ( 'NONE',  ( 17.83931934289999788, 20.00000000000000000, 230.6999999999999886 ) ) ;
#23216 = DIRECTION ( 'NONE',  ( -0.000000000000000000, 0.000000000000000000, 1.000000000000000000 ) ) ;
#23217 = CARTESIAN_POINT ( 'NONE',  ( -12.77820031340000106, 20.99999999999999645, -56.10000000020000499 ) ) ;
#23218 = CARTESIAN_POINT ( 'NONE',  ( 13.00000000000000000, 25.22617105830878614, -61.82510970417090590 ) ) ;
#23219 = ORIENTED_EDGE ( 'NONE', *, *, #7848, .T. ) ;
#23220 = CARTESIAN_POINT ( 'NONE',  ( 24.93720649360215802, -13.79881813812812297, 3.899998581000013509 ) ) ;
#23221 = CARTESIAN_POINT ( 'NONE',  ( 25.26809617030000155, 12.77001320659999983, 229.0000000000000000 ) ) ;
#23222 = EDGE_CURVE ( 'NONE', #17862, #24922, #11325, .T. ) ;
#23223 = CIRCLE ( 'NONE', #12154, 4.997501249380000843 ) ;
#23224 = CARTESIAN_POINT ( 'NONE',  ( 1.217040025866600539, -3.881590577319316893, -68.10000000002500542 ) ) ;
#23225 = CARTESIAN_POINT ( 'NONE',  ( 3.529820002191843997, -0.01646793578303169109, -0.6999999999999783062 ) ) ;
#23226 = CARTESIAN_POINT ( 'NONE',  ( -4.127468247539838764, -0.07107026465252587466, -44.10000000002499831 ) ) ;
#23227 = FILL_AREA_STYLE ('',( #16133 ) ) ;
#23228 = ORIENTED_EDGE ( 'NONE', *, *, #11988, .F. ) ;
#23229 = CARTESIAN_POINT ( 'NONE',  ( 3.686970300939999667, -0.1862064327014488485, -68.94610314789109395 ) ) ;
#23230 = CARTESIAN_POINT ( 'NONE',  ( 5.384875807261761516, 2.601783486389667832, -67.33315453642501325 ) ) ;
#23231 = ORIENTED_EDGE ( 'NONE', *, *, #16565, .T. ) ;
#23232 = CARTESIAN_POINT ( 'NONE',  ( 17.83931934289999788, 20.00000000000000000, 230.6999999999999886 ) ) ;
#23233 = VERTEX_POINT ( 'NONE', #11339 ) ;
#23234 = CARTESIAN_POINT ( 'NONE',  ( -25.14597776469546631, -15.02549348218341230, 0.8585788009999872905 ) ) ;
#23235 = AXIS2_PLACEMENT_3D ( 'NONE', #22147, #8113, #13003 ) ;
#23236 = VERTEX_POINT ( 'NONE', #18087 ) ;
#23237 = CARTESIAN_POINT ( 'NONE',  ( -11.14649459219999983, -24.37257237719999736, -0.7852065530999998710 ) ) ;
#23238 = VECTOR ( 'NONE', #17154, 1000.000000000000000 ) ;
#23239 = PRESENTATION_STYLE_ASSIGNMENT (( #13948 ) ) ;
#23240 = CARTESIAN_POINT ( 'NONE',  ( -8.699999999669005391, -18.23122067931867107, -34.51216076567753532 ) ) ;
#23241 = CARTESIAN_POINT ( 'NONE',  ( -3.455601306038264209, -0.7156333712644181722, 0.000000000000000000 ) ) ;
#23242 = FACE_BOUND ( 'NONE', #4105, .T. ) ;
#23243 = CARTESIAN_POINT ( 'NONE',  ( 1.065814103639999922E-14, -1.065814103639999922E-14, 143.6055512749999821 ) ) ;
#23244 = CARTESIAN_POINT ( 'NONE',  ( 8.700000000245456278, -28.58416947897984173, -30.97788247129344086 ) ) ;
#23245 = EDGE_LOOP ( 'NONE', ( #11092, #27323, #21079, #27359 ) ) ;
#23246 = FACE_BOUND ( 'NONE', #31043, .T. ) ;
#23247 = LINE ( 'NONE', #22624, #8750 ) ;
#23248 = CARTESIAN_POINT ( 'NONE',  ( -3.868754989949999779, 11.66966430080000094, 232.6627643349999914 ) ) ;
#23249 = EDGE_CURVE ( 'NONE', #20613, #8033, #27855, .T. ) ;
#23250 = CARTESIAN_POINT ( 'NONE',  ( -2.909761405888054320, -1.959661555870369831, 230.8336353467288973 ) ) ;
#23251 = CARTESIAN_POINT ( 'NONE',  ( 23.45268582460785112, -12.96920632855593425, 4.006804827044976314 ) ) ;
#23252 = CARTESIAN_POINT ( 'NONE',  ( -1.100001419170000050, -27.77850706310000106, 225.1040592169999854 ) ) ;
#23253 = AXIS2_PLACEMENT_3D ( 'NONE', #19035, #28944, #6919 ) ;
#23254 = CARTESIAN_POINT ( 'NONE',  ( -4.498618707852113374, 2.988074248075567318, -0.6999999999999992895 ) ) ;
#23255 = CARTESIAN_POINT ( 'NONE',  ( -15.73624015665173914, -8.835417945575107623, -0.6999999999999783062 ) ) ;
#23256 = CARTESIAN_POINT ( 'NONE',  ( -3.108138112192400104, -3.359256988581868608, -49.79612412472500438 ) ) ;
#23257 = ADVANCED_FACE ( 'NONE', ( #15735 ), #20935, .F. ) ;
#23258 = CARTESIAN_POINT ( 'NONE',  ( 27.52676963214367944, 0.5008603480904615379, 0.2686740700000300741 ) ) ;
#23259 = CARTESIAN_POINT ( 'NONE',  ( -17.59696597926837214, -9.791839085300418688, -0.6999999999999784173 ) ) ;
#23260 = CARTESIAN_POINT ( 'NONE',  ( 3.401136804196998931, -1.108686906912193182, 230.7917081009935032 ) ) ;
#23261 = AXIS2_PLACEMENT_3D ( 'NONE', #20492, #1142, #20335 ) ;
#23262 = PLANE ( 'NONE',  #7228 ) ;
#23263 = VERTEX_POINT ( 'NONE', #25666 ) ;
#23264 = CARTESIAN_POINT ( 'NONE',  ( 10.69999999997381757, -25.15707083535441768, -30.79962415710182810 ) ) ;
#23265 = ORIENTED_EDGE ( 'NONE', *, *, #25427, .F. ) ;
#23266 = ADVANCED_FACE ( 'NONE', ( #4096 ), #13065, .F. ) ;
#23267 = CARTESIAN_POINT ( 'NONE',  ( -4.541600168151706640, -0.1148504950298593758, -53.95673954922499860 ) ) ;
#23268 = ORIENTED_EDGE ( 'NONE', *, *, #28811, .T. ) ;
#23269 = PRODUCT_CONTEXT ( 'NONE', #3128, 'mechanical' ) ;
#23270 = ORIENTED_EDGE ( 'NONE', *, *, #8933, .F. ) ;
#23271 = CARTESIAN_POINT ( 'NONE',  ( -17.48108435972729424, -29.89324280579608839, -32.50314025840578580 ) ) ;
#23272 = EDGE_LOOP ( 'NONE', ( #20455, #25181, #20304 ) ) ;
#23273 = CARTESIAN_POINT ( 'NONE',  ( 14.69473318574057430, -28.06568682441304574, -23.24217067950538862 ) ) ;
#23274 = CARTESIAN_POINT ( 'NONE',  ( 4.638687372224857164, -10.76914457791739999, -35.56451223092034297 ) ) ;
#23275 = CARTESIAN_POINT ( 'NONE',  ( 380005.9281980000087, 207598.1847299999790, 250226.6334002700169 ) ) ;
#23276 = CARTESIAN_POINT ( 'NONE',  ( -8.699999998949005331, -18.23122067931867107, -34.51216076567753532 ) ) ;
#23277 = CARTESIAN_POINT ( 'NONE',  ( 0.000000000000000000, 0.000000000000000000, 188.3395398250000028 ) ) ;
#23278 = DIRECTION ( 'NONE',  ( 0.000000000000000000, 0.000000000000000000, 1.000000000000000000 ) ) ;
#23279 = CARTESIAN_POINT ( 'NONE',  ( -3.885731905334995684, 2.027028853511404272, -0.9187643563000024161 ) ) ;
#23280 = AXIS2_PLACEMENT_3D ( 'NONE', #1073, #8131, #20115 ) ;
#23281 = CARTESIAN_POINT ( 'NONE',  ( -26.80000000000000071, 3.552713678799999608E-15, 230.6999999999999886 ) ) ;
#23282 = ORIENTED_EDGE ( 'NONE', *, *, #437, .F. ) ;
#23283 = DIRECTION ( 'NONE',  ( -0.000000000000000000, -0.000000000000000000, -1.000000000000000000 ) ) ;
#23284 = CARTESIAN_POINT ( 'NONE',  ( -5.853056545089267537, 1.703994407032248581, -16.90443125760000243 ) ) ;
#23285 = CARTESIAN_POINT ( 'NONE',  ( -4.976668802704899086, 3.592974922927941073, -33.86696136360001219 ) ) ;
#23286 = EDGE_CURVE ( 'NONE', #7351, #22999, #30777, .T. ) ;
#23287 = CARTESIAN_POINT ( 'NONE',  ( 24.36724931191462318, 13.38201648793565468, 4.854188467883240321 ) ) ;
#23288 = CARTESIAN_POINT ( 'NONE',  ( 1.127732790480000080, -28.47784299079999926, 224.8959500220000223 ) ) ;
#23289 = CARTESIAN_POINT ( 'NONE',  ( -26.99557660706030049, -9.615007461563203961, 8.000000000000007105 ) ) ;
#23290 = CARTESIAN_POINT ( 'NONE',  ( -2.596859818084732208, 2.501786840328394046, 227.7073827799883361 ) ) ;
#23291 = EDGE_CURVE ( 'NONE', #10428, #18996, #8332, .T. ) ;
#23292 = CARTESIAN_POINT ( 'NONE',  ( 27.47529052171122288, 5.047756207413780949, -0.5592437529999827461 ) ) ;
#23293 = CARTESIAN_POINT ( 'NONE',  ( 8.700000000290035729, -14.46884615155692977, -37.57385308047970796 ) ) ;
#23294 = CARTESIAN_POINT ( 'NONE',  ( 8.700000000235821318, -29.73863906516063693, -27.17531388883607590 ) ) ;
#23295 = AXIS2_PLACEMENT_3D ( 'NONE', #26270, #317, #24071 ) ;
#23296 = CARTESIAN_POINT ( 'NONE',  ( -6.000000000000000000, -17.40201702037870746, -76.27632353305202173 ) ) ;
#23297 = ORIENTED_EDGE ( 'NONE', *, *, #1625, .F. ) ;
#23298 = PRESENTATION_LAYER_ASSIGNMENT (  '', '', ( #19275 ) ) ;
#23299 = DIRECTION ( 'NONE',  ( 0.8660254037843289066, -0.5000000000001899592, 0.000000000000000000 ) ) ;
#23300 = CARTESIAN_POINT ( 'NONE',  ( 3.888118302228526169, 1.436696886034274812, -38.17989306233251057 ) ) ;
#23301 = CARTESIAN_POINT ( 'NONE',  ( 1.270994686748740277, -4.981061367834454856, -0.7000029814077138868 ) ) ;
#23302 = ORIENTED_EDGE ( 'NONE', *, *, #26362, .F. ) ;
#23303 = EDGE_CURVE ( 'NONE', #24422, #30907, #16116, .T. ) ;
#23304 = CARTESIAN_POINT ( 'NONE',  ( 0.7190444496271986008, -5.886645524271489904, -43.78057807742499818 ) ) ;
#23305 = EDGE_LOOP ( 'NONE', ( #18809, #15727, #12262, #481 ) ) ;
#23306 = ORIENTED_EDGE ( 'NONE', *, *, #28250, .T. ) ;
#23307 = ORIENTED_EDGE ( 'NONE', *, *, #5479, .T. ) ;
#23308 = CARTESIAN_POINT ( 'NONE',  ( 22.43614352489999675, 17.98932536259999893, 229.7625741969999922 ) ) ;
#23309 = ADVANCED_FACE ( 'NONE', ( #2053 ), #18718, .F. ) ;
#23310 = ORIENTED_EDGE ( 'NONE', *, *, #2639, .T. ) ;
#23311 = CARTESIAN_POINT ( 'NONE',  ( -24.11017618899999704, -13.84060607850000046, 226.0986578700000109 ) ) ;
#23312 = PRODUCT_RELATED_PRODUCT_CATEGORY ( 'part', '', ( #3119 ) ) ;
#23313 = CARTESIAN_POINT ( 'NONE',  ( 24.40022624086872938, 14.72688605419589614, 3.899998581000013509 ) ) ;
#23314 = CARTESIAN_POINT ( 'NONE',  ( -23.82471740849593544, -15.64077206322649083, 4.791628272000025390 ) ) ;
#23315 = DIRECTION ( 'NONE',  ( 0.3633921898465291567, 0.9316362575375349842, -6.938893903907229167E-15 ) ) ;
#23316 = CARTESIAN_POINT ( 'NONE',  ( 17.16657240420000008, 10.97998838177520931, 0.05106179917585291356 ) ) ;
#23317 = CARTESIAN_POINT ( 'NONE',  ( 23.03549535077002375, -13.87410949944762351, -1.399999999999998357 ) ) ;
#23318 = CARTESIAN_POINT ( 'NONE',  ( 23.20948082139999968, -13.40000000000000036, 6.099999999630000502 ) ) ;
#23319 = AXIS2_PLACEMENT_3D ( 'NONE', #9073, #1540, #23417 ) ;
#23320 = DIRECTION ( 'NONE',  ( 1.000000000000000000, -2.197671641579999817E-16, 0.000000000000000000 ) ) ;
#23321 = CIRCLE ( 'NONE', #1708, 3.199999983039998774 ) ;
#23322 = ORIENTED_EDGE ( 'NONE', *, *, #23196, .F. ) ;
#23323 = AXIS2_PLACEMENT_3D ( 'NONE', #19271, #399, #14243 ) ;
#23324 = CARTESIAN_POINT ( 'NONE',  ( -3.866727543631055308, 3.949224786475222349, -5.568732180600000525 ) ) ;
#23325 = CARTESIAN_POINT ( 'NONE',  ( -5.611385130160316592, 1.726552310816597435, -21.32289663400000634 ) ) ;
#23326 = AXIS2_PLACEMENT_3D ( 'NONE', #17893, #8141, #783 ) ;
#23327 = DIRECTION ( 'NONE',  ( 1.000000000000000000, -1.224606353820000075E-16, 0.000000000000000000 ) ) ;
#23328 = STYLED_ITEM ( 'NONE', ( #8783 ), #438 ) ;
#23329 = EDGE_CURVE ( 'NONE', #30101, #8184, #3337, .T. ) ;
#23330 = CARTESIAN_POINT ( 'NONE',  ( -23.35113490818136839, -13.15228900125540434, 223.9278743037135655 ) ) ;
#23331 = CARTESIAN_POINT ( 'NONE',  ( 0.6231431573705923377, 3.499789347373832626, 227.6774647154332456 ) ) ;
#23332 = CARTESIAN_POINT ( 'NONE',  ( -12.30000000006999805, -27.00000000000000000, -28.40000000020000215 ) ) ;
#23333 = CARTESIAN_POINT ( 'NONE',  ( -24.48873108229999929, -14.58042505439999914, 226.0425106499999970 ) ) ;
#23334 = EDGE_CURVE ( 'NONE', #17637, #13449, #20630, .T. ) ;
#23335 = CARTESIAN_POINT ( 'NONE',  ( -2.595987296770100095, -16.63200279373747392, -109.8342699011499946 ) ) ;
#23336 = CARTESIAN_POINT ( 'NONE',  ( 14.76964124820000102, 19.99999999999999645, -0.6999999999999992895 ) ) ;
#23337 = LINE ( 'NONE', #6639, #5757 ) ;
#23338 = EDGE_LOOP ( 'NONE', ( #2116, #23559, #6072, #5567, #249, #27280, #18382, #6486 ) ) ;
#23339 = CARTESIAN_POINT ( 'NONE',  ( -5.110483438867316153, -2.062468175234513534, -58.58491726642499486 ) ) ;
#23340 = CARTESIAN_POINT ( 'NONE',  ( -24.93720648713954446, 13.79881813474513486, 6.099998581000020792 ) ) ;
#23341 = VERTEX_POINT ( 'NONE', #30844 ) ;
#23342 = EDGE_CURVE ( 'NONE', #15436, #29055, #21030, .T. ) ;
#23343 = ORIENTED_EDGE ( 'NONE', *, *, #19252, .T. ) ;
#23344 = CARTESIAN_POINT ( 'NONE',  ( -5.712231154917421249E-11, -114.8328013978253495, 22.59891173985517199 ) ) ;
#23345 = CARTESIAN_POINT ( 'NONE',  ( 4.725722714896615884, -3.873618144318392797, -23.99674734060000603 ) ) ;
#23346 = ORIENTED_EDGE ( 'NONE', *, *, #21977, .F. ) ;
#23347 = CARTESIAN_POINT ( 'NONE',  ( -25.22658730140000216, -13.26242337740000110, 225.1042194559999814 ) ) ;
#23348 = DIRECTION ( 'NONE',  ( -0.9316362575375356503, -0.3633921898465275468, 0.000000000000000000 ) ) ;
#23349 = AXIS2_PLACEMENT_3D ( 'NONE', #23023, #11060, #3340 ) ;
#23350 = EDGE_LOOP ( 'NONE', ( #19395, #4317 ) ) ;
#23351 = VECTOR ( 'NONE', #24979, 1000.000000000000000 ) ;
#23352 = ORIENTED_EDGE ( 'NONE', *, *, #9048, .T. ) ;
#23353 = ORIENTED_EDGE ( 'NONE', *, *, #2867, .F. ) ;
#23354 = CIRCLE ( 'NONE', #6758, 3.000000000000001332 ) ;
#23355 = DIRECTION ( 'NONE',  ( -0.9595496299847263710, 0.2815395311429191305, 0.000000000000000000 ) ) ;
#23356 =( LENGTH_UNIT ( ) NAMED_UNIT ( * ) SI_UNIT ( .MILLI., .METRE. ) );
#23357 = VECTOR ( 'NONE', #22591, 1000.000000000000000 ) ;
#23358 = VERTEX_POINT ( 'NONE', #14328 ) ;
#23359 = LINE ( 'NONE', #1638, #15476 ) ;
#23360 = CARTESIAN_POINT ( 'NONE',  ( 23.81569860410000317, -13.75000000000000000, 3.900000000369999942 ) ) ;
#23361 = CARTESIAN_POINT ( 'NONE',  ( -0.9992285280876744835, -5.354791469827751449, -67.10745670422500098 ) ) ;
#23362 = CARTESIAN_POINT ( 'NONE',  ( 5.041582825300000792, -29.73257086209999756, 230.0000000000000000 ) ) ;
#23363 = B_SPLINE_CURVE_WITH_KNOTS ( 'NONE', 3,
 ( #23173, #6634, #15924, #18905, #6794, #25534, #23490, #16081, #11203, #8832, #20805, #16391, #11364, #4124, #28503, #13720, #23331, #31024, #1774, #20961, #30567, #8994, #6948, #25997, #16232, #25848 ),
 .UNSPECIFIED., .F., .F.,
 ( 4, 2, 2, 1, 1, 2, 2, 2, 2, 2, 1, 1, 2, 2, 4 ),
 ( 0.000000000000000000, 0.1249999999999871769, 0.1874999999999786282, 0.2187499999999742983, 0.2343749999999737987, 0.2421874999999750755, 0.2499999999999762967, 0.4999999999999507061, 0.6249999999999379385, 0.6874999999999308331, 0.7187499999999272804, 0.7343749999999240607, 0.7421874999999240607, 0.7499999999999240607, 1.000000000000000000 ),
 .UNSPECIFIED. ) ;
#23364 = CARTESIAN_POINT ( 'NONE',  ( -0.5612683859346103699, -26.79446734600721314, 224.0425474258357212 ) ) ;
#23365 = CARTESIAN_POINT ( 'NONE',  ( -3.339220672710000226, -27.75291293060000086, 222.0000000000000000 ) ) ;
#23366 =( GEOMETRIC_REPRESENTATION_CONTEXT ( 3 ) GLOBAL_UNCERTAINTY_ASSIGNED_CONTEXT ( ( #16918 ) ) GLOBAL_UNIT_ASSIGNED_CONTEXT ( ( #29643, #1159, #1013 ) ) REPRESENTATION_CONTEXT ( 'NONE', 'WORKASPACE' ) );
#23367 = FACE_OUTER_BOUND ( 'NONE', #23513, .T. ) ;
#23368 = CARTESIAN_POINT ( 'NONE',  ( -24.39135169139981940, 14.74223402956394402, 4.689353541000001790 ) ) ;
#23369 = ORIENTED_EDGE ( 'NONE', *, *, #25559, .F. ) ;
#23370 = CARTESIAN_POINT ( 'NONE',  ( -19.43556844913216608, 20.00000873967102777, -0.3062681690857439465 ) ) ;
#23371 = CARTESIAN_POINT ( 'NONE',  ( 3.550610403408205329, -5.007233058897099021, -11.52388893670000591 ) ) ;
#23372 = DIRECTION ( 'NONE',  ( 1.000000000000000000, 0.000000000000000000, 0.000000000000000000 ) ) ;
#23373 = ADVANCED_FACE ( 'NONE', ( #18880 ), #16516, .F. ) ;
#23374 = CIRCLE ( 'NONE', #9794, 27.50000000000000000 ) ;
#23375 = CARTESIAN_POINT ( 'NONE',  ( 4.977446931567997446, 11.28020582389469517, 232.6627635322004153 ) ) ;
#23376 = VERTEX_POINT ( 'NONE', #25821 ) ;
#23377 = CARTESIAN_POINT ( 'NONE',  ( 9.993285220779439371, -25.61999708228226069, 36.39444872359999295 ) ) ;
#23378 = DIRECTION ( 'NONE',  ( 0.000000000000000000, 0.000000000000000000, -1.000000000000000000 ) ) ;
#23379 = VECTOR ( 'NONE', #10443, 1000.000000000000000 ) ;
#23380 = CARTESIAN_POINT ( 'NONE',  ( -8.999999999796672867, 20.52198665876978012, -44.20777309639302644 ) ) ;
#23381 = CARTESIAN_POINT ( 'NONE',  ( 1.929629880830433075, -20.49902116409572983, -27.48112851569159787 ) ) ;
#23382 = EDGE_CURVE ( 'NONE', #10428, #1677, #13897, .T. ) ;
#23383 = CARTESIAN_POINT ( 'NONE',  ( 10.69999999999999929, -130.0000000000000000, -42.39999999999999858 ) ) ;
#23384 = EDGE_CURVE ( 'NONE', #11027, #24538, #12380, .T. ) ;
#23385 = CARTESIAN_POINT ( 'NONE',  ( -4.535753307212162078, -3.367775055652930227, -56.27895058492499913 ) ) ;
#23386 = CARTESIAN_POINT ( 'NONE',  ( 0.000000000000000000, 0.000000000000000000, 229.6412452697800006 ) ) ;
#23388 = EDGE_CURVE ( 'NONE', #21601, #27055, #13162, .T. ) ;
#23387 = CARTESIAN_POINT ( 'NONE',  ( 0.000000000000000000, 0.000000000000000000, 229.6412452697800006 ) ) ;
#23389 = ORIENTED_EDGE ( 'NONE', *, *, #28054, .F. ) ;
#23390 = CARTESIAN_POINT ( 'NONE',  ( 22.83442928019999840, 16.43389279790000046, 222.0000000000000000 ) ) ;
#23391 = CARTESIAN_POINT ( 'NONE',  ( 1.954603020853704187, -3.688534106663021284, -68.10000000002501963 ) ) ;
#23392 = TOROIDAL_SURFACE ( 'NONE', #7291, 24.50000000000000000, 3.200000000000000178 ) ;
#23393 =( GEOMETRIC_REPRESENTATION_CONTEXT ( 3 ) GLOBAL_UNCERTAINTY_ASSIGNED_CONTEXT ( ( #21965 ) ) GLOBAL_UNIT_ASSIGNED_CONTEXT ( ( #17632, #17487, #29913 ) ) REPRESENTATION_CONTEXT ( 'NONE', 'WORKASPACE' ) );
#23394 = CARTESIAN_POINT ( 'NONE',  ( -1.366018022287268430, -3.254826447534360234, -0.6999999999999783062 ) ) ;
#23395 = CARTESIAN_POINT ( 'NONE',  ( -23.88745424812704954, 14.22183756790175302, 5.677565560279540513 ) ) ;
#23396 = PRESENTATION_STYLE_ASSIGNMENT (( #9051 ) ) ;
#23397 = ORIENTED_EDGE ( 'NONE', *, *, #7072, .F. ) ;
#23398 = CARTESIAN_POINT ( 'NONE',  ( -10.00000000045316284, -24.07808196999543782, -27.61475634692235559 ) ) ;
#23399 = CARTESIAN_POINT ( 'NONE',  ( 4.883349601227579662, 0.1168011502185895972, -64.46686508972499041 ) ) ;
#23400 = VECTOR ( 'NONE', #27691, 1000.000000000000114 ) ;
#23401 = ORIENTED_EDGE ( 'NONE', *, *, #24774, .F. ) ;
#23402 = FACE_OUTER_BOUND ( 'NONE', #19626, .T. ) ;
#23403 = CARTESIAN_POINT ( 'NONE',  ( -25.07108469382532334, -14.98074245159186191, 0.5514273980000150566 ) ) ;
#23404 = ORIENTED_EDGE ( 'NONE', *, *, #14798, .F. ) ;
#23405 = CARTESIAN_POINT ( 'NONE',  ( -12.29999999970000069, -27.00000000000000000, -28.40000000001083436 ) ) ;
#23406 = EDGE_CURVE ( 'NONE', #8650, #22953, #3701, .T. ) ;
#23407 = DIRECTION ( 'NONE',  ( 0.000000000000000000, 4.000204360710000258E-16, 1.000000000000000000 ) ) ;
#23408 = CARTESIAN_POINT ( 'NONE',  ( -3.388885134110333208, -1.130278766700842263, 230.7950857227854158 ) ) ;
#23409 = FACE_OUTER_BOUND ( 'NONE', #22028, .T. ) ;
#23410 = CARTESIAN_POINT ( 'NONE',  ( -12.35698168758715099, -22.00000000000000000, -29.34490690764078380 ) ) ;
#23411 = STYLED_ITEM ( 'NONE', ( #24085 ), #20440 ) ;
#23412 = DIRECTION ( 'NONE',  ( -1.347073341475313442E-12, 0.9800962620158550909, 0.1985228379369698981 ) ) ;
#23413 = ORIENTED_EDGE ( 'NONE', *, *, #7926, .F. ) ;
#23414 = DIRECTION ( 'NONE',  ( -0.9998345049574558496, -0.01819238017630799703, 0.000000000000000000 ) ) ;
#23415 = CARTESIAN_POINT ( 'NONE',  ( 0.8784916434280891639, -26.78562594471228664, 225.6660761023112229 ) ) ;
#23416 = CARTESIAN_POINT ( 'NONE',  ( 20.30406631259999983, 20.00000862929999812, 229.0000000000000000 ) ) ;
#23417 = DIRECTION ( 'NONE',  ( 1.000000000000000000, 0.000000000000000000, 0.000000000000000000 ) ) ;
#23418 = PLANE ( 'NONE',  #2105 ) ;
#23419 = CARTESIAN_POINT ( 'NONE',  ( -10.14902473071360411, -26.01926976408356396, 92.06031501460000754 ) ) ;
#23420 = CARTESIAN_POINT ( 'NONE',  ( 8.700000000247927190, -27.47597782793287990, -31.38791861936106287 ) ) ;
#23421 = CARTESIAN_POINT ( 'NONE',  ( 10.70000000009999930, -27.00000000000000000, -28.39999999989999679 ) ) ;
#23422 = CARTESIAN_POINT ( 'NONE',  ( -3.745704904464692842, -4.048335345151853559, -49.39612412472500580 ) ) ;
#23423 = B_SPLINE_CURVE_WITH_KNOTS ( 'NONE', 3,
 ( #16071, #28181, #13392, #25836, #11045, #10887 ),
 .UNSPECIFIED., .F., .F.,
 ( 4, 2, 4 ),
 ( 0.000000000000000000, 0.5000000000000000000, 1.000000000000000000 ),
 .UNSPECIFIED. ) ;
#23424 = B_SPLINE_CURVE_WITH_KNOTS ( 'NONE', 3,
 ( #15914, #25523, #30081, #18106, #30557, #6471 ),
 .UNSPECIFIED., .F., .F.,
 ( 4, 2, 4 ),
 ( 0.000000000000000000, 0.5000000000000000000, 1.000000000000000000 ),
 .UNSPECIFIED. ) ;
#23425 = B_SPLINE_CURVE_WITH_KNOTS ( 'NONE', 3,
 ( #16594, #21950, #4811, #9988, #28408, #4492 ),
 .UNSPECIFIED., .F., .F.,
 ( 4, 2, 4 ),
 ( 0.000000000000000000, 0.5000000000000000000, 1.000000000000000000 ),
 .UNSPECIFIED. ) ;
#23426 = CARTESIAN_POINT ( 'NONE',  ( 20.30405755279999980, 20.00000000000000000, 226.9999998930000231 ) ) ;
#23427 = CARTESIAN_POINT ( 'NONE',  ( -7.196110752422828938, -6.955782886976791701, -34.08660717815514829 ) ) ;
#23428 = PLANE ( 'NONE',  #18813 ) ;
#23429 = CARTESIAN_POINT ( 'NONE',  ( -24.34663841809999951, -12.78636765230000094, 225.0000000000000000 ) ) ;
#23430 = VERTEX_POINT ( 'NONE', #4049 ) ;
#23431 = CARTESIAN_POINT ( 'NONE',  ( 5.672553144689285176, -0.9485505809898806540, -36.34517599849999669 ) ) ;
#23432 = VERTEX_POINT ( 'NONE', #18517 ) ;
#23433 = ADVANCED_FACE ( 'NONE', ( #16005 ), #8759, .F. ) ;
#23434 = CARTESIAN_POINT ( 'NONE',  ( 5.053719932297398465, 0.5711438792955092492, -55.76771407622499055 ) ) ;
#23435 = ORIENTED_EDGE ( 'NONE', *, *, #27360, .T. ) ;
#23436 = ITEM_DEFINED_TRANSFORMATION ( 'NONE', 'NONE', #15350,  #17722 ) ;
#23437 = ORIENTED_EDGE ( 'NONE', *, *, #18840, .T. ) ;
#23438 = DIRECTION ( 'NONE',  ( 0.000000000000000000, 0.000000000000000000, 1.000000000000000000 ) ) ;
#23439 = ORIENTED_EDGE ( 'NONE', *, *, #14479, .F. ) ;
#23440 = FILL_AREA_STYLE_COLOUR ( '', #5720 ) ;
#23441 = EDGE_CURVE ( 'NONE', #24111, #24088, #1704, .T. ) ;
#23442 = CARTESIAN_POINT ( 'NONE',  ( 6.171604636184551573, -8.664889659197820393, -36.59082592942991141 ) ) ;
#23443 = CARTESIAN_POINT ( 'NONE',  ( -17.20468998641199576, -31.52458743410349484, -25.23876908135297015 ) ) ;
#23444 = CARTESIAN_POINT ( 'NONE',  ( -6.372675331765073281, 4.806357324490649674, -43.16119209199440121 ) ) ;
#23445 = CARTESIAN_POINT ( 'NONE',  ( -20.26572724632349320, -21.15151735177849091, 8.000000000000007105 ) ) ;
#23446 = CARTESIAN_POINT ( 'NONE',  ( 27.54391552379999908, -3.373045395939999845E-15, 92.95625301640001226 ) ) ;
#23447 = CARTESIAN_POINT ( 'NONE',  ( -3.052679639724400928, 3.117809041995142749, -4.568732180599999637 ) ) ;
#23448 = CARTESIAN_POINT ( 'NONE',  ( -27.04041630560000087, -3.552713678799999608E-15, 230.6999999999999886 ) ) ;
#23449 = ORIENTED_EDGE ( 'NONE', *, *, #28153, .T. ) ;
#23450 = CARTESIAN_POINT ( 'NONE',  ( 24.93720649360215802, -13.79881813812812297, 6.099998581000020792 ) ) ;
#23451 = CARTESIAN_POINT ( 'NONE',  ( -2.579713781069702616, -4.412685520613435664, -16.61932079290000530 ) ) ;
#23452 = CARTESIAN_POINT ( 'NONE',  ( 4.373195337096333013, -2.904765488536246387, -35.35875473020000470 ) ) ;
#23453 = CARTESIAN_POINT ( 'NONE',  ( -0.8466629511608627645, -26.78674366427728160, 5.703642739696129560 ) ) ;
#23454 = CARTESIAN_POINT ( 'NONE',  ( 0.8738980057240000043, -27.78653623639999992, 224.3198498209999912 ) ) ;
#23455 = CARTESIAN_POINT ( 'NONE',  ( -8.000000000030556890, -116.5561065465021784, 18.74526241810166027 ) ) ;
#23456 = CARTESIAN_POINT ( 'NONE',  ( -2.572138351271164414, 2.544598447946130992, 227.7144805344102849 ) ) ;
#23457 = CARTESIAN_POINT ( 'NONE',  ( 28.36759364733395472, 5.211690002337984851, 0.5017677510000262409 ) ) ;
#23458 = CARTESIAN_POINT ( 'NONE',  ( -10.00000000000000000, 21.70000000000000284, -64.10000000000000853 ) ) ;
#23459 = CARTESIAN_POINT ( 'NONE',  ( 0.4024591535043843260, -27.79733476267318437, 3.904047916000019658 ) ) ;
#23460 = EDGE_CURVE ( 'NONE', #28246, #2338, #11994, .T. ) ;
#23461 = LINE ( 'NONE', #11337, #21295 ) ;
#23462 = ORIENTED_EDGE ( 'NONE', *, *, #13667, .T. ) ;
#23463 = CARTESIAN_POINT ( 'NONE',  ( -17.77342497899898888, -8.417133906617015882, 0.000000000000000000 ) ) ;
#23464 =( NAMED_UNIT ( * ) SI_UNIT ( $, .STERADIAN. ) SOLID_ANGLE_UNIT ( ) );
#23465 = CARTESIAN_POINT ( 'NONE',  ( -2.023360855367876354, -4.853169170121535814, -0.7001634333184084680 ) ) ;
#23466 = ORIENTED_EDGE ( 'NONE', *, *, #2303, .F. ) ;
#23467 = CARTESIAN_POINT ( 'NONE',  ( -4.945984810541346199, -1.782911138613007207, -45.16497819512499490 ) ) ;
#23468 = ORIENTED_EDGE ( 'NONE', *, *, #23759, .T. ) ;
#23469 = VERTEX_POINT ( 'NONE', #15854 ) ;
#23470 = EDGE_LOOP ( 'NONE', ( #1363, #26384, #14864, #25672 ) ) ;
#23471 = CARTESIAN_POINT ( 'NONE',  ( 21.80586599240000112, 17.48396816709999868, 230.5592437530000041 ) ) ;
#23472 = B_SPLINE_CURVE_WITH_KNOTS ( 'NONE', 3,
 ( #28052, #18610, #23507, #6181, #30104, #28207, #8371, #3660, #15939, #13581 ),
 .UNSPECIFIED., .F., .F.,
 ( 4, 2, 2, 2, 4 ),
 ( 0.000000000000000000, 0.2499999999999998890, 0.4999999999999997780, 0.7499999999999998890, 1.000000000000000000 ),
 .UNSPECIFIED. ) ;
#23473 = ORIENTED_EDGE ( 'NONE', *, *, #15465, .F. ) ;
#23474 = CARTESIAN_POINT ( 'NONE',  ( 10.69999999997181561, -29.62111648953255738, -29.91136270442498102 ) ) ;
#23475 = CARTESIAN_POINT ( 'NONE',  ( 24.21906834310036771, 15.02342240524378703, 3.957526369000014199 ) ) ;
#23476 = EDGE_CURVE ( 'NONE', #13298, #11678, #11813, .T. ) ;
#23477 = LINE ( 'NONE', #30858, #22520 ) ;
#23478 = CARTESIAN_POINT ( 'NONE',  ( -10.00000000070000183, -27.00000000000000000, -25.39999999999999858 ) ) ;
#23479 = CARTESIAN_POINT ( 'NONE',  ( 0.5184513693225318853, -28.49550581263314086, 3.899998581000013509 ) ) ;
#23480 = DIRECTION ( 'NONE',  ( -1.000000000000000000, 0.000000000000000000, 0.000000000000000000 ) ) ;
#23481 = CARTESIAN_POINT ( 'NONE',  ( 3.108392760683923228, -1.616105808619877626, 227.6466545571246343 ) ) ;
#23482 = FACE_OUTER_BOUND ( 'NONE', #6838, .T. ) ;
#23483 = ORIENTED_EDGE ( 'NONE', *, *, #23149, .T. ) ;
#23484 = CARTESIAN_POINT ( 'NONE',  ( -4.273751495587445604, 4.364932658710685587, -4.568732180600005854 ) ) ;
#23485 = CARTESIAN_POINT ( 'NONE',  ( 0.3233900739386466605, 6.101867874933233793, -22.94418644579999977 ) ) ;
#23486 = DIRECTION ( 'NONE',  ( 0.000000000000000000, 0.000000000000000000, -1.000000000000000000 ) ) ;
#23487 = PRODUCT ( 'Catch Spring', 'Catch Spring', '', ( #24392 ) ) ;
#23488 = CARTESIAN_POINT ( 'NONE',  ( -3.494139924891833893, -1.791588778288840000, -92.88964426498927196 ) ) ;
#23489 = EDGE_CURVE ( 'NONE', #13152, #3686, #14835, .T. ) ;
#23490 = CARTESIAN_POINT ( 'NONE',  ( -1.091910126179790330, 3.499798787991532212, 227.7419800002291197 ) ) ;
#23491 = CARTESIAN_POINT ( 'NONE',  ( -1.030301836990161535, 20.00000000003602452, -0.6999999999999784173 ) ) ;
#23492 = CARTESIAN_POINT ( 'NONE',  ( -24.07583586439999834, -13.90018868249999962, 226.1000014189999945 ) ) ;
#23493 = COLOUR_RGB ( '', 0.31764706, 0.68627451, 0.89019608) ;
#23494 = EDGE_CURVE ( 'NONE', #29062, #28672, #27717, .T. ) ;
#23495 = AXIS2_PLACEMENT_3D ( 'NONE', #13674, #23278, #25485 ) ;
#23496 = CARTESIAN_POINT ( 'NONE',  ( 27.79999999999999716, 2.355804440410000085E-11, 229.0000000000000000 ) ) ;
#23497 = CARTESIAN_POINT ( 'NONE',  ( 5.414213562369999622, -31.28896728272270877, -80.26658230080884948 ) ) ;
#23498 = DIRECTION ( 'NONE',  ( 1.000000000000000000, -0.000000000000000000, 0.000000000000000000 ) ) ;
#23499 = ORIENTED_EDGE ( 'NONE', *, *, #4048, .T. ) ;
#23500 = CARTESIAN_POINT ( 'NONE',  ( -4.300317018729668206, 2.364939115720630980, -59.81908057272499946 ) ) ;
#23501 = CARTESIAN_POINT ( 'NONE',  ( -1.484924240490000047, -1.484924240490000047, 226.6412452697800006 ) ) ;
#23502 = EDGE_CURVE ( 'NONE', #24111, #24506, #30950, .T. ) ;
#23503 = CARTESIAN_POINT ( 'NONE',  ( 1.000415564564199444, -28.48292217093161938, 3.997481721999984750 ) ) ;
#23504 = PLANE ( 'NONE',  #12306 ) ;
#23505 = ORIENTED_EDGE ( 'NONE', *, *, #25652, .T. ) ;
#23506 = CARTESIAN_POINT ( 'NONE',  ( -23.88764392071930587, 14.22151635026485117, 4.322084506810967675 ) ) ;
#23507 = CARTESIAN_POINT ( 'NONE',  ( 21.30888436558567633, -16.34772642260384856, 186.7828584119999960 ) ) ;
#23508 = ORIENTED_EDGE ( 'NONE', *, *, #15014, .T. ) ;
#23509 = ORIENTED_EDGE ( 'NONE', *, *, #4559, .T. ) ;
#23510 = ORIENTED_EDGE ( 'NONE', *, *, #24825, .T. ) ;
#23511 = B_SPLINE_SURFACE_WITH_KNOTS ( 'NONE', 5, 1, ( 
 ( #13432, #30275 ),
 ( #10462, #5729 ),
 ( #1022, #10610 ),
 ( #29796, #8228 ),
 ( #4469, #11394 ),
 ( #16261, #30743 ),
 ( #16110, #28535 ),
 ( #14068, #1644 ),
 ( #15956, #8863 ),
 ( #9492, #30597 ),
 ( #18468, #9333 ),
 ( #6822, #23365 ),
 ( #16420, #11234 ),
 ( #21147, #23827 ),
 ( #26029, #28066 ),
 ( #4613, #23203 ),
 ( #14221, #6982 ),
 ( #30443, #23673 ),
 ( #6662, #2107 ),
 ( #11700, #18933 ),
 ( #4315, #4156 ),
 ( #16571, #6510 ),
 ( #30904, #21303 ),
 ( #28220, #26177 ),
 ( #31056, #19094 ),
 ( #9173, #2271 ),
 ( #13911, #11857 ) ),
 .UNSPECIFIED., .F., .F., .F.,
 ( 6, 3, 3, 3, 3, 3, 3, 3, 6 ),
 ( 2, 2 ),
 ( 0.000000000000000000, 12.04914910469999967, 24.12830621100000172, 36.22018076730000047, 48.28758829720000278, 60.33208762030000116, 72.38455155859999479, 84.43687076610000020, 88.75867308210000317 ),
 ( -2.393070191420000080E-05, 0.7036780443879999680 ),
 .UNSPECIFIED. ) ;
#23512 =( NAMED_UNIT ( * ) SI_UNIT ( $, .STERADIAN. ) SOLID_ANGLE_UNIT ( ) );
#23513 = EDGE_LOOP ( 'NONE', ( #5719, #11148, #18847, #2791 ) ) ;
#23514 = CARTESIAN_POINT ( 'NONE',  ( 24.88589369718092215, -13.89120818692358483, 6.095967889000020179 ) ) ;
#23515 = VECTOR ( 'NONE', #12894, 1000.000000000000000 ) ;
#23516 = EDGE_CURVE ( 'NONE', #24719, #10063, #6864, .T. ) ;
#23517 = LINE ( 'NONE', #6505, #27521 ) ;
#23518 = CARTESIAN_POINT ( 'NONE',  ( -5.606848515966891711, 1.848691355091094835, -68.74019511502498858 ) ) ;
#23519 = FILL_AREA_STYLE ('',( #26024 ) ) ;
#23520 = VECTOR ( 'NONE', #22917, 1000.000000000000000 ) ;
#23521 = CARTESIAN_POINT ( 'NONE',  ( 7.100352917962720056, -6.872658567668013418, -34.12714961758439358 ) ) ;
#23522 = CARTESIAN_POINT ( 'NONE',  ( -4.084346732781016343, 0.2146938847797513761, -40.92168819672095736 ) ) ;
#23523 = FACE_OUTER_BOUND ( 'NONE', #15467, .T. ) ;
#23524 = ORIENTED_EDGE ( 'NONE', *, *, #6043, .T. ) ;
#23525 = EDGE_CURVE ( 'NONE', #29098, #18993, #16278, .T. ) ;
#23526 = CARTESIAN_POINT ( 'NONE',  ( -19.53717638892995723, 20.00009241111888159, -0.2444329966749828886 ) ) ;
#23527 = CARTESIAN_POINT ( 'NONE',  ( 3.665953941183818010, 4.858601989977915814, -13.62796858839999992 ) ) ;
#23528 = CARTESIAN_POINT ( 'NONE',  ( 25.43291179139270142, -8.631520107455976643, -0.000000000000000000 ) ) ;
#23529 = CARTESIAN_POINT ( 'NONE',  ( -10.69999999968266913, -25.03385111784779227, -30.95943383852850062 ) ) ;
#23530 = VERTEX_POINT ( 'NONE', #4360 ) ;
#23531 = CARTESIAN_POINT ( 'NONE',  ( 23.35460918733123847, 13.32399080374418787, -1.399999999999998801 ) ) ;
#23532 = CARTESIAN_POINT ( 'NONE',  ( -8.699999999683917906, -16.84112679184576677, -33.19732076807623145 ) ) ;
#23533 = CARTESIAN_POINT ( 'NONE',  ( 0.8260714174469999671, -28.48835664879999996, 225.7596297540000023 ) ) ;
#23534 = CARTESIAN_POINT ( 'NONE',  ( 23.13573312470881405, -13.52773475764968225, 3.899999999999999911 ) ) ;
#23535 = CARTESIAN_POINT ( 'NONE',  ( -1.595193757947241497, 6.212219048941578059, -66.20876360962500939 ) ) ;
#23536 = CIRCLE ( 'NONE', #16974, 3.200000000000002398 ) ;
#23537 = DIRECTION ( 'NONE',  ( 0.000000000000000000, 0.000000000000000000, 1.000000000000000000 ) ) ;
#23538 = CARTESIAN_POINT ( 'NONE',  ( 16.08958307952436328, 11.26717219148106786, -0.6999999999999784173 ) ) ;
#23539 = ORIENTED_EDGE ( 'NONE', *, *, #5831, .F. ) ;
#23540 = DIRECTION ( 'NONE',  ( 0.000000000000000000, -0.000000000000000000, 1.000000000000000000 ) ) ;
#23541 = CARTESIAN_POINT ( 'NONE',  ( -16.85343921402336775, -7.900182044543379689, -0.6999999999999784173 ) ) ;
#23542 = AXIS2_PLACEMENT_3D ( 'NONE', #7617, #9524, #4954 ) ;
#23543 = B_SPLINE_CURVE_WITH_KNOTS ( 'NONE', 3,
 ( #4210, #11298, #16013, #13493, #18527, #20901, #8925, #23582, #15861, #8603, #28129, #18044, #13340, #6415 ),
 .UNSPECIFIED., .F., .F.,
 ( 4, 2, 2, 1, 1, 2, 2, 4 ),
 ( 0.000000000000000000, 0.2500000000000140998, 0.3750000000000173750, 0.4375000000000172640, 0.4687500000000170974, 0.4843750000000187073, 0.5000000000000203171, 1.000000000000000000 ),
 .UNSPECIFIED. ) ;
#23544 = CARTESIAN_POINT ( 'NONE',  ( 2.875056473737671592, -3.558337944997149283, -68.10000000002501963 ) ) ;
#23545 = VECTOR ( 'NONE', #26290, 1000.000000000000000 ) ;
#23546 = CARTESIAN_POINT ( 'NONE',  ( 3.415131431000496764, 0.8926240808846060970, -0.6999999999999785283 ) ) ;
#23547 = CARTESIAN_POINT ( 'NONE',  ( -2.467959925502309915, -3.051731433341752453, -44.10000000002498410 ) ) ;
#23548 =( NAMED_UNIT ( * ) SI_UNIT ( $, .STERADIAN. ) SOLID_ANGLE_UNIT ( ) );
#23549 = VERTEX_POINT ( 'NONE', #26534 ) ;
#23550 = CARTESIAN_POINT ( 'NONE',  ( -12.32633706535996154, 0.2818134420149785435, 232.6627637660202197 ) ) ;
#23551 = ADVANCED_FACE ( 'NONE', ( #29041 ), #11746, .T. ) ;
#23552 = CARTESIAN_POINT ( 'NONE',  ( -4.919493655965280432, -0.2618778636566052032, -66.31421022022500722 ) ) ;
#23553 = VERTEX_POINT ( 'NONE', #9376 ) ;
#23554 = CARTESIAN_POINT ( 'NONE',  ( -22.06837820954319440, 15.41983382789281620, 0.000000000000000000 ) ) ;
#23555 = AXIS2_PLACEMENT_3D ( 'NONE', #14654, #12431, #26755 ) ;
#23556 = EDGE_CURVE ( 'NONE', #21828, #28697, #15782, .T. ) ;
#23557 = ADVANCED_FACE ( 'NONE', ( #28587 ), #16970, .T. ) ;
#23558 = CARTESIAN_POINT ( 'NONE',  ( -3.458129700889219116, 0.5397582531354577773, -88.52261276322501260 ) ) ;
#23559 = ORIENTED_EDGE ( 'NONE', *, *, #11521, .T. ) ;
#23560 = DIRECTION ( 'NONE',  ( -1.000000000000000000, 0.000000000000000000, -6.771000000000000128E-12 ) ) ;
#23561 = DIRECTION ( 'NONE',  ( 0.000000000000000000, 0.000000000000000000, 1.000000000000000000 ) ) ;
#23562 = DIRECTION ( 'NONE',  ( 0.7071067811865466846, -1.595945597898659700E-12, -0.7071067811865484609 ) ) ;
#23563 = CARTESIAN_POINT ( 'NONE',  ( 10.69999999994010587, -26.89354272454766814, -15.86444061765503122 ) ) ;
#23564 = PRODUCT_DEFINITION_CONTEXT ( 'detailed design', #1543, 'design' ) ;
#23565 = CARTESIAN_POINT ( 'NONE',  ( -0.5944614571882205212, -27.79380703160649446, 4.895947184000021046 ) ) ;
#23566 = CIRCLE ( 'NONE', #30079, 4.000000004070001225 ) ;
#23567 = CARTESIAN_POINT ( 'NONE',  ( -12.44217317843894222, -22.00000000000000355, -26.84827175176876324 ) ) ;
#23568 = CARTESIAN_POINT ( 'NONE',  ( 0.000000000000000000, 0.000000000000000000, 90.00000000000000000 ) ) ;
#23569 = VERTEX_POINT ( 'NONE', #20490 ) ;
#23570 = CARTESIAN_POINT ( 'NONE',  ( 14.40197535836999876, -32.00000000000000000, -25.51324865394999719 ) ) ;
#23571 = CARTESIAN_POINT ( 'NONE',  ( 10.69999999996289652, -28.79065839761292978, -25.96313344405833234 ) ) ;
#23572 = CARTESIAN_POINT ( 'NONE',  ( 19.79266700209999996, 19.51190850369999907, 229.1494847489999813 ) ) ;
#23573 = CARTESIAN_POINT ( 'NONE',  ( -19.80526803549999926, 19.50877411510000314, 229.0000000000000000 ) ) ;
#23574 = B_SPLINE_CURVE_WITH_KNOTS ( 'NONE', 3,
 ( #30161, #10240, #8433, #27801, #10973, #29424, #17462, #15681, #10393, #2839, #12434, #25456 ),
 .UNSPECIFIED., .F., .F.,
 ( 4, 2, 2, 2, 2, 4 ),
 ( 0.000000000000000000, 0.1249999999999999445, 0.2499999999999998890, 0.5000000000000000000, 0.7500000000000001110, 1.000000000000000000 ),
 .UNSPECIFIED. ) ;
#23575 = CARTESIAN_POINT ( 'NONE',  ( 17.04261818891856350, -10.10243747014645521, -0.6999999999999783062 ) ) ;
#23576 = CARTESIAN_POINT ( 'NONE',  ( -0.3738033647169999862, -27.79799560440000050, 226.0423263479999889 ) ) ;
#23577 = CARTESIAN_POINT ( 'NONE',  ( 8.700000000249431764, -26.69088343938642538, -31.40976070819087695 ) ) ;
#23578 = CARTESIAN_POINT ( 'NONE',  ( -16.25551851031397632, 10.05302898035984605, -1.400000000000001688 ) ) ;
#23579 = CARTESIAN_POINT ( 'NONE',  ( -3.985743628842679076, -2.180176701716177057, -53.34982952342500084 ) ) ;
#23580 = VECTOR ( 'NONE', #26383, 1000.000000000000000 ) ;
#23581 = CARTESIAN_POINT ( 'NONE',  ( 27.15000000039999861, -3.324806250660000050E-15, 230.0000000000000000 ) ) ;
#23582 = CARTESIAN_POINT ( 'NONE',  ( 14.75144444200372718, -28.36701773692398731, -33.38425558406653693 ) ) ;
#23583 = CARTESIAN_POINT ( 'NONE',  ( 3.430548664023152838, -1.057777877209630901, 230.7844944799449820 ) ) ;
#23584 = FACE_BOUND ( 'NONE', #900, .T. ) ;
#23585 = CARTESIAN_POINT ( 'NONE',  ( 9.000000000000000000, -55.00000000000000000, -44.10000000000000142 ) ) ;
#23586 = AXIS2_PLACEMENT_3D ( 'NONE', #27965, #1068, #3894 ) ;
#23587 = ORIENTED_EDGE ( 'NONE', *, *, #19830, .T. ) ;
#23588 = CARTESIAN_POINT ( 'NONE',  ( -1.256295066205788347, -5.815478746186413694, -55.93033560642499680 ) ) ;
#23589 = EDGE_LOOP ( 'NONE', ( #14942, #24011, #5076, #15592 ) ) ;
#23590 = ORIENTED_EDGE ( 'NONE', *, *, #5663, .T. ) ;
#23591 = DIRECTION ( 'NONE',  ( -1.000000000000000000, 5.665498452320000818E-16, 0.000000000000000000 ) ) ;
#23592 = EDGE_CURVE ( 'NONE', #1959, #18650, #17391, .T. ) ;
#23593 = EDGE_LOOP ( 'NONE', ( #14238, #29982, #24258, #30083 ) ) ;
#23594 = DIRECTION ( 'NONE',  ( 1.000000000000000000, 7.807837518093016606E-13, 2.626330150305131362E-12 ) ) ;
#23595 = CARTESIAN_POINT ( 'NONE',  ( -9.897162125403687227, -25.37356426577970581, 91.66046017469999185 ) ) ;
#23596 = CARTESIAN_POINT ( 'NONE',  ( -17.04621913067799710, -27.00000000059169736, -22.62649730796000114 ) ) ;
#23597 = AXIS2_PLACEMENT_3D ( 'NONE', #4791, #5240, #19255 ) ;
#23598 = CARTESIAN_POINT ( 'NONE',  ( -6.982632971260604116, 4.357143524085962838, -42.94209588230350505 ) ) ;
#23599 = CARTESIAN_POINT ( 'NONE',  ( -24.68204616399999907, -14.25020164319999871, 223.9000014189999774 ) ) ;
#23600 = CYLINDRICAL_SURFACE ( 'NONE', #9406, 26.80000000000000071 ) ;
#23601 = CARTESIAN_POINT ( 'NONE',  ( -5.082228009654736312, -3.365126390422853220, -6.289929326000004650 ) ) ;
#23602 = CARTESIAN_POINT ( 'NONE',  ( -13.50216071430000042, -27.11059322570000418, 230.6577119970000069 ) ) ;
#23603 = ORIENTED_EDGE ( 'NONE', *, *, #24886, .T. ) ;
#23604 = CARTESIAN_POINT ( 'NONE',  ( 0.000000000000000000, 0.000000000000000000, 230.0000000000000000 ) ) ;
#23605 = CARTESIAN_POINT ( 'NONE',  ( 4.130711734062741947, 1.221343755424970201, -18.04190840230000958 ) ) ;
#23606 = CARTESIAN_POINT ( 'NONE',  ( -1.100001242879427243, -27.77850260588756015, 225.1469357386177421 ) ) ;
#23607 = TOROIDAL_SURFACE ( 'NONE', #9007, 5.792819795519999815, 3.000000000000000000 ) ;
#23608 = CARTESIAN_POINT ( 'NONE',  ( 28.35455043824866550, 0.5159221438580675612, 0.2374258030000131470 ) ) ;
#23609 = CARTESIAN_POINT ( 'NONE',  ( -17.99585043762395742, 19.96083428726235809, 0.000000000000000000 ) ) ;
#23610 = CARTESIAN_POINT ( 'NONE',  ( 23.98155922632636816, -15.68763507556827541, 8.000000000000007105 ) ) ;
#23611 = CARTESIAN_POINT ( 'NONE',  ( -17.99585043762395742, 19.96083428726235809, 0.000000000000000000 ) ) ;
#23612 = CARTESIAN_POINT ( 'NONE',  ( 27.29371452669260734, 0.4966198192112817322, -0.6577119969999878357 ) ) ;
#23613 = CARTESIAN_POINT ( 'NONE',  ( -12.41421356240000051, 26.55509710711128335, -61.34142017886538412 ) ) ;
#23614 = CARTESIAN_POINT ( 'NONE',  ( 24.93720649360215802, -13.79881813812812297, 3.899998581000013509 ) ) ;
#23615 = EDGE_CURVE ( 'NONE', #9708, #9436, #28338, .T. ) ;
#23616 = CARTESIAN_POINT ( 'NONE',  ( -11.39379051978746915, 21.69999999994131556, -70.10000000020002631 ) ) ;
#23617 = ORIENTED_EDGE ( 'NONE', *, *, #17586, .F. ) ;
#23618 = CARTESIAN_POINT ( 'NONE',  ( 8.700000000249179521, -24.10030203291533368, -29.26452672280898781 ) ) ;
#23619 = FACE_OUTER_BOUND ( 'NONE', #5861, .T. ) ;
#23620 = CARTESIAN_POINT ( 'NONE',  ( 0.000000000000000000, 0.000000000000000000, 0.000000000000000000 ) ) ;
#23621 = CARTESIAN_POINT ( 'NONE',  ( -0.8383234616028363284, -5.156720310874200131, -0.7000226318098609068 ) ) ;
#23622 = ORIENTED_EDGE ( 'NONE', *, *, #19968, .F. ) ;
#23623 = CARTESIAN_POINT ( 'NONE',  ( 10.69999999999999929, -24.00000000000000000, -28.40000000000000213 ) ) ;
#23624 = ORIENTED_EDGE ( 'NONE', *, *, #24279, .F. ) ;
#23625 = ORIENTED_EDGE ( 'NONE', *, *, #27192, .T. ) ;
#23626 = CARTESIAN_POINT ( 'NONE',  ( 0.000000000000000000, 0.000000000000000000, 0.000000000000000000 ) ) ;
#23627 = AXIS2_PLACEMENT_3D ( 'NONE', #4650, #2146, #4188 ) ;
#23628 = VERTEX_POINT ( 'NONE', #14731 ) ;
#23629 = CARTESIAN_POINT ( 'NONE',  ( -16.81341597784800967, -10.09981795476353739, 0.000000000000000000 ) ) ;
#23630 = ORIENTED_EDGE ( 'NONE', *, *, #5060, .F. ) ;
#23631 = CARTESIAN_POINT ( 'NONE',  ( -24.60699806910000120, -12.93667933180000063, 225.1042194559999814 ) ) ;
#23632 = CARTESIAN_POINT ( 'NONE',  ( -7.105427357599999217E-15, -7.105427357599999217E-15, 186.7828584120000244 ) ) ;
#23633 = CARTESIAN_POINT ( 'NONE',  ( 3.235226967573094914, 2.011182562232342708, -35.69999999999999574 ) ) ;
#23634 = CARTESIAN_POINT ( 'NONE',  ( 19.28276787503908452, 20.00015277968180882, -0.3880171390712462420 ) ) ;
#23635 = CARTESIAN_POINT ( 'NONE',  ( 26.22084555198160771, -5.650681821715154207, -1.399999999999998579 ) ) ;
#23636 = CARTESIAN_POINT ( 'NONE',  ( -4.175165894169885483, -50.49316738903675628, -43.39999999999999858 ) ) ;
#23637 = DIRECTION ( 'NONE',  ( 0.9595496282943491995, -0.2815395369041025497, 0.000000000000000000 ) ) ;
#23638 = ORIENTED_EDGE ( 'NONE', *, *, #18560, .T. ) ;
#23639 = CARTESIAN_POINT ( 'NONE',  ( 1.765446408317208560, -4.831419061753667421, -7.198085232199999517 ) ) ;
#23640 = CARTESIAN_POINT ( 'NONE',  ( 1.566980368899947962, 4.067530462867743779, -26.09462237480000724 ) ) ;
#23641 = DIRECTION ( 'NONE',  ( 0.9316362575375356503, 0.3633921898465274913, 0.000000000000000000 ) ) ;
#23642 = CARTESIAN_POINT ( 'NONE',  ( -3.213922572545196310, -4.048003670336641768, -93.88815951138718674 ) ) ;
#23643 = DIRECTION ( 'NONE',  ( -1.000000000000000000, 0.000000000000000000, 0.000000000000000000 ) ) ;
#23644 = CYLINDRICAL_SURFACE ( 'NONE', #92, 1.100000000000002309 ) ;
#23645 = CARTESIAN_POINT ( 'NONE',  ( -24.15901410609999900, -15.12012600319999933, 225.5071239680000303 ) ) ;
#23646 = ADVANCED_FACE ( 'NONE', ( #10009 ), #19607, .T. ) ;
#23647 = VECTOR ( 'NONE', #8865, 1000.000000000000227 ) ;
#23648 = CARTESIAN_POINT ( 'NONE',  ( 24.25496636523650551, -13.58595625263505013, 6.099998581000014575 ) ) ;
#23649 = APPLICATION_CONTEXT ( 'automotive_design' ) ;
#23650 = CARTESIAN_POINT ( 'NONE',  ( 0.7459188900473354700, -27.79046661982714639, 6.079790450999988494 ) ) ;
#23651 = DIRECTION ( 'NONE',  ( -0.9316362575375349842, 0.3633921898465292122, -0.000000000000000000 ) ) ;
#23652 = ORIENTED_EDGE ( 'NONE', *, *, #26550, .F. ) ;
#23653 = CARTESIAN_POINT ( 'NONE',  ( 5.433585117924402574, 2.226379967917181180, -60.09141554682499731 ) ) ;
#23654 = CARTESIAN_POINT ( 'NONE',  ( -1.053429623273372640, -1.822228224019613485, 226.6412452697799154 ) ) ;
#23655 = EDGE_CURVE ( 'NONE', #27389, #2398, #13090, .T. ) ;
#23656 = CARTESIAN_POINT ( 'NONE',  ( 8.700000000273238498, -16.53478705811768990, -33.08035312245812776 ) ) ;
#23657 = CARTESIAN_POINT ( 'NONE',  ( -4.901082056042067592, -4.330235462241937228, -33.83447003409999354 ) ) ;
#23658 = ORIENTED_EDGE ( 'NONE', *, *, #26147, .T. ) ;
#23659 = B_SPLINE_CURVE_WITH_KNOTS ( 'NONE', 1,
 ( #29748, #14830 ),
 .UNSPECIFIED., .F., .F.,
 ( 2, 2 ),
 ( -0.7031447686210000603, -5.021915139291621699E-08 ),
 .UNSPECIFIED. ) ;
#23660 = DIRECTION ( 'NONE',  ( 1.000000000000000000, -1.843431230200084908E-12, 2.650498504963248473E-12 ) ) ;
#23661 = PLANE ( 'NONE',  #24349 ) ;
#23662 = ORIENTED_EDGE ( 'NONE', *, *, #28939, .T. ) ;
#23663 = ORIENTED_EDGE ( 'NONE', *, *, #1962, .F. ) ;
#23664 = EDGE_LOOP ( 'NONE', ( #15039, #484, #13388, #15095 ) ) ;
#23665 = ORIENTED_EDGE ( 'NONE', *, *, #30739, .F. ) ;
#23666 = DIRECTION ( 'NONE',  ( 9.219210260491733511E-13, 0.9128796883888953273, -0.4082287037029530552 ) ) ;
#23667 = LINE ( 'NONE', #14215, #17967 ) ;
#23668 = B_SPLINE_CURVE_WITH_KNOTS ( 'NONE', 5,
 ( #27435, #29328, #19901, #3207, #714, #15023, #29483, #3356, #7922 ),
 .UNSPECIFIED., .F., .F.,
 ( 6, 3, 6 ),
 ( 0.000000000000000000, 6.585791975970000323, 10.75845894650000112 ),
 .UNSPECIFIED. ) ;
#23669 = CARTESIAN_POINT ( 'NONE',  ( -4.185763533044374540, 4.163314928055855901, -68.94322600512501253 ) ) ;
#23670 = CARTESIAN_POINT ( 'NONE',  ( 25.33947091559999976, -14.52216050880000076, 229.4485726019999845 ) ) ;
#23671 = EDGE_CURVE ( 'NONE', #27935, #16211, #27564, .T. ) ;
#23672 = CARTESIAN_POINT ( 'NONE',  ( 9.999999999959999997, -36.62914859500000375, -26.86371135770000151 ) ) ;
#23673 = CARTESIAN_POINT ( 'NONE',  ( 18.73270429609999965, -20.74707689250000087, 222.0000000000000000 ) ) ;
#23674 = CARTESIAN_POINT ( 'NONE',  ( 3.718425205896203067, -3.001845489190030136, -0.7000011950963532792 ) ) ;
#23675 = ORIENTED_EDGE ( 'NONE', *, *, #3105, .T. ) ;
#23676 = CARTESIAN_POINT ( 'NONE',  ( -20.07475214973380773, 19.99999824547289862, 0.2739201808243049152 ) ) ;
#23677 = AXIS2_PLACEMENT_3D ( 'NONE', #1980, #26356, #31074 ) ;
#23678 = CARTESIAN_POINT ( 'NONE',  ( 3.390625094264292372, -3.362288366427768072, -14.12362212869999745 ) ) ;
#23679 = DIRECTION ( 'NONE',  ( 0.000000000000000000, 1.000000000000000000, 0.000000000000000000 ) ) ;
#23680 = B_SPLINE_CURVE_WITH_KNOTS ( 'NONE', 5,
 ( #16095, #18131, #18453, #8847, #18291, #1630, #28051, #11220, #20346, #3658, #27898, #27733, #15779, #23347, #1790 ),
 .UNSPECIFIED., .F., .F.,
 ( 6, 3, 3, 3, 6 ),
 ( 0.000000000000000000, 0.1000000000022905483, 0.4000000000034356629, 0.7000000000005726086, 1.000000000000000000 ),
 .UNSPECIFIED. ) ;
#23681 = DIRECTION ( 'NONE',  ( 0.000000000000000000, 0.000000000000000000, -1.000000000000000000 ) ) ;
#23682 = ORIENTED_EDGE ( 'NONE', *, *, #6232, .F. ) ;
#23683 = CARTESIAN_POINT ( 'NONE',  ( 26.80813537125358081, 0.8641279371233817619, -1.399999999999998579 ) ) ;
#23684 = CARTESIAN_POINT ( 'NONE',  ( -10.69999999999999929, -129.8920065082999997, -39.38774058400999678 ) ) ;
#23685 = DIRECTION ( 'NONE',  ( -1.000000000000000000, 0.000000000000000000, 0.000000000000000000 ) ) ;
#23686 = CARTESIAN_POINT ( 'NONE',  ( 11.02573875750000099, -24.63456739829999975, -1.660048601699999571 ) ) ;
#23687 = CARTESIAN_POINT ( 'NONE',  ( -2.744116393020877620, -4.299119443564640264, -68.10000000002500542 ) ) ;
#23688 = EDGE_CURVE ( 'NONE', #17409, #18614, #27324, .T. ) ;
#23689 = CARTESIAN_POINT ( 'NONE',  ( -24.68204616399999907, -14.25020164319999871, 223.9000014189999774 ) ) ;
#23690 = CARTESIAN_POINT ( 'NONE',  ( 10.69999999997514095, -121.7823864053157195, -31.38636738194435694 ) ) ;
#23691 = ORIENTED_EDGE ( 'NONE', *, *, #16182, .T. ) ;
#23692 = CARTESIAN_POINT ( 'NONE',  ( 17.16657240410000185, 10.99999999889999458, -0.6999999999999992895 ) ) ;
#23693 = CARTESIAN_POINT ( 'NONE',  ( -7.999999999668092165, -18.32608219842778752, -34.72428978364464314 ) ) ;
#23694 = B_SPLINE_CURVE_WITH_KNOTS ( 'NONE', 3,
 ( #17780, #17930, #30064, #3316, #18091, #29751, #822, #5833, #15281, #8034, #1120, #20309 ),
 .UNSPECIFIED., .F., .F.,
 ( 4, 2, 2, 2, 2, 4 ),
 ( 0.000000000000000000, 0.2500000000000002776, 0.3750000000000002776, 0.5000000000000003331, 0.7500000000000001110, 1.000000000000000000 ),
 .UNSPECIFIED. ) ;
#23695 = CARTESIAN_POINT ( 'NONE',  ( -6.999999999597122269, -114.8328013979413527, 22.59891173954833477 ) ) ;
#23696 = CARTESIAN_POINT ( 'NONE',  ( 10.00000000060000005, -25.00000000000000000, -7.274962170899998526 ) ) ;
#23697 = EDGE_CURVE ( 'NONE', #12690, #13120, #3738, .T. ) ;
#23698 = CARTESIAN_POINT ( 'NONE',  ( 27.23548387060000309, -1.776356839399999804E-15, 188.3395398250000028 ) ) ;
#23699 = CARTESIAN_POINT ( 'NONE',  ( 3.389121577140000063, 11.55088360979999962, 230.6412452697800006 ) ) ;
#23700 = ORIENTED_EDGE ( 'NONE', *, *, #29385, .T. ) ;
#23701 = DIRECTION ( 'NONE',  ( 0.000000000000000000, 0.000000000000000000, 1.000000000000000000 ) ) ;
#23702 = CARTESIAN_POINT ( 'NONE',  ( 7.638687372290002386, 3.765626869274008026, -39.31578811164669673 ) ) ;
#23703 = EDGE_LOOP ( 'NONE', ( #17022, #1062 ) ) ;
#23704 = CARTESIAN_POINT ( 'NONE',  ( 24.83827260360999389, -12.48687744688666967, 4.999998581000003384 ) ) ;
#23705 = ADVANCED_FACE ( 'NONE', ( #26994 ), #24634, .F. ) ;
#23706 = CARTESIAN_POINT ( 'NONE',  ( 3.458129700889219116, -0.5397582531354573332, -88.52261276322501260 ) ) ;
#23707 = ORIENTED_EDGE ( 'NONE', *, *, #17169, .T. ) ;
#23708 = LINE ( 'NONE', #14415, #11555 ) ;
#23709 = PRODUCT_RELATED_PRODUCT_CATEGORY ( 'part', '', ( #23487 ) ) ;
#23710 = CARTESIAN_POINT ( 'NONE',  ( -23.39354070940022723, -15.01969650296710768, 4.239862999000004962 ) ) ;
#23711 = DIRECTION ( 'NONE',  ( -1.000000000000000000, 1.843431230205392516E-12, -2.650498504954667282E-12 ) ) ;
#23712 = CARTESIAN_POINT ( 'NONE',  ( -10.69999999999999929, -24.04799545849999731, -27.72121045900000169 ) ) ;
#23713 = CARTESIAN_POINT ( 'NONE',  ( 26.80000000000000071, -1.776356839399999804E-15, 43.21714158840000408 ) ) ;
#23714 = CARTESIAN_POINT ( 'NONE',  ( -9.000000000229999131, 21.70000000000000284, -58.10000000000000142 ) ) ;
#23715 = ORIENTED_EDGE ( 'NONE', *, *, #13033, .F. ) ;
#23716 = CARTESIAN_POINT ( 'NONE',  ( -26.80000000069999899, 3.281945028329999726E-15, 193.2171415869999862 ) ) ;
#23717 = CARTESIAN_POINT ( 'NONE',  ( 24.09856112909999837, -15.21545593799999985, 225.1041867410000350 ) ) ;
#23718 = FACE_OUTER_BOUND ( 'NONE', #19257, .T. ) ;
#23719 = CARTESIAN_POINT ( 'NONE',  ( -19.80526803560000104, 19.50877411520000138, 223.3999999999999773 ) ) ;
#23720 = VECTOR ( 'NONE', #2921, 1000.000000000000000 ) ;
#23721 = CARTESIAN_POINT ( 'NONE',  ( 8.700000000235821318, -29.73863906516063693, -27.17531388883607590 ) ) ;
#23722 = CARTESIAN_POINT ( 'NONE',  ( -0.06887222117140000266, -27.80017212539999960, 226.0986539140000104 ) ) ;
#23723 = CARTESIAN_POINT ( 'NONE',  ( 0.000000000000000000, 0.000000000000000000, 188.3395398250000028 ) ) ;
#23724 = EDGE_CURVE ( 'NONE', #17896, #18728, #9361, .T. ) ;
#23725 = AXIS2_PLACEMENT_3D ( 'NONE', #28289, #9090, #25942 ) ;
#23726 = CARTESIAN_POINT ( 'NONE',  ( -28.49530731802708416, -0.5184832703812605192, 8.000000000000007105 ) ) ;
#23727 = CIRCLE ( 'NONE', #11153, 0.9999999999999991118 ) ;
#23728 = DIRECTION ( 'NONE',  ( 0.000000000000000000, -1.000000000000000000, 0.000000000000000000 ) ) ;
#23729 = CARTESIAN_POINT ( 'NONE',  ( -3.469775141984876576, 3.953596984329539321, -53.23587006832500634 ) ) ;
#23730 = EDGE_CURVE ( 'NONE', #27396, #28115, #8177, .T. ) ;
#23731 = CARTESIAN_POINT ( 'NONE',  ( -7.999999999728899525, -28.83899161331666150, -25.99720916226845091 ) ) ;
#23732 = CARTESIAN_POINT ( 'NONE',  ( -27.79999999999999716, -2.358405305979999929E-11, 229.1414213560000235 ) ) ;
#23733 = CARTESIAN_POINT ( 'NONE',  ( 7.572771919626319459, -115.1908526478854071, 21.79823870879123504 ) ) ;
#23734 = ORIENTED_EDGE ( 'NONE', *, *, #6449, .F. ) ;
#23735 = FACE_OUTER_BOUND ( 'NONE', #30039, .T. ) ;
#23736 = CARTESIAN_POINT ( 'NONE',  ( 4.457006042266220547, -0.7452897422089094226, -36.68267599850000238 ) ) ;
#23737 = AXIS2_PLACEMENT_3D ( 'NONE', #28228, #9503, #19103 ) ;
#23738 = CARTESIAN_POINT ( 'NONE',  ( 4.692739937114382087, 0.5303478879429707193, -55.41771407622499623 ) ) ;
#23739 = ORIENTED_EDGE ( 'NONE', *, *, #10797, .F. ) ;
#23740 = CONTEXT_DEPENDENT_SHAPE_REPRESENTATION ( #14819, #9465 ) ;
#23741 = AXIS2_PLACEMENT_3D ( 'NONE', #27188, #29702, #19649 ) ;
#23742 = VERTEX_POINT ( 'NONE', #23018 ) ;
#23743 = CARTESIAN_POINT ( 'NONE',  ( -10.00000000070000183, -27.00000000000000000, -28.40000000000000213 ) ) ;
#23744 = ORIENTED_EDGE ( 'NONE', *, *, #22783, .F. ) ;
#23745 = DIRECTION ( 'NONE',  ( 1.000000000000000000, -1.843431230198065424E-12, 2.650498504953516580E-12 ) ) ;
#23746 = CARTESIAN_POINT ( 'NONE',  ( -8.699999999660271044, -9.763725516012462080, -36.23155182226569337 ) ) ;
#23747 =( NAMED_UNIT ( * ) PLANE_ANGLE_UNIT ( ) SI_UNIT ( $, .RADIAN. ) );
#23748 = B_SPLINE_CURVE_WITH_KNOTS ( 'NONE', 5,
 ( #21272, #8833, #6795, #18906, #1775, #21433 ),
 .UNSPECIFIED., .F., .F.,
 ( 6, 6 ),
 ( -88.61406016669999985, -71.78006588680000277 ),
 .UNSPECIFIED. ) ;
#23749 = CARTESIAN_POINT ( 'NONE',  ( -2.703235379809999728, -11.76103604130000058, 231.9999991140000191 ) ) ;
#23750 = DIRECTION ( 'NONE',  ( 0.000000000000000000, 0.000000000000000000, -1.000000000000000000 ) ) ;
#23751 = CARTESIAN_POINT ( 'NONE',  ( -2.220446049249999755E-16, -0.1455297029551360921, -71.05965357398815740 ) ) ;
#23752 = CARTESIAN_POINT ( 'NONE',  ( 1.604951280288043014, -4.392199147046020435, -6.260585232200001293 ) ) ;
#23753 = CARTESIAN_POINT ( 'NONE',  ( 20.82782576890000215, -20.96114668230000078, 230.2432540810000319 ) ) ;
#23754 = VERTEX_POINT ( 'NONE', #24327 ) ;
#23755 = CARTESIAN_POINT ( 'NONE',  ( 1.597375353785503327, -4.657940850439431735, -44.10000000002499831 ) ) ;
#23756 = CARTESIAN_POINT ( 'NONE',  ( 4.180014548479816128, -1.737364395512316362, -18.80872516810000405 ) ) ;
#23757 = CARTESIAN_POINT ( 'NONE',  ( 19.80538173169999894, 19.50875421069999760, 226.9999998930000231 ) ) ;
#23758 = CARTESIAN_POINT ( 'NONE',  ( 0.000000000000000000, 0.000000000000000000, 230.8412452699534470 ) ) ;
#23759 = EDGE_CURVE ( 'NONE', #25602, #28085, #5288, .T. ) ;
#23760 = CARTESIAN_POINT ( 'NONE',  ( -24.55564696219999732, -13.03410599059999875, 224.4928762930000232 ) ) ;
#23761 = DIRECTION ( 'NONE',  ( 0.000000000000000000, 0.000000000000000000, 1.000000000000000000 ) ) ;
#23762 = CARTESIAN_POINT ( 'NONE',  ( -19.90432701819680972, 19.99999991336795802, 0.04921632800000685926 ) ) ;
#23763 = CARTESIAN_POINT ( 'NONE',  ( 7.908785388650001025, 16.35326433119999834, 231.6999999999999886 ) ) ;
#23764 = EDGE_CURVE ( 'NONE', #7351, #9833, #12364, .T. ) ;
#23765 = DIRECTION ( 'NONE',  ( -1.000000000000000000, 5.687697913155423197E-16, -6.771501495041734442E-12 ) ) ;
#23766 = CARTESIAN_POINT ( 'NONE',  ( -10.69999999989999928, -25.00000000000000000, -4.837481085799996805 ) ) ;
#23767 = ADVANCED_FACE ( 'NONE', ( #29353 ), #14777, .F. ) ;
#23768 = CARTESIAN_POINT ( 'NONE',  ( -3.686970300939999667, -0.1862064327014488485, -68.94610314789107974 ) ) ;
#23769 = ORIENTED_EDGE ( 'NONE', *, *, #17676, .T. ) ;
#23770 = CARTESIAN_POINT ( 'NONE',  ( 5.414213562369999622, -31.28896728272270877, -80.26658230080884948 ) ) ;
#23771 = CARTESIAN_POINT ( 'NONE',  ( 10.91239719759999893, 19.99999999999999645, -1.779565482400005560 ) ) ;
#23772 = CARTESIAN_POINT ( 'NONE',  ( 14.54659216921188936, -26.54260447311150628, -33.90912748487277639 ) ) ;
#23773 = EDGE_LOOP ( 'NONE', ( #562, #18725, #30850, #13857 ) ) ;
#23774 = CARTESIAN_POINT ( 'NONE',  ( -10.00000000045946713, -129.7569854617604506, -38.71642352146631794 ) ) ;
#23775 = EDGE_LOOP ( 'NONE', ( #20587, #13752, #18015, #6967 ) ) ;
#23776 = ORIENTED_EDGE ( 'NONE', *, *, #24892, .T. ) ;
#23777 = DIRECTION ( 'NONE',  ( 0.000000000000000000, 0.000000000000000000, 1.000000000000000000 ) ) ;
#23778 = ORIENTED_EDGE ( 'NONE', *, *, #6445, .T. ) ;
#23779 = CARTESIAN_POINT ( 'NONE',  ( 3.550686847520000117E-05, -28.50022181210000127, 223.9000014189999774 ) ) ;
#23780 = ORIENTED_EDGE ( 'NONE', *, *, #25043, .T. ) ;
#23781 = VECTOR ( 'NONE', #18985, 1000.000000000000000 ) ;
#23782 = CARTESIAN_POINT ( 'NONE',  ( 23.50666810109999716, -14.84174128299999929, 225.1041867410000350 ) ) ;
#23783 = CARTESIAN_POINT ( 'NONE',  ( 23.81776757409229361, 15.65134803726813217, 4.999998581000003384 ) ) ;
#23784 = CARTESIAN_POINT ( 'NONE',  ( 1.210976328703774474, 4.719380953081087959, -35.69999999999999574 ) ) ;
#23785 = CARTESIAN_POINT ( 'NONE',  ( 17.95841148951064525, -9.763538383420391042, -0.6999999999999784173 ) ) ;
#23786 = CARTESIAN_POINT ( 'NONE',  ( 14.56063207224778289, -22.00000000000000355, -30.73714836706114895 ) ) ;
#23787 = DIRECTION ( 'NONE',  ( 0.000000000000000000, -1.000000000000000000, 0.000000000000000000 ) ) ;
#23788 = CARTESIAN_POINT ( 'NONE',  ( -20.25360388639999698, 20.00000774629999611, 229.3817167830000017 ) ) ;
#23789 = EDGE_CURVE ( 'NONE', #17696, #15285, #28096, .T. ) ;
#23790 = CARTESIAN_POINT ( 'NONE',  ( -2.150134890876696847, -3.785840986416655340, -6.685065142700001850 ) ) ;
#23791 = CARTESIAN_POINT ( 'NONE',  ( 3.430850994441077439, -5.010772104901466406, -27.13292313650000764 ) ) ;
#23792 = DIRECTION ( 'NONE',  ( 0.7071067811865475727, -0.7071067811865475727, 0.000000000000000000 ) ) ;
#23793 = CARTESIAN_POINT ( 'NONE',  ( 10.45000000009999930, -29.92682926828999967, -28.39999999990001811 ) ) ;
#23794 = CIRCLE ( 'NONE', #26379, 2.999999999999999556 ) ;
#23795 = CARTESIAN_POINT ( 'NONE',  ( 24.36130769279719033, 13.39283555502935208, 5.208359080000030339 ) ) ;
#23796 = CARTESIAN_POINT ( 'NONE',  ( -25.35557883284624481, 13.01417685709828831, 5.679894689235580607 ) ) ;
#23797 = CARTESIAN_POINT ( 'NONE',  ( -3.679974273075529823, -2.251605409995534490, -21.90799200640000777 ) ) ;
#23798 = AXIS2_PLACEMENT_3D ( 'NONE', #30044, #17614, #5818 ) ;
#23799 = PRODUCT_DEFINITION_SHAPE ( 'NONE', 'NONE',  #31141 ) ;
#23800 = CARTESIAN_POINT ( 'NONE',  ( -10.99999999969999998, 21.69999999919999212, -70.09999999999999432 ) ) ;
#23801 = CARTESIAN_POINT ( 'NONE',  ( 0.000000000000000000, 0.000000000000000000, 40.00000000000000000 ) ) ;
#23802 = CARTESIAN_POINT ( 'NONE',  ( -20.44987259205819896, -17.46217831278680421, -1.399999999999998579 ) ) ;
#23803 = VERTEX_POINT ( 'NONE', #10328 ) ;
#23804 = VECTOR ( 'NONE', #30990, 1000.000000000000000 ) ;
#23805 = ORIENTED_EDGE ( 'NONE', *, *, #17096, .F. ) ;
#23806 = CARTESIAN_POINT ( 'NONE',  ( 0.000000000000000000, -50.49316738903675628, -63.39999999999999858 ) ) ;
#23807 = CARTESIAN_POINT ( 'NONE',  ( -1.776062861149290062E-14, -3.231615895114969171E-16, -0.5999999999999894307 ) ) ;
#23808 = EDGE_LOOP ( 'NONE', ( #28996, #19629, #28174, #25936 ) ) ;
#23809 = B_SPLINE_CURVE_WITH_KNOTS ( 'NONE', 5,
 ( #1984, #9197, #20544, #13621, #3702, #1355, #8569, #10949, #25589 ),
 .UNSPECIFIED., .F., .F.,
 ( 6, 3, 6 ),
 ( 0.000000000000000000, 18.06409709749999948, 31.46353197719999883 ),
 .UNSPECIFIED. ) ;
#23810 = CARTESIAN_POINT ( 'NONE',  ( 25.22625794089999829, -13.26224522399999906, 225.1041818340000020 ) ) ;
#23811 = DIRECTION ( 'NONE',  ( 3.112440860597585673E-12, 0.3322662713817149949, -0.9431856258987901809 ) ) ;
#23812 = ORIENTED_EDGE ( 'NONE', *, *, #446, .F. ) ;
#23813 = VERTEX_POINT ( 'NONE', #24488 ) ;
#23814 = ORIENTED_EDGE ( 'NONE', *, *, #28875, .T. ) ;
#23815 = ORIENTED_EDGE ( 'NONE', *, *, #30470, .T. ) ;
#23816 = CARTESIAN_POINT ( 'NONE',  ( 26.93395403039999891, -3.298349123909999533E-15, 37.75675929319999824 ) ) ;
#23817 = CARTESIAN_POINT ( 'NONE',  ( 28.49999999959999641, 10.47094317839999889, 229.0000000000000000 ) ) ;
#23818 = EDGE_CURVE ( 'NONE', #16560, #13298, #19067, .T. ) ;
#23820 = CARTESIAN_POINT ( 'NONE',  ( 18.26639035967037827, -8.979988381807324060, -1.000005633855494125E-09 ) ) ;
#23819 = VECTOR ( 'NONE', #30212, 1000.000000000000000 ) ;
#23821 = AXIS2_PLACEMENT_3D ( 'NONE', #26726, #155, #4710 ) ;
#23822 = ORIENTED_EDGE ( 'NONE', *, *, #13915, .T. ) ;
#23823 = EDGE_CURVE ( 'NONE', #23079, #9796, #17087, .T. ) ;
#23824 = CYLINDRICAL_SURFACE ( 'NONE', #17424, 3.000000000000003997 ) ;
#23825 = VECTOR ( 'NONE', #28863, 1000.000000000000000 ) ;
#23826 = CARTESIAN_POINT ( 'NONE',  ( 24.21598885539167867, -13.65447905993845978, 226.0728589708802474 ) ) ;
#23827 = CARTESIAN_POINT ( 'NONE',  ( 3.820026707160000257, -27.79243965350000067, 222.0000000000000000 ) ) ;
#23828 = CARTESIAN_POINT ( 'NONE',  ( 0.6686231747779999290, -28.49266848160000265, 225.9009072510000067 ) ) ;
#23829 = VERTEX_POINT ( 'NONE', #17238 ) ;
#23830 = EDGE_CURVE ( 'NONE', #30177, #16921, #435, .T. ) ;
#23831 = CARTESIAN_POINT ( 'NONE',  ( -20.89763770104046259, 16.92004971534728597, -1.399999999999998579 ) ) ;
#23832 = CARTESIAN_POINT ( 'NONE',  ( 2.558869066659682723, 3.716983018758990287, -16.27509163649999735 ) ) ;
#23833 = CARTESIAN_POINT ( 'NONE',  ( 0.000000000000000000, 0.000000000000000000, 226.6412452707750163 ) ) ;
#23834 = ORIENTED_EDGE ( 'NONE', *, *, #21668, .T. ) ;
#23835 = CYLINDRICAL_SURFACE ( 'NONE', #19735, 2.000000000000000000 ) ;
#23836 = CARTESIAN_POINT ( 'NONE',  ( 1.645560275461343203, -28.45273235261698019, 4.895940783000013674 ) ) ;
#23837 = CARTESIAN_POINT ( 'NONE',  ( 16.04674922903581091, 10.97998838177520931, 0.05106179917585291356 ) ) ;
#23838 = CARTESIAN_POINT ( 'NONE',  ( 11.62710820729999917, -24.17108566339999953, -1.401657795999995626 ) ) ;
#23839 = CARTESIAN_POINT ( 'NONE',  ( -12.30800288698999978, -29.39779533043000015, -32.78913491261000246 ) ) ;
#23840 = CARTESIAN_POINT ( 'NONE',  ( 24.36724931188768650, 13.38201648792073684, 4.999998581000003384 ) ) ;
#23841 = CARTESIAN_POINT ( 'NONE',  ( 16.06675444873834380, 10.97998838177521286, -0.6999999999999784173 ) ) ;
#23842 = CIRCLE ( 'NONE', #14289, 3.500000000000000888 ) ;
#23843 = ORIENTED_EDGE ( 'NONE', *, *, #3854, .F. ) ;
#23844 = EDGE_CURVE ( 'NONE', #4605, #17290, #12518, .T. ) ;
#23845 = CARTESIAN_POINT ( 'NONE',  ( 27.79999999999999716, 2.355804440410000085E-11, 229.0000000000000000 ) ) ;
#23846 = CARTESIAN_POINT ( 'NONE',  ( 8.699999999567717524, -16.96959321761985606, -37.81493174582519146 ) ) ;
#23847 = VECTOR ( 'NONE', #18371, 1000.000000000000000 ) ;
#23848 = CIRCLE ( 'NONE', #6237, 2.000000000000000000 ) ;
#23849 = AXIS2_PLACEMENT_3D ( 'NONE', #580, #12203, #29342 ) ;
#23850 = CARTESIAN_POINT ( 'NONE',  ( 0.000000000000000000, 0.000000000000000000, 115.0000000000000000 ) ) ;
#23851 = CARTESIAN_POINT ( 'NONE',  ( -9.000000000000000000, -130.0000000000000000, -42.39999999999999858 ) ) ;
#23852 = EDGE_CURVE ( 'NONE', #19721, #1607, #587, .T. ) ;
#23853 = CARTESIAN_POINT ( 'NONE',  ( 24.31679662959999888, 11.82640008669999965, 230.6999999999999886 ) ) ;
#23854 = ORIENTED_EDGE ( 'NONE', *, *, #7021, .F. ) ;
#23855 = PLANE ( 'NONE',  #11949 ) ;
#23856 = CARTESIAN_POINT ( 'NONE',  ( -4.617404660156336327, 1.522451704138575668, -69.49019511502498858 ) ) ;
#23857 = VERTEX_POINT ( 'NONE', #15049 ) ;
#23858 = ORIENTED_EDGE ( 'NONE', *, *, #19773, .T. ) ;
#23859 = CARTESIAN_POINT ( 'NONE',  ( 24.58642410257749233, -12.97641166413832714, 4.035859796549723377 ) ) ;
#23860 = CARTESIAN_POINT ( 'NONE',  ( 1.321824945545745145, 4.319062652178982553, -51.46125421262499344 ) ) ;
#23861 = ORIENTED_EDGE ( 'NONE', *, *, #5405, .T. ) ;
#23863 = CARTESIAN_POINT ( 'NONE',  ( 1.484924240490000047, 1.484924240490000047, 227.6412452697800006 ) ) ;
#23862 = CONICAL_SURFACE ( 'NONE', #9765, 2.500000000105231823, 0.7853981633974348453 ) ;
#23864 = CARTESIAN_POINT ( 'NONE',  ( -10.69999999999999929, -27.00000000000000000, -25.39999999999999858 ) ) ;
#23865 = EDGE_CURVE ( 'NONE', #27171, #1470, #9857, .T. ) ;
#23866 = CIRCLE ( 'NONE', #4250, 18.00000000000000000 ) ;
#23867 = AXIS2_PLACEMENT_3D ( 'NONE', #8249, #6211, #25103 ) ;
#23868 = B_SPLINE_CURVE_WITH_KNOTS ( 'NONE', 3,
 ( #4361, #13964, #11598, #21196, #7791, #880, #24328, #22275, #21974, #14732, #29042, #10324, #14892, #17392, #15044, #429, #12514, #8092 ),
 .UNSPECIFIED., .F., .F.,
 ( 4, 2, 2, 2, 2, 2, 2, 2, 4 ),
 ( 0.000000000000000000, 0.1249999999999999722, 0.2499999999999999445, 0.3749999999999998890, 0.4999999999999998890, 0.6249999999999998890, 0.7499999999999997780, 0.8749999999999998890, 1.000000000000000000 ),
 .UNSPECIFIED. ) ;
#23869 = CARTESIAN_POINT ( 'NONE',  ( 8.700000000296048697, -11.00364569656339775, -37.83911830543074473 ) ) ;
#23870 = B_SPLINE_CURVE_WITH_KNOTS ( 'NONE', 5,
 ( #11643, #14161, #6450, #25968, #28165, #21242 ),
 .UNSPECIFIED., .F., .F.,
 ( 6, 6 ),
 ( -2.300779717630000221, 0.000000000000000000 ),
 .UNSPECIFIED. ) ;
#23871 = CARTESIAN_POINT ( 'NONE',  ( -19.29999999990000248, -26.99999999999986144, -28.39999999990009272 ) ) ;
#23872 = CARTESIAN_POINT ( 'NONE',  ( 8.700000000241731257, -29.44972865398396067, -30.17591950688898095 ) ) ;
#23873 = VERTEX_POINT ( 'NONE', #19612 ) ;
#23874 = FACE_OUTER_BOUND ( 'NONE', #24132, .T. ) ;
#23875 = CARTESIAN_POINT ( 'NONE',  ( 0.8355090511298449707, -26.78702287612135891, 225.7193154187195603 ) ) ;
#23876 = CARTESIAN_POINT ( 'NONE',  ( 0.3105039177659999483, 12.06370740949999920, 231.9999989789999972 ) ) ;
#23877 = CARTESIAN_POINT ( 'NONE',  ( -19.80526803549999926, 19.50877411510000314, 227.5999999999999943 ) ) ;
#23878 = LINE ( 'NONE', #2468, #18685 ) ;
#23879 = CARTESIAN_POINT ( 'NONE',  ( -8.349999999348669988, -5.981227587280896429, -27.94042817487314423 ) ) ;
#23880 =( REPRESENTATION_RELATIONSHIP ('NONE','NONE', #2712, #19621 ) REPRESENTATION_RELATIONSHIP_WITH_TRANSFORMATION ( #4994 )SHAPE_REPRESENTATION_RELATIONSHIP( ) );
#23881 = CARTESIAN_POINT ( 'NONE',  ( -4.084346732781016343, 0.2146938849550972250, -40.92168819636143695 ) ) ;
#23882 = AXIS2_PLACEMENT_3D ( 'NONE', #3722, #13319, #10966 ) ;
#23883 = EDGE_CURVE ( 'NONE', #16796, #8103, #29596, .T. ) ;
#23884 = CARTESIAN_POINT ( 'NONE',  ( -24.63375100851393640, 12.88633854783081922, 4.098596794000014754 ) ) ;
#23885 = CARTESIAN_POINT ( 'NONE',  ( 1.599333684796361066, 1.229093439949829003, 227.6412452701079019 ) ) ;
#23886 = EDGE_CURVE ( 'NONE', #4374, #10417, #1069, .T. ) ;
#23887 = EDGE_CURVE ( 'NONE', #29453, #5618, #27452, .T. ) ;
#23888 = CARTESIAN_POINT ( 'NONE',  ( -23.88846875299723393, -13.62395840478711762, 6.099999999630012937 ) ) ;
#23889 = LINE ( 'NONE', #7189, #13813 ) ;
#23890 = CYLINDRICAL_SURFACE ( 'NONE', #3744, 2.000000000000003553 ) ;
#23891 = ORIENTED_EDGE ( 'NONE', *, *, #19416, .T. ) ;
#23892 = VECTOR ( 'NONE', #22446, 1000.000000000000000 ) ;
#23893 = CARTESIAN_POINT ( 'NONE',  ( 20.30396079662882158, 20.00000000004802203, 1.000000000000000888 ) ) ;
#23894 = EDGE_CURVE ( 'NONE', #18133, #23236, #29971, .T. ) ;
#23895 = EDGE_LOOP ( 'NONE', ( #27869, #11143, #18888, #28013 ) ) ;
#23896 = CARTESIAN_POINT ( 'NONE',  ( 4.198532171030673332, 1.238783022246746413, -35.53159726780000227 ) ) ;
#23897 = CARTESIAN_POINT ( 'NONE',  ( -4.499599993570057244, -1.182519567789861004, -57.20102360502500005 ) ) ;
#23898 = VERTEX_POINT ( 'NONE', #8097 ) ;
#23899 = CONTEXT_DEPENDENT_SHAPE_REPRESENTATION ( #15215, #10423 ) ;
#23900 = B_SPLINE_CURVE_WITH_KNOTS ( 'NONE', 5,
 ( #11170, #11331, #13368, #3935, #18403, #6293 ),
 .UNSPECIFIED., .F., .F.,
 ( 6, 6 ),
 ( 76.73731126729998664, 94.75474465359999954 ),
 .UNSPECIFIED. ) ;
#23901 = VERTEX_POINT ( 'NONE', #29813 ) ;
#23903 = EDGE_CURVE ( 'NONE', #29525, #1709, #20695, .T. ) ;
#23902 = CARTESIAN_POINT ( 'NONE',  ( -28.50000000000000000, -5.684341886079999373E-14, 229.0000000000000000 ) ) ;
#23904 = ORIENTED_EDGE ( 'NONE', *, *, #14092, .F. ) ;
#23905 = VECTOR ( 'NONE', #227, 1000.000000000000000 ) ;
#23906 =( NAMED_UNIT ( * ) PLANE_ANGLE_UNIT ( ) SI_UNIT ( $, .RADIAN. ) );
#23907 = CARTESIAN_POINT ( 'NONE',  ( -8.699999999643161175, -12.00129099599161897, -38.75807114290937250 ) ) ;
#23908 = CARTESIAN_POINT ( 'NONE',  ( 9.439621097969999042, 19.99999999999999645, -43.30705920210200333 ) ) ;
#23909 = CARTESIAN_POINT ( 'NONE',  ( 1.605176535610508326, -27.75389821387976852, 4.999998581000003384 ) ) ;
#23910 = CARTESIAN_POINT ( 'NONE',  ( -27.79539923781770128, -0.5057481688779184026, 8.000000000000007105 ) ) ;
#23911 = DIRECTION ( 'NONE',  ( 1.000000000000000000, -5.551115123130002122E-16, 0.000000000000000000 ) ) ;
#23912 = CARTESIAN_POINT ( 'NONE',  ( 2.521631941452523229, 3.946033397249450125, -5.200967428500000267 ) ) ;
#23913 = CARTESIAN_POINT ( 'NONE',  ( -28.45771199689999875, -10.45540640809999999, 229.4982322489999831 ) ) ;
#23914 = VERTEX_POINT ( 'NONE', #11101 ) ;
#23915 = CARTESIAN_POINT ( 'NONE',  ( -24.11911872370000154, -15.18353100999999938, 224.6893563800000209 ) ) ;
#23916 = ADVANCED_FACE ( 'NONE', ( #8401 ), #3537, .F. ) ;
#23917 = CARTESIAN_POINT ( 'NONE',  ( 4.790228392454985773, 0.1193559191107074896, -21.61411200059999871 ) ) ;
#23918 = CARTESIAN_POINT ( 'NONE',  ( -27.79999999999999716, -2.355663498000000066E-11, 223.3999999999999773 ) ) ;
#23919 = CARTESIAN_POINT ( 'NONE',  ( -10.32522729140000095, -25.00000000000000000, -1.399999999999998579 ) ) ;
#23920 = CARTESIAN_POINT ( 'NONE',  ( -8.341448913149999811, -8.801865131599999614, 230.6412452697800006 ) ) ;
#23921 = CARTESIAN_POINT ( 'NONE',  ( 11.69999999989999928, -2.500000000000002220, -2.399999999999999467 ) ) ;
#23922 = CARTESIAN_POINT ( 'NONE',  ( -19.65670002335123812, 20.00000013293643875, -0.1824558819999988479 ) ) ;
#23923 = DIRECTION ( 'NONE',  ( -3.133604487004501508E-12, -0.3568421334038989756, 0.9341647027306019258 ) ) ;
#23924 = CARTESIAN_POINT ( 'NONE',  ( 8.000000000276081380, -16.84112630282697154, -33.19732204816383359 ) ) ;
#23925 = CARTESIAN_POINT ( 'NONE',  ( 8.699999999959866059, -117.3672015275926697, 16.33620430255450628 ) ) ;
#23926 = CARTESIAN_POINT ( 'NONE',  ( -26.80000000000000071, 9.769962616700000205E-15, 36.78285841159999592 ) ) ;
#23927 = ORIENTED_EDGE ( 'NONE', *, *, #15574, .F. ) ;
#23928 = CARTESIAN_POINT ( 'NONE',  ( 6.252427222934309192, -16.79754308524862694, -74.99213524079873139 ) ) ;
#23929 = FACE_OUTER_BOUND ( 'NONE', #5284, .T. ) ;
#23930 = PLANE ( 'NONE',  #15197 ) ;
#23931 = ORIENTED_EDGE ( 'NONE', *, *, #1982, .F. ) ;
#23932 = DIRECTION ( 'NONE',  ( 1.000000000000000000, 5.998481157687279274E-24, -2.257150022441830001E-12 ) ) ;
#23933 = CARTESIAN_POINT ( 'NONE',  ( -0.6222386373588042474, 5.469632259241050676, -49.06410749632500057 ) ) ;
#23934 = VERTEX_POINT ( 'NONE', #17689 ) ;
#23935 = ORIENTED_EDGE ( 'NONE', *, *, #20743, .F. ) ;
#23936 = SURFACE_SIDE_STYLE ('',( #7241 ) ) ;
#23937 = ORIENTED_EDGE ( 'NONE', *, *, #30240, .F. ) ;
#23938 = DIRECTION ( 'NONE',  ( -1.000000000000000000, 0.000000000000000000, 0.000000000000000000 ) ) ;
#23939 = EDGE_CURVE ( 'NONE', #23813, #3101, #10825, .T. ) ;
#23940 = ORIENTED_EDGE ( 'NONE', *, *, #23099, .T. ) ;
#23941 = CARTESIAN_POINT ( 'NONE',  ( 23.56533302370000271, -14.74861233630000079, 225.5069924249999929 ) ) ;
#23942 = CARTESIAN_POINT ( 'NONE',  ( 2.871635305848139641, 2.026181749456782200, 227.6510696331277472 ) ) ;
#23943 = CARTESIAN_POINT ( 'NONE',  ( -14.89999999913999851, -32.00000000000000000, -31.28675134683000536 ) ) ;
#23944 = CARTESIAN_POINT ( 'NONE',  ( 0.5582180380177076406, 4.216789577812869005, -35.70000000000000284 ) ) ;
#23945 = EDGE_CURVE ( 'NONE', #8194, #9526, #27768, .T. ) ;
#23946 = EDGE_CURVE ( 'NONE', #9708, #13263, #30866, .T. ) ;
#23947 = CARTESIAN_POINT ( 'NONE',  ( 18.02647417827482812, 19.99991602546214153, -0.6955594401470849286 ) ) ;
#23948 = ADVANCED_FACE ( 'NONE', ( #5746 ), #27610, .F. ) ;
#23949 = CARTESIAN_POINT ( 'NONE',  ( -2.823270949701056409, -2.499023824075683020, -0.6999999999999992895 ) ) ;
#23950 = DIRECTION ( 'NONE',  ( 0.6941258031311203780, 0.7198537139083029945, 0.000000000000000000 ) ) ;
#23951 = CARTESIAN_POINT ( 'NONE',  ( -8.999999999970000886, 20.99999999999999645, -45.10000000000000142 ) ) ;
#23952 = ORIENTED_EDGE ( 'NONE', *, *, #19604, .F. ) ;
#23953 = CARTESIAN_POINT ( 'NONE',  ( 0.1708583496781435063, 4.358252033550405358, -7.937690181100000686 ) ) ;
#23954 = CARTESIAN_POINT ( 'NONE',  ( 4.370697773661016861, 1.580342671372844787, -26.51249766020000109 ) ) ;
#23955 = CARTESIAN_POINT ( 'NONE',  ( -8.699999999785086757, -66.94093258035375982, -17.28188441703444411 ) ) ;
#23956 = DIRECTION ( 'NONE',  ( -0.9998345049574558496, -0.01819238017630799703, 0.000000000000000000 ) ) ;
#23957 = CARTESIAN_POINT ( 'NONE',  ( 1.841797396446237967, -26.73663745407121795, 20.00000000000000355 ) ) ;
#23958 =( NAMED_UNIT ( * ) PLANE_ANGLE_UNIT ( ) SI_UNIT ( $, .RADIAN. ) );
#23959 = CARTESIAN_POINT ( 'NONE',  ( -3.885731905334990799, 2.027028853511393613, -1.418764356299999418 ) ) ;
#23960 = CARTESIAN_POINT ( 'NONE',  ( 17.33810066013692719, 9.903956624692348498, -1.400000000000001910 ) ) ;
#23961 = DIRECTION ( 'NONE',  ( -1.000000000000000000, 0.000000000000000000, 0.000000000000000000 ) ) ;
#23962 = CARTESIAN_POINT ( 'NONE',  ( -1.158394559326821005, -3.499774879700301433, 230.7286668686161306 ) ) ;
#23963 = VERTEX_POINT ( 'NONE', #20380 ) ;
#23964 = CARTESIAN_POINT ( 'NONE',  ( -8.700000000030557956, -116.5561065468281186, 18.74526241736806043 ) ) ;
#23965 = LINE ( 'NONE', #7573, #4267 ) ;
#23966 = ORIENTED_EDGE ( 'NONE', *, *, #18238, .T. ) ;
#23967 = CARTESIAN_POINT ( 'NONE',  ( 24.91921101730000032, -13.83103916669999833, 226.0027513979999867 ) ) ;
#23968 = CARTESIAN_POINT ( 'NONE',  ( 20.30405756109999871, 20.00000000820000068, 226.9999998930000231 ) ) ;
#23969 = VERTEX_POINT ( 'NONE', #6212 ) ;
#23970 = ORIENTED_EDGE ( 'NONE', *, *, #8642, .F. ) ;
#23971 = ORIENTED_EDGE ( 'NONE', *, *, #24110, .T. ) ;
#23972 = ORIENTED_EDGE ( 'NONE', *, *, #27821, .F. ) ;
#23973 = FACE_OUTER_BOUND ( 'NONE', #25665, .T. ) ;
#23974 = CARTESIAN_POINT ( 'NONE',  ( 27.29371452669260734, 0.4966198192113223664, -0.6577119969999878357 ) ) ;
#23975 = CARTESIAN_POINT ( 'NONE',  ( -7.999999999671499218, -17.87438019985146553, -33.91263442688144636 ) ) ;
#23976 = EDGE_LOOP ( 'NONE', ( #14983, #1247, #18624, #24503 ) ) ;
#23977 = DIRECTION ( 'NONE',  ( -1.000000000000000000, 0.000000000000000000, 0.000000000000000000 ) ) ;
#23978 = CARTESIAN_POINT ( 'NONE',  ( -0.1000000000582341592, -13.84939817494921321, -36.47165854350617309 ) ) ;
#23979 = EDGE_CURVE ( 'NONE', #7544, #13699, #15651, .T. ) ;
#23980 = CARTESIAN_POINT ( 'NONE',  ( 18.31101511981528773, 19.88193408480103486, 0.02162463700000616385 ) ) ;
#23981 = CARTESIAN_POINT ( 'NONE',  ( 11.20000000009999930, -27.00000000000000000, -28.39999999989999679 ) ) ;
#23982 = VERTEX_POINT ( 'NONE', #10784 ) ;
#23983 = CARTESIAN_POINT ( 'NONE',  ( -23.35903771415276609, 13.31654055986141572, -1.399999999999998357 ) ) ;
#23984 = AXIS2_PLACEMENT_3D ( 'NONE', #28719, #22260, #2906 ) ;
#23985 = CARTESIAN_POINT ( 'NONE',  ( 0.7420639427752478978, -6.011517603930927045, -17.77054674910000287 ) ) ;
#23986 = DIRECTION ( 'NONE',  ( -1.000000000000000000, 0.000000000000000000, 0.000000000000000000 ) ) ;
#23987 = B_SPLINE_CURVE_WITH_KNOTS ( 'NONE', 3,
 ( #13198, #20603, #12904, #18073, #22512, #20447 ),
 .UNSPECIFIED., .F., .F.,
 ( 4, 2, 4 ),
 ( 0.000000000000000000, 0.5000000000000000000, 1.000000000000000000 ),
 .UNSPECIFIED. ) ;
#23988 = CARTESIAN_POINT ( 'NONE',  ( 0.9245300016271229548, -27.48475604047800047, 5.597451638069735225 ) ) ;
#23989 = CIRCLE ( 'NONE', #7395, 5.999999999999996447 ) ;
#23990 = ORIENTED_EDGE ( 'NONE', *, *, #17346, .F. ) ;
#23991 = CARTESIAN_POINT ( 'NONE',  ( 8.000000000236575204, -29.80249033211431708, -29.47052495773638370 ) ) ;
#23992 = DIRECTION ( 'NONE',  ( 0.000000000000000000, -1.000000000000000000, 0.000000000000000000 ) ) ;
#23993 = CARTESIAN_POINT ( 'NONE',  ( 4.175165894169885483, -50.49316738903675628, -43.39999999999999858 ) ) ;
#23994 = FACE_OUTER_BOUND ( 'NONE', #2748, .T. ) ;
#23995 = DIRECTION ( 'NONE',  ( 0.3633921898465291567, 0.9316362575375349842, 1.850371707708594444E-14 ) ) ;
#23996 = CARTESIAN_POINT ( 'NONE',  ( 27.77512470430000135, -2.242274238020000225E-11, 229.2930777930000090 ) ) ;
#23997 = CARTESIAN_POINT ( 'NONE',  ( -17.50139837460000081, 5.282193806050000440, 230.6999999999999886 ) ) ;
#23998 = ORIENTED_EDGE ( 'NONE', *, *, #18493, .T. ) ;
#23999 = EDGE_CURVE ( 'NONE', #22441, #11915, #30720, .T. ) ;
#24000 = DIRECTION ( 'NONE',  ( 0.000000000000000000, 0.000000000000000000, -1.000000000000000000 ) ) ;
#24001 = CARTESIAN_POINT ( 'NONE',  ( -11.00000000000000000, 25.22617105830878614, -61.82510970417090590 ) ) ;
#24002 = CARTESIAN_POINT ( 'NONE',  ( -27.24406355354254217, -0.4957164003246626316, 0.08279779300002232389 ) ) ;
#24003 = CARTESIAN_POINT ( 'NONE',  ( -4.006504157561272983, -3.130081512437369984, -68.10000000002499121 ) ) ;
#24004 = VERTEX_POINT ( 'NONE', #13297 ) ;
#24005 = ADVANCED_FACE ( 'NONE', ( #3859 ), #15500, .T. ) ;
#24006 = CARTESIAN_POINT ( 'NONE',  ( 3.388043077353672494, 1.111846212962369629, -88.52261276243450538 ) ) ;
#24007 = VECTOR ( 'NONE', #14146, 999.9999999999998863 ) ;
#24008 = ORIENTED_EDGE ( 'NONE', *, *, #2794, .T. ) ;
#24009 = CARTESIAN_POINT ( 'NONE',  ( -24.32472894358752313, 13.45989150749028873, 3.899998581000013509 ) ) ;
#24010 = CARTESIAN_POINT ( 'NONE',  ( -0.8291470764733299692, -4.443337602648613327, -67.90745670422499813 ) ) ;
#24011 = ORIENTED_EDGE ( 'NONE', *, *, #11988, .T. ) ;
#24012 = CARTESIAN_POINT ( 'NONE',  ( -1.151230282303595587, -4.494053275198272246, -28.04882611460000064 ) ) ;
#24013 = LINE ( 'NONE', #26667, #5368 ) ;
#24014 = CARTESIAN_POINT ( 'NONE',  ( 4.009291712408949770, -2.091746824018178685, -61.31790713612500099 ) ) ;
#24015 = DIRECTION ( 'NONE',  ( 0.000000000000000000, -0.9128796883888953273, 0.4082287037029528332 ) ) ;
#24016 = CARTESIAN_POINT ( 'NONE',  ( -20.30403093138962234, 20.00000000003553424, 1.000000000000000888 ) ) ;
#24017 = CARTESIAN_POINT ( 'NONE',  ( -19.80535397421925481, 19.50875616500616871, 0.9999999989999952543 ) ) ;
#24018 = CARTESIAN_POINT ( 'NONE',  ( -7.999999999684019869, -16.03708229645564742, -33.01798262065937450 ) ) ;
#24019 = PLANE ( 'NONE',  #22063 ) ;
#24020 = EDGE_CURVE ( 'NONE', #8030, #13901, #23842, .T. ) ;
#24021 = ORIENTED_EDGE ( 'NONE', *, *, #14841, .F. ) ;
#24022 = CYLINDRICAL_SURFACE ( 'NONE', #17496, 3.500000000000003109 ) ;
#24023 = CARTESIAN_POINT ( 'NONE',  ( 3.900999017799251956, -2.591123067748548614, -35.07256796030007706 ) ) ;
#24024 = CARTESIAN_POINT ( 'NONE',  ( -10.37415685080000038, -6.597363088169999834, 232.6627643349999914 ) ) ;
#24025 = CARTESIAN_POINT ( 'NONE',  ( -27.79999999990000248, 4.328052761030000362, 227.5999999999999943 ) ) ;
#24026 = CARTESIAN_POINT ( 'NONE',  ( 22.97559295455008765, 15.65128684778802715, 8.000000000000007105 ) ) ;
#24027 = CARTESIAN_POINT ( 'NONE',  ( -8.699999999729206124, -25.09057560198417747, -26.05270539051472767 ) ) ;
#24028 = CARTESIAN_POINT ( 'NONE',  ( 24.21557264265764431, -13.65522559108275935, 223.9268223389925083 ) ) ;
#24029 = AXIS2_PLACEMENT_3D ( 'NONE', #28491, #4424, #26141 ) ;
#24030 = CARTESIAN_POINT ( 'NONE',  ( -25.45799949038170240, 12.81261085762170815, 4.791562840999991302 ) ) ;
#24031 = CARTESIAN_POINT ( 'NONE',  ( 17.16657240419154462, 10.99999999996915179, -0.6999999999999784173 ) ) ;
#24032 = CARTESIAN_POINT ( 'NONE',  ( -0.2766206855629021466, -12.09920926763397553, 232.0000002394077399 ) ) ;
#24033 = LINE ( 'NONE', #7498, #24370 ) ;
#24034 = CARTESIAN_POINT ( 'NONE',  ( 6.999999999945624829, -115.1185614904238577, 21.95989595801592031 ) ) ;
#24035 = ORIENTED_EDGE ( 'NONE', *, *, #11785, .T. ) ;
#24036 = ADVANCED_FACE ( 'NONE', ( #23066 ), #1509, .F. ) ;
#24037 = AXIS2_PLACEMENT_3D ( 'NONE', #14536, #2569, #24130 ) ;
#24038 = DIRECTION ( 'NONE',  ( 1.000000000000000000, -3.981000000000000101E-12, 1.940999999999999908E-12 ) ) ;
#24039 = SHAPE_REPRESENTATION ( 'Moving Handle', ( #17722 ), #9278 ) ;
#24040 = EDGE_LOOP ( 'NONE', ( #7651, #26941, #25512, #14986 ) ) ;
#24041 = CARTESIAN_POINT ( 'NONE',  ( 24.60092358069999818, -12.94742893949999818, 225.2083619149999834 ) ) ;
#24042 = CARTESIAN_POINT ( 'NONE',  ( 3.992508014903327407, 4.044424149039453908, -58.50805965152499510 ) ) ;
#24043 = ORIENTED_EDGE ( 'NONE', *, *, #23460, .T. ) ;
#24044 = CONTEXT_DEPENDENT_SHAPE_REPRESENTATION ( #13183, #31082 ) ;
#24045 = EDGE_LOOP ( 'NONE', ( #23307, #2155, #20163, #19517 ) ) ;
#24047 = CARTESIAN_POINT ( 'NONE',  ( -17.40937546595008101, -25.54985367907119453, -23.46373967705341457 ) ) ;
#24046 = VECTOR ( 'NONE', #20408, 1000.000000000000000 ) ;
#24048 = ORIENTED_EDGE ( 'NONE', *, *, #14444, .F. ) ;
#24049 = EDGE_CURVE ( 'NONE', #28478, #24307, #1730, .T. ) ;
#24050 = B_SPLINE_CURVE_WITH_KNOTS ( 'NONE', 3,
 ( #18307, #17979, #28214, #27590, #16255, #6351, #15629, #25875, #25239, #25404 ),
 .UNSPECIFIED., .F., .F.,
 ( 4, 2, 2, 2, 4 ),
 ( 0.000000000000000000, 0.2500000000000000000, 0.5000000000000000000, 0.7500000000000000000, 1.000000000000000000 ),
 .UNSPECIFIED. ) ;
#24051 = CARTESIAN_POINT ( 'NONE',  ( 2.086681040044585433, 0.2757844057790842518, 226.6412452697800290 ) ) ;
#24052 = CARTESIAN_POINT ( 'NONE',  ( -2.595987296770100095, -16.63200279373747392, -109.8342699011499946 ) ) ;
#24053 = CARTESIAN_POINT ( 'NONE',  ( -27.07233438391262226, 8.380005029826659069, 5.200000000000009948 ) ) ;
#24054 = EDGE_CURVE ( 'NONE', #28713, #28185, #2576, .T. ) ;
#24055 = CARTESIAN_POINT ( 'NONE',  ( 17.14121550692227558, 12.10909424797362455, -1.400000000000002132 ) ) ;
#24056 = CARTESIAN_POINT ( 'NONE',  ( -4.667733413567799694, -30.93201666733562405, 8.000000000000007105 ) ) ;
#24057 = CARTESIAN_POINT ( 'NONE',  ( -19.80535357377644701, 19.50875577052588739, 2.200000064000007249 ) ) ;
#24058 = CARTESIAN_POINT ( 'NONE',  ( 2.246931792404676997, -6.149078805876593279, -5.660585232200005201 ) ) ;
#24059 = CARTESIAN_POINT ( 'NONE',  ( 10.95000000009999930, -27.00000000000000000, -28.39999999989999679 ) ) ;
#24060 = VERTEX_POINT ( 'NONE', #31071 ) ;
#24061 = CARTESIAN_POINT ( 'NONE',  ( -1.728755095528217378, -4.797076482011579657, -44.10000000002499831 ) ) ;
#24062 = AXIS2_PLACEMENT_3D ( 'NONE', #20953, #14500, #13875 ) ;
#24063 = EDGE_CURVE ( 'NONE', #1319, #145, #22861, .T. ) ;
#24064 = CARTESIAN_POINT ( 'NONE',  ( -2.618143654921853969, 3.481518582925489991, -20.13064294429999990 ) ) ;
#24065 = DIRECTION ( 'NONE',  ( 0.2815395311429192970, 0.9595496299847263710, 0.000000000000000000 ) ) ;
#24066 = CARTESIAN_POINT ( 'NONE',  ( 24.78870453580057998, -12.58522324566301620, 5.507123706999989210 ) ) ;
#24067 = CARTESIAN_POINT ( 'NONE',  ( -11.69999999989999928, -25.00000000000000000, -2.399999999999999467 ) ) ;
#24068 = CARTESIAN_POINT ( 'NONE',  ( 20.50716141039999840, 18.79636021840000026, 225.9999999149999894 ) ) ;
#24069 = CARTESIAN_POINT ( 'NONE',  ( -19.36598219300702794, 19.99999980947656297, -0.3593759589999856452 ) ) ;
#24070 = CARTESIAN_POINT ( 'NONE',  ( 10.69999999999842366, -26.27037943368971540, -25.46729144948177748 ) ) ;
#24071 = DIRECTION ( 'NONE',  ( 0.3633921898465272138, -0.9316362575375356503, 0.000000000000000000 ) ) ;
#24072 = DIRECTION ( 'NONE',  ( -2.256992747040000044E-12, 0.000000000000000000, -1.000000000000000000 ) ) ;
#24074 = ADVANCED_FACE ( 'NONE', ( #13765 ), #8881, .T. ) ;
#24073 = VECTOR ( 'NONE', #11632, 999.9999999999998863 ) ;
#24075 = FACE_OUTER_BOUND ( 'NONE', #22560, .T. ) ;
#24076 = ORIENTED_EDGE ( 'NONE', *, *, #27582, .T. ) ;
#24077 = CARTESIAN_POINT ( 'NONE',  ( 4.420334067734101424, -4.199682076162645217, -30.05126389020000488 ) ) ;
#24078 = CARTESIAN_POINT ( 'NONE',  ( 1.776356839399999804E-15, 1.776356839399999804E-15, 229.6412452697800006 ) ) ;
#24079 = ORIENTED_EDGE ( 'NONE', *, *, #19281, .F. ) ;
#24080 = CARTESIAN_POINT ( 'NONE',  ( 9.999999999979998222, -27.00000000000000000, -31.39999999999999858 ) ) ;
#24081 = CARTESIAN_POINT ( 'NONE',  ( 2.137930486642451555, 6.059703978454344941, -45.97079303332500189 ) ) ;
#24082 = ORIENTED_EDGE ( 'NONE', *, *, #16916, .F. ) ;
#24083 = EDGE_CURVE ( 'NONE', #19165, #30573, #19316, .T. ) ;
#24084 = ORIENTED_EDGE ( 'NONE', *, *, #5934, .T. ) ;
#24085 = PRESENTATION_STYLE_ASSIGNMENT (( #16370 ) ) ;
#24086 = VERTEX_POINT ( 'NONE', #11716 ) ;
#24087 = CYLINDRICAL_SURFACE ( 'NONE', #24531, 8.000000000000000000 ) ;
#24088 = VERTEX_POINT ( 'NONE', #19110 ) ;
#24089 = CARTESIAN_POINT ( 'NONE',  ( 14.25032083441342934, -27.35421241409322946, 1.000000000000000888 ) ) ;
#24090 = CARTESIAN_POINT ( 'NONE',  ( 27.79539923781924315, 0.5057481687932959824, 8.000000000000007105 ) ) ;
#24091 = CARTESIAN_POINT ( 'NONE',  ( 0.7747757076663149833, 4.116528746048892629, -35.69999999999999574 ) ) ;
#24092 = VECTOR ( 'NONE', #20881, 1000.000000000000000 ) ;
#24093 = CARTESIAN_POINT ( 'NONE',  ( 18.56971040771836101, 20.00001258923172998, -0.6273519244159778685 ) ) ;
#24094 = CARTESIAN_POINT ( 'NONE',  ( -23.77947513073445407, 14.40125622634048774, 5.208432825000025801 ) ) ;
#24095 = CARTESIAN_POINT ( 'NONE',  ( -5.005341893651962693, -8.809215901958738826, -33.18262749602455841 ) ) ;
#24096 = AXIS2_PLACEMENT_3D ( 'NONE', #8347, #20016, #22388 ) ;
#24097 = CARTESIAN_POINT ( 'NONE',  ( 17.33054985591605757, -10.09719844076225215, -4.336808689942018722E-16 ) ) ;
#24098 = VERTEX_POINT ( 'NONE', #6679 ) ;
#24099 = CARTESIAN_POINT ( 'NONE',  ( 5.067327387632984959, 4.072231104569050686, -8.954586408000002606 ) ) ;
#24100 = CARTESIAN_POINT ( 'NONE',  ( -3.052438874386679046, 3.509528713898351970, -28.08728588870000209 ) ) ;
#24101 = CARTESIAN_POINT ( 'NONE',  ( 0.7153897335033406746, -3.455736562763356279, 0.000000000000000000 ) ) ;
#24102 = CARTESIAN_POINT ( 'NONE',  ( 8.699999999569731912, -15.05691612486679176, -37.86814428171000912 ) ) ;
#24103 = CARTESIAN_POINT ( 'NONE',  ( 24.41841038956698640, 14.69667349781389376, 6.099998581000020792 ) ) ;
#24104 = CARTESIAN_POINT ( 'NONE',  ( -23.48807013395677856, -14.30280389748388359, 225.9130852761126107 ) ) ;
#24105 = CARTESIAN_POINT ( 'NONE',  ( 6.112318018889860483, -26.81313817375426112, 21.03870473235707550 ) ) ;
#24106 = CARTESIAN_POINT ( 'NONE',  ( -1.831588579526997940, 3.958388136463042439, -7.731725184300007214 ) ) ;
#24107 = CARTESIAN_POINT ( 'NONE',  ( -9.993285220779545952, -25.61999708228220740, 193.6055512750000105 ) ) ;
#24108 = CARTESIAN_POINT ( 'NONE',  ( -24.22405393111852234, -13.63981656674930854, 4.239871886000001311 ) ) ;
#24109 = DIRECTION ( 'NONE',  ( 0.000000000000000000, 0.000000000000000000, -1.000000000000000000 ) ) ;
#24110 = EDGE_CURVE ( 'NONE', #29777, #24119, #28851, .T. ) ;
#24111 = VERTEX_POINT ( 'NONE', #13612 ) ;
#24112 = ADVANCED_FACE ( 'NONE', ( #26047, #14087 ), #13929, .F. ) ;
#24113 = LINE ( 'NONE', #12601, #4221 ) ;
#24114 = CARTESIAN_POINT ( 'NONE',  ( -12.30772508779320695, -31.99999999999999289, -28.84027805903673780 ) ) ;
#24115 = VECTOR ( 'NONE', #3801, 1000.000000000000000 ) ;
#24116 = VERTEX_POINT ( 'NONE', #11871 ) ;
#24117 = DIRECTION ( 'NONE',  ( 0.000000000000000000, 0.000000000000000000, 1.000000000000000000 ) ) ;
#24118 = CARTESIAN_POINT ( 'NONE',  ( 23.81776757409229361, 15.65134803726813217, 4.999998581000003384 ) ) ;
#24119 = VERTEX_POINT ( 'NONE', #23218 ) ;
#24120 = ORIENTED_EDGE ( 'NONE', *, *, #15461, .F. ) ;
#24121 = EDGE_LOOP ( 'NONE', ( #16263, #17631, #25598, #7277 ) ) ;
#24122 = EDGE_LOOP ( 'NONE', ( #9151, #9181, #5688, #7738 ) ) ;
#24123 = CARTESIAN_POINT ( 'NONE',  ( 10.00000000070000183, -27.00000000000000000, -25.39999999999999858 ) ) ;
#24124 = CARTESIAN_POINT ( 'NONE',  ( 23.69119887989999995, 20.94188554249999967, 222.0000000000000000 ) ) ;
#24125 = PLANE ( 'NONE',  #24796 ) ;
#24126 = ORIENTED_EDGE ( 'NONE', *, *, #7930, .T. ) ;
#24127 = CARTESIAN_POINT ( 'NONE',  ( -25.46368746804859740, 12.80129684245613575, 4.999998581000003384 ) ) ;
#24128 = CARTESIAN_POINT ( 'NONE',  ( 4.000000000000000000, -29.27600094726834712, -81.66227801707495360 ) ) ;
#24129 = CARTESIAN_POINT ( 'NONE',  ( -17.31586207618096651, -31.99964831253470621, -26.55600617737724534 ) ) ;
#24130 = DIRECTION ( 'NONE',  ( -0.7071067811865467956, 0.6644630243886068266, 0.2418447626481644297 ) ) ;
#24131 = CARTESIAN_POINT ( 'NONE',  ( 2.479820170275052860, -4.407201367387826529, -0.7000592809870032074 ) ) ;
#24132 = EDGE_LOOP ( 'NONE', ( #2670, #19005, #26641, #12218 ) ) ;
#24133 = CARTESIAN_POINT ( 'NONE',  ( -18.33647963386089685, 19.99999869789418128, -0.6670195793833753051 ) ) ;
#24134 = B_SPLINE_CURVE_WITH_KNOTS ( 'NONE', 4,
 ( #28146, #16185, #6432, #29879, #23129 ),
 .UNSPECIFIED., .F., .F.,
 ( 5, 5 ),
 ( -0.9817477042479999527, 0.9817477042479999527 ),
 .UNSPECIFIED. ) ;
#24135 = CARTESIAN_POINT ( 'NONE',  ( 4.130711734062741947, 1.221343755424970201, -17.04190840230000248 ) ) ;
#24136 = CARTESIAN_POINT ( 'NONE',  ( -7.999999999650188265, -15.90960369693041088, -38.05208140759208391 ) ) ;
#24137 = CARTESIAN_POINT ( 'NONE',  ( -2.962149026499999369E-14, -27.50000000069999828, 6.100000000000000533 ) ) ;
#24138 = DIRECTION ( 'NONE',  ( 0.3633921898465291567, 0.9316362575375348731, -0.000000000000000000 ) ) ;
#24139 = CARTESIAN_POINT ( 'NONE',  ( 23.51173842660000091, 14.86483492350000013, 222.0000000000000000 ) ) ;
#24140 = DIRECTION ( 'NONE',  ( -0.000000000000000000, 1.000000000000000000, -0.000000000000000000 ) ) ;
#24141 = CYLINDRICAL_SURFACE ( 'NONE', #29534, 1.099999999999999867 ) ;
#24142 = CARTESIAN_POINT ( 'NONE',  ( 10.00000000000000000, -13.98526668056139144, -73.96855033896248699 ) ) ;
#24143 = CARTESIAN_POINT ( 'NONE',  ( 26.80907646719999704, 9.389153233520001862, 229.0000000000000000 ) ) ;
#24144 = CARTESIAN_POINT ( 'NONE',  ( 10.00000000000000000, -13.98526668056139144, -73.96855033896248699 ) ) ;
#24145 = ORIENTED_EDGE ( 'NONE', *, *, #16155, .F. ) ;
#24146 = DIRECTION ( 'NONE',  ( 0.000000000000000000, 0.000000000000000000, 1.000000000000000000 ) ) ;
#24147 = ADVANCED_FACE ( 'NONE', ( #21317 ), #6529, .T. ) ;
#24148 = CARTESIAN_POINT ( 'NONE',  ( 2.402407292417764406, -4.152604782219900592, -68.10000000002501963 ) ) ;
#24149 = CARTESIAN_POINT ( 'NONE',  ( -4.505292919096236304, -2.281031367935008269, -68.10000000002500542 ) ) ;
#24150 = ADVANCED_FACE ( 'NONE', ( #16126 ), #4632, .F. ) ;
#24151 = ORIENTED_EDGE ( 'NONE', *, *, #9169, .F. ) ;
#24152 = CARTESIAN_POINT ( 'NONE',  ( 26.80000000000000071, -6.394884621839999216E-14, 230.6999999999999886 ) ) ;
#24153 =( NAMED_UNIT ( * ) PLANE_ANGLE_UNIT ( ) SI_UNIT ( $, .RADIAN. ) );
#24154 = ORIENTED_EDGE ( 'NONE', *, *, #18315, .T. ) ;
#24155 = DIRECTION ( 'NONE',  ( 1.000000000000000000, -9.219999999999999084E-13, 4.710999999999999616E-12 ) ) ;
#24156 = CARTESIAN_POINT ( 'NONE',  ( -3.200877993934844401, 3.183711413074225671, -69.34322600122500546 ) ) ;
#24157 = VERTEX_POINT ( 'NONE', #30460 ) ;
#24158 = CARTESIAN_POINT ( 'NONE',  ( -3.834000099192893973, 2.652495916366584439, -25.46779765530001072 ) ) ;
#24159 = CARTESIAN_POINT ( 'NONE',  ( -2.099999999790000960, -0.1392085008781404898, 226.6412452697799722 ) ) ;
#24160 = CARTESIAN_POINT ( 'NONE',  ( 4.883349601227576997, 0.1168011502185872796, -64.06686508972499894 ) ) ;
#24161 = DIRECTION ( 'NONE',  ( 0.000000000000000000, 0.000000000000000000, 1.000000000000000000 ) ) ;
#24162 = CARTESIAN_POINT ( 'NONE',  ( -23.81866173682177390, -14.33570044646243247, 3.899998581000013509 ) ) ;
#24163 = CYLINDRICAL_SURFACE ( 'NONE', #27806, 2.500000000000000888 ) ;
#24164 = UNCERTAINTY_MEASURE_WITH_UNIT (LENGTH_MEASURE( 1.000000000000000082E-05 ), #22994, 'distance_accuracy_value', 'NONE');
#24165 = CARTESIAN_POINT ( 'NONE',  ( 8.699999999551790708, -9.149979919791583427, -35.02638174844071983 ) ) ;
#24166 = CARTESIAN_POINT ( 'NONE',  ( -17.49266624248041779, -21.99978574281297483, -28.62488781290136686 ) ) ;
#24167 = ORIENTED_EDGE ( 'NONE', *, *, #15526, .F. ) ;
#24168 = CARTESIAN_POINT ( 'NONE',  ( -27.06563794070000029, 3.314475219249999806E-15, 191.9402686260000053 ) ) ;
#24169 = CARTESIAN_POINT ( 'NONE',  ( 8.700000000290671665, -15.69142432425455347, -38.04086644837175157 ) ) ;
#24170 = EDGE_CURVE ( 'NONE', #11464, #27319, #25085, .T. ) ;
#24171 = CARTESIAN_POINT ( 'NONE',  ( -11.74965333179999938, 3.618560759109999747, 232.6627643349999914 ) ) ;
#24172 = CARTESIAN_POINT ( 'NONE',  ( -19.80526803549999926, 19.50877411520000138, 224.8000000000000114 ) ) ;
#24173 = B_SPLINE_CURVE_WITH_KNOTS ( 'NONE', 3,
 ( #13046, #22653, #17753, #15712, #15410, #8158, #22504, #3767, #8314, #1258, #8470, #25009, #5962 ),
 .UNSPECIFIED., .F., .F.,
 ( 4, 2, 2, 1, 2, 2, 4 ),
 ( 0.000000000000000000, 0.2499999999999729661, 0.3749999999999577005, 0.4374999999999472644, 0.4687499999999453215, 0.4999999999999433786, 1.000000000000000000 ),
 .UNSPECIFIED. ) ;
#24174 = CYLINDRICAL_SURFACE ( 'NONE', #30741, 20.00000000000000711 ) ;
#24175 = CARTESIAN_POINT ( 'NONE',  ( 10.45000000009999930, -30.17682926828999967, -28.39999999989999679 ) ) ;
#24176 = CARTESIAN_POINT ( 'NONE',  ( 8.999999999540001738, 19.99999999999999645, -44.09999999970998630 ) ) ;
#24177 = CARTESIAN_POINT ( 'NONE',  ( 23.89355638714178198, 14.21126451599432272, 3.899998580999974873 ) ) ;
#24178 = CARTESIAN_POINT ( 'NONE',  ( -0.6479069133012533843, -26.79235980095155512, 225.9098122281707788 ) ) ;
#24179 = CARTESIAN_POINT ( 'NONE',  ( -24.73568147689076469, 12.68911064935910815, 4.319165764000016061 ) ) ;
#24180 = DIRECTION ( 'NONE',  ( -1.000000000000000000, 0.000000000000000000, 0.000000000000000000 ) ) ;
#24181 = VECTOR ( 'NONE', #21637, 1000.000000000000000 ) ;
#24182 = CARTESIAN_POINT ( 'NONE',  ( 9.999984944298805800, 21.69999999997726903, -54.17105275116254148 ) ) ;
#24183 = CARTESIAN_POINT ( 'NONE',  ( -16.14308042027219869, -8.142661250102314341, 0.000000000000000000 ) ) ;
#24184 = CARTESIAN_POINT ( 'NONE',  ( 7.439629836415988962, -115.1565018356284327, 21.87505388250205129 ) ) ;
#24185 = ADVANCED_BREP_SHAPE_REPRESENTATION ( '', ( #21218, #17722 ), #23393 ) ;
#24186 = VERTEX_POINT ( 'NONE', #2288 ) ;
#24187 = CARTESIAN_POINT ( 'NONE',  ( 19.80526555972147307, 19.50877392102524155, 3.000000000000002665 ) ) ;
#24188 = VERTEX_POINT ( 'NONE', #1977 ) ;
#24189 = FACE_OUTER_BOUND ( 'NONE', #31046, .T. ) ;
#24190 = CARTESIAN_POINT ( 'NONE',  ( 1.078097839695846494, -5.807694627614346849, -59.54125695792498618 ) ) ;
#24191 = EDGE_LOOP ( 'NONE', ( #26906, #28047 ) ) ;
#24192 = EDGE_LOOP ( 'NONE', ( #1807, #18792, #30887, #12257 ) ) ;
#24193 = DIRECTION ( 'NONE',  ( -0.9316362575375349842, 0.3633921898465292122, -0.000000000000000000 ) ) ;
#24194 = ORIENTED_EDGE ( 'NONE', *, *, #3586, .T. ) ;
#24195 = EDGE_LOOP ( 'NONE', ( #8457, #15358, #21956, #2368 ) ) ;
#24196 =( LENGTH_UNIT ( ) NAMED_UNIT ( * ) SI_UNIT ( .MILLI., .METRE. ) );
#24197 = CARTESIAN_POINT ( 'NONE',  ( -16.52704821365513510, -10.06576768835640046, -0.6999999999999785283 ) ) ;
#24198 = ADVANCED_FACE ( 'NONE', ( #11568 ), #5250, .T. ) ;
#24199 = COLOUR_RGB ( '', 0.31764706, 0.68627451, 0.89019608) ;
#24200 = CARTESIAN_POINT ( 'NONE',  ( 9.657736559230000850, -7.680833809369999265, 232.6627648150000027 ) ) ;
#24201 = LINE ( 'NONE', #28758, #30539 ) ;
#24202 = CARTESIAN_POINT ( 'NONE',  ( 1.765446408317208560, -4.831419061753667421, -5.323085232199998629 ) ) ;
#24203 = FACE_OUTER_BOUND ( 'NONE', #25359, .T. ) ;
#24204 = VERTEX_POINT ( 'NONE', #4943 ) ;
#24205 = CARTESIAN_POINT ( 'NONE',  ( 13.15714562406650501, 20.99999999997228528, -56.37888616265984609 ) ) ;
#24206 = DIRECTION ( 'NONE',  ( 1.000000000000000000, 0.000000000000000000, 0.000000000000000000 ) ) ;
#24207 = EDGE_CURVE ( 'NONE', #10804, #5944, #29197, .T. ) ;
#24208 = CARTESIAN_POINT ( 'NONE',  ( 3.800013225884300905, -1.579422177728472487, -18.37122516810000050 ) ) ;
#24209 = CARTESIAN_POINT ( 'NONE',  ( -1.549220603335524693, 3.500000000000000000, 230.6508329224841987 ) ) ;
#24210 = LINE ( 'NONE', #26720, #17517 ) ;
#24211 = CARTESIAN_POINT ( 'NONE',  ( -24.58975347950000057, -12.96948186770000078, 224.6893543200000067 ) ) ;
#24212 = CARTESIAN_POINT ( 'NONE',  ( -15.96459051030187126, 11.69027953513920437, -0.6999999999999784173 ) ) ;
#24213 = CARTESIAN_POINT ( 'NONE',  ( -18.62325121933723437, 19.80375466501974913, 0.06723541799999455115 ) ) ;
#24214 = CARTESIAN_POINT ( 'NONE',  ( -10.69999999999999929, -127.0192926649000071, -34.11611703194000000 ) ) ;
#24215 = CARTESIAN_POINT ( 'NONE',  ( -15.76747295634271495, 11.30736579152925003, -4.336808689942018722E-16 ) ) ;
#24216 = CARTESIAN_POINT ( 'NONE',  ( -4.482429117347703773, -20.47894748273654741, -30.82872492568852962 ) ) ;
#24217 = CARTESIAN_POINT ( 'NONE',  ( -0.5496038873989572693, -2.045530029857146825, 226.6412452697800006 ) ) ;
#24218 = EDGE_CURVE ( 'NONE', #22703, #18256, #25839, .T. ) ;
#24219 = LINE ( 'NONE', #28774, #2716 ) ;
#24220 = AXIS2_PLACEMENT_3D ( 'NONE', #2653, #24373, #14469 ) ;
#24221 = ORIENTED_EDGE ( 'NONE', *, *, #21687, .F. ) ;
#24222 = CARTESIAN_POINT ( 'NONE',  ( 3.157381476932438868, -2.999772911539577702, -30.05126389020000488 ) ) ;
#24223 = CARTESIAN_POINT ( 'NONE',  ( 9.999999999971848297, -123.0374659623223010, -31.63552742122224259 ) ) ;
#24224 = ORIENTED_EDGE ( 'NONE', *, *, #3742, .T. ) ;
#24225 = CARTESIAN_POINT ( 'NONE',  ( -10.00000000045272763, -38.97546878308436646, -26.38794647281848427 ) ) ;
#24226 = CARTESIAN_POINT ( 'NONE',  ( 1.760648636159114933, 4.990344452800529851, -46.24079303332500501 ) ) ;
#24227 = ORIENTED_EDGE ( 'NONE', *, *, #21634, .T. ) ;
#24228 = ORIENTED_EDGE ( 'NONE', *, *, #19127, .F. ) ;
#24229 = DIRECTION ( 'NONE',  ( 0.000000000000000000, 0.000000000000000000, 1.000000000000000000 ) ) ;
#24230 = EDGE_LOOP ( 'NONE', ( #2302, #20372, #24393, #29641 ) ) ;
#24231 = DIRECTION ( 'NONE',  ( 1.000000000000000000, 0.000000000000000000, 0.000000000000000000 ) ) ;
#24232 = ORIENTED_EDGE ( 'NONE', *, *, #446, .T. ) ;
#24233 = CARTESIAN_POINT ( 'NONE',  ( 17.93011078763067090, 11.79183908526299085, -0.6999999999999784173 ) ) ;
#24234 = CARTESIAN_POINT ( 'NONE',  ( -7.861312627733068936, -2.231046042314999145, -39.72882113112014224 ) ) ;
#24235 = CARTESIAN_POINT ( 'NONE',  ( 0.2030058330167056890, 4.518950146840584381, -35.69999999999999574 ) ) ;
#24236 = CARTESIAN_POINT ( 'NONE',  ( 19.13554320545159371, 20.00034038933170422, -0.4554370248835840629 ) ) ;
#24237 = CARTESIAN_POINT ( 'NONE',  ( -24.14205448738587023, 13.78537896750705194, 6.042507811999997536 ) ) ;
#24238 = CARTESIAN_POINT ( 'NONE',  ( -22.78048776543632670, -14.11708351994821165, 5.719315394042070011 ) ) ;
#24239 = AXIS2_PLACEMENT_3D ( 'NONE', #20025, #12166, #29465 ) ;
#24240 = CARTESIAN_POINT ( 'NONE',  ( -25.96688743241739061, 8.776138983998601262, -0.6999999999999784173 ) ) ;
#24241 = VERTEX_POINT ( 'NONE', #12025 ) ;
#24242 = EDGE_CURVE ( 'NONE', #18572, #979, #3673, .T. ) ;
#24243 = CARTESIAN_POINT ( 'NONE',  ( -3.409041349409528632, -3.412796932024714014, -10.75149163099999505 ) ) ;
#24244 = CARTESIAN_POINT ( 'NONE',  ( 0.6752547517502489605, 4.742883336923179094, -28.06850711719999936 ) ) ;
#24245 = CARTESIAN_POINT ( 'NONE',  ( 0.000000000000000000, 0.000000000000000000, 142.0603150149999863 ) ) ;
#24246 = CARTESIAN_POINT ( 'NONE',  ( -12.75378086759999796, -22.00000000000000000, -31.28675134614999820 ) ) ;
#24247 = CARTESIAN_POINT ( 'NONE',  ( 20.28766220345061910, 20.00000013976770674, 0.7460156100000114865 ) ) ;
#24248 = CARTESIAN_POINT ( 'NONE',  ( 3.613223338493661174, -19.84398329827888219, -27.80061182959511257 ) ) ;
#24249 = CARTESIAN_POINT ( 'NONE',  ( -2.618143654921863295, 3.481518582925488658, -19.63064294430000345 ) ) ;
#24250 = FACE_OUTER_BOUND ( 'NONE', #30258, .T. ) ;
#24251 = CARTESIAN_POINT ( 'NONE',  ( -3.510330246760000161, -1.917702155200005976, -44.10000000000000142 ) ) ;
#24252 = CARTESIAN_POINT ( 'NONE',  ( 0.6231431573718050343, -3.499789347373825077, 230.8050258245700093 ) ) ;
#24253 = AXIS2_PLACEMENT_3D ( 'NONE', #30997, #26277, #26128 ) ;
#24254 = ORIENTED_EDGE ( 'NONE', *, *, #20097, .T. ) ;
#24255 = ADVANCED_FACE ( 'NONE', ( #16895 ), #28850, .T. ) ;
#24256 = CARTESIAN_POINT ( 'NONE',  ( -7.999999999718343524, -24.19750589173343869, -27.32947359979155166 ) ) ;
#24257 = CARTESIAN_POINT ( 'NONE',  ( 10.69999999999583729, -24.60099947294593292, -26.55635983988242188 ) ) ;
#24258 = ORIENTED_EDGE ( 'NONE', *, *, #11856, .F. ) ;
#24259 = EDGE_CURVE ( 'NONE', #3948, #14079, #19577, .T. ) ;
#24260 = DIRECTION ( 'NONE',  ( 1.000000000000000000, 0.000000000000000000, 0.000000000000000000 ) ) ;
#24261 = CARTESIAN_POINT ( 'NONE',  ( -16.26054471415775993, 10.04965037057037236, -0.6999999999999784173 ) ) ;
#24262 = VERTEX_POINT ( 'NONE', #29160 ) ;
#24263 = DIRECTION ( 'NONE',  ( 0.000000000000000000, 0.9396926207858125046, 0.3420201433259318358 ) ) ;
#24264 = VERTEX_POINT ( 'NONE', #26500 ) ;
#24265 = B_SPLINE_SURFACE_WITH_KNOTS ( 'NONE', 5, 5, ( 
 ( #28513, #14628, #627, #12563, #13890, #14776, #25857, #9900, #12251 ),
 ( #18603, #30883, #22024, #2090, #11680, #22169, #9313, #28200, #29090 ),
 ( #24378, #21871, #2971, #319, #2816, #28358, #7536, #17128, #4295 ),
 ( #11528, #12408, #477, #10059, #19655, #29238, #7678, #17280, #26890 ),
 ( #5329, #14933, #21130, #9153, #24530, #18757, #6803, #10666, #24682 ),
 ( #22323, #15086, #29396, #20261, #15232, #8135, #15388, #776, #12876 ) ),
 .UNSPECIFIED., .F., .F., .F.,
 ( 6, 6 ),
 ( 6, 3, 6 ),
 ( 64.89339659379999148, 88.33140247330000250 ),
 ( 8.011061266649999624, 8.811732102769999742, 9.612402938880000747 ),
 .UNSPECIFIED. ) ;
#24266 = ORIENTED_EDGE ( 'NONE', *, *, #31101, .F. ) ;
#24267 = EDGE_CURVE ( 'NONE', #23969, #25641, #24839, .T. ) ;
#24268 = VERTEX_POINT ( 'NONE', #24144 ) ;
#24269 = CARTESIAN_POINT ( 'NONE',  ( 6.795230380966086337, -8.420262557263953340, -36.71013853908947766 ) ) ;
#24270 = DIRECTION ( 'NONE',  ( 0.3090169943750400994, -0.9510565162951234441, 0.000000000000000000 ) ) ;
#24271 = CARTESIAN_POINT ( 'NONE',  ( 18.23252704342300845, -8.692634207812194092, -4.336808689942018722E-16 ) ) ;
#24272 = ORIENTED_EDGE ( 'NONE', *, *, #29712, .F. ) ;
#24273 = CARTESIAN_POINT ( 'NONE',  ( 1.776356839399999804E-15, -5.329070518200000398E-15, 227.7662452697800006 ) ) ;
#24274 = CARTESIAN_POINT ( 'NONE',  ( -14.94562240850000023, -8.628859120750000500, 5.000000000000000000 ) ) ;
#24275 = ADVANCED_FACE ( 'NONE', ( #700 ), #23862, .T. ) ;
#24276 = CARTESIAN_POINT ( 'NONE',  ( 19.29866511436280874, 19.63492491799039996, 0.3046098590000212436 ) ) ;
#24277 = LINE ( 'NONE', #2725, #29547 ) ;
#24278 = ORIENTED_EDGE ( 'NONE', *, *, #17060, .T. ) ;
#24279 = EDGE_CURVE ( 'NONE', #6080, #10911, #14948, .T. ) ;
#24280 = CARTESIAN_POINT ( 'NONE',  ( -4.706847372945446750, -0.8873292358359263776, -15.16199426529999705 ) ) ;
#24281 = VECTOR ( 'NONE', #10259, 1000.000000000000000 ) ;
#24282 = CARTESIAN_POINT ( 'NONE',  ( -7.999999999650268201, -15.05691661382650537, -37.86814300153927348 ) ) ;
#24283 = CARTESIAN_POINT ( 'NONE',  ( 26.80000000069999899, -3.281945028320000125E-15, 86.78285841090000474 ) ) ;
#24284 = AXIS2_PLACEMENT_3D ( 'NONE', #12405, #5018, #22020 ) ;
#24285 = CARTESIAN_POINT ( 'NONE',  ( 4.298353652097317124, -19.10214718657442390, -28.16242947664836649 ) ) ;
#24286 = DIRECTION ( 'NONE',  ( 1.000000000000000000, 0.000000000000000000, 0.000000000000000000 ) ) ;
#24287 = CARTESIAN_POINT ( 'NONE',  ( -24.77402022478258914, 12.61404137177703433, 4.439986940269814220 ) ) ;
#24288 = EDGE_CURVE ( 'NONE', #5682, #23569, #20570, .T. ) ;
#24289 = DIRECTION ( 'NONE',  ( -5.962915006522622422E-16, -0.4383711467890810676, -0.8987940462991651502 ) ) ;
#24290 = DIRECTION ( 'NONE',  ( 0.3633921898465291567, 0.9316362575375349842, 0.000000000000000000 ) ) ;
#24291 = CARTESIAN_POINT ( 'NONE',  ( 26.54997920389999777, 9.298361011320000813, 229.7313259189999712 ) ) ;
#24292 = CARTESIAN_POINT ( 'NONE',  ( -6.408211168649999401, 17.12116672390000005, 230.6999999999999886 ) ) ;
#24293 = EDGE_LOOP ( 'NONE', ( #11075, #11371, #30633, #7682 ) ) ;
#24294 = CARTESIAN_POINT ( 'NONE',  ( -4.541600168151700423, -0.1148504950298639971, -53.55673954922500002 ) ) ;
#24295 = CARTESIAN_POINT ( 'NONE',  ( 4.000000000000000000, -29.27600094726834712, -81.66227801707495360 ) ) ;
#24296 = CARTESIAN_POINT ( 'NONE',  ( -27.77052805885498898, -0.5052956280874019157, 0.7069222069999991920 ) ) ;
#24297 = CARTESIAN_POINT ( 'NONE',  ( 9.999999999922765781, -25.00000000003785061, -8.540325879148895183 ) ) ;
#24298 = AXIS2_PLACEMENT_3D ( 'NONE', #22668, #19998, #1431 ) ;
#24299 = ORIENTED_EDGE ( 'NONE', *, *, #14130, .T. ) ;
#24300 = AXIS2_PLACEMENT_3D ( 'NONE', #17771, #15724, #25340 ) ;
#24301 = FACE_BOUND ( 'NONE', #19230, .T. ) ;
#24302 = PRESENTATION_STYLE_ASSIGNMENT (( #7466 ) ) ;
#24303 = AXIS2_PLACEMENT_3D ( 'NONE', #11073, #20510, #16670 ) ;
#24304 = ORIENTED_EDGE ( 'NONE', *, *, #20256, .T. ) ;
#24305 = CARTESIAN_POINT ( 'NONE',  ( -3.686970300939999667, 0.4978338539504151838, -70.82548838946271985 ) ) ;
#24306 = CARTESIAN_POINT ( 'NONE',  ( 0.6090474298383116158, -27.79358669172298946, 3.904048352000033528 ) ) ;
#24307 = VERTEX_POINT ( 'NONE', #13247 ) ;
#24308 = CARTESIAN_POINT ( 'NONE',  ( -5.340187987486594068, -1.400932219821331870, -26.04656121680001135 ) ) ;
#24309 = CARTESIAN_POINT ( 'NONE',  ( -2.086681039676111737, -0.2757844063077397601, 226.6412452697800290 ) ) ;
#24310 = CARTESIAN_POINT ( 'NONE',  ( -0.9891938378274525157, -4.753657830815115837, -52.92706695232499925 ) ) ;
#24311 = EDGE_CURVE ( 'NONE', #27823, #18767, #1756, .T. ) ;
#24312 = FACE_OUTER_BOUND ( 'NONE', #9713, .T. ) ;
#24313 = PRESENTATION_STYLE_ASSIGNMENT (( #9684 ) ) ;
#24314 = DIRECTION ( 'NONE',  ( 0.000000000000000000, 1.000000000000000000, 0.000000000000000000 ) ) ;
#24315 = EDGE_CURVE ( 'NONE', #20583, #26453, #11928, .T. ) ;
#24316 = CYLINDRICAL_SURFACE ( 'NONE', #10790, 10.00000000000000178 ) ;
#24317 = EDGE_CURVE ( 'NONE', #19402, #11684, #27569, .T. ) ;
#24318 = EDGE_CURVE ( 'NONE', #26056, #24186, #10102, .T. ) ;
#24319 = VECTOR ( 'NONE', #17545, 1000.000000000000000 ) ;
#24320 = CARTESIAN_POINT ( 'NONE',  ( -17.38654519918314278, -22.00020860527460798, -27.03011121754735413 ) ) ;
#24321 = VERTEX_POINT ( 'NONE', #13408 ) ;
#24322 = CARTESIAN_POINT ( 'NONE',  ( 4.638687372183705193, -19.12054368226126400, -31.49126272761206025 ) ) ;
#24323 = CARTESIAN_POINT ( 'NONE',  ( 23.73463268742296961, -12.44713172126245126, 224.7819332099832081 ) ) ;
#24324 = AXIS2_PLACEMENT_3D ( 'NONE', #16160, #18037, #25774 ) ;
#24325 = AXIS2_PLACEMENT_3D ( 'NONE', #15731, #25345, #969 ) ;
#24326 = CARTESIAN_POINT ( 'NONE',  ( -10.46518171449999990, 6.538123262210000064, 232.6627643349999914 ) ) ;
#24327 = CARTESIAN_POINT ( 'NONE',  ( -8.699999999718668775, -5.981227587262315737, -27.94042817488295682 ) ) ;
#24328 = CARTESIAN_POINT ( 'NONE',  ( -8.359833048262370170, 8.751033796363188344, 232.0000000000050022 ) ) ;
#24329 = AXIS2_PLACEMENT_3D ( 'NONE', #25151, #3277, #25310 ) ;
#24330 = DIRECTION ( 'NONE',  ( 0.7071067811834159667, -0.6355433650310505778, 0.3099752105724545292 ) ) ;
#24331 = AXIS2_PLACEMENT_3D ( 'NONE', #1869, #23745, #20914 ) ;
#24332 = CARTESIAN_POINT ( 'NONE',  ( 3.653275382406361071, -2.426579979385206531, -0.6999999999999992895 ) ) ;
#24333 = CARTESIAN_POINT ( 'NONE',  ( -4.540209229552565340, -30.08687099007853405, -0.6999999999999784173 ) ) ;
#24334 = CARTESIAN_POINT ( 'NONE',  ( -25.84755624059999946, 9.037785233839999322, 230.0000000000000000 ) ) ;
#24335 = DIRECTION ( 'NONE',  ( 0.000000000000000000, 0.000000000000000000, -1.000000000000000000 ) ) ;
#24336 = CARTESIAN_POINT ( 'NONE',  ( -17.83928249680000278, 19.99999999999999645, -0.6999999999999992895 ) ) ;
#24337 = B_SPLINE_CURVE_WITH_KNOTS ( 'NONE', 3,
 ( #16799, #14760, #24358, #26412, #14456, #17263, #24055, #26870, #5313, #14917, #24512, #12543, #20103, #1371, #8426, #18025, #17570, #27792 ),
 .UNSPECIFIED., .F., .F.,
 ( 4, 2, 2, 2, 2, 2, 2, 2, 4 ),
 ( 0.000000000000000000, 0.1250000000000000000, 0.2500000000000000000, 0.3750000000000000000, 0.5000000000000000000, 0.6250000000000000000, 0.7500000000000000000, 0.8750000000000000000, 1.000000000000000000 ),
 .UNSPECIFIED. ) ;
#24338 = CARTESIAN_POINT ( 'NONE',  ( 11.95683611934412838, -1.871217229727538678, 232.0000002394077399 ) ) ;
#24339 = DIRECTION ( 'NONE',  ( 0.000000000000000000, 0.000000000000000000, -1.000000000000000000 ) ) ;
#24340 = LINE ( 'NONE', #12373, #21340 ) ;
#24341 = STYLED_ITEM ( 'NONE', ( #21484 ), #18548 ) ;
#24342 = ORIENTED_EDGE ( 'NONE', *, *, #4891, .F. ) ;
#24343 = DIRECTION ( 'NONE',  ( 0.000000000000000000, 0.000000000000000000, 1.000000000000000000 ) ) ;
#24344 = CARTESIAN_POINT ( 'NONE',  ( 24.25004754381673422, -14.97293715294370031, 224.2649987588634417 ) ) ;
#24345 = CONICAL_SURFACE ( 'NONE', #6261, 1.472846691535505848, 0.3390887027916915653 ) ;
#24346 = CARTESIAN_POINT ( 'NONE',  ( -3.468517234904584079, -2.575357395510375902, -56.67895058492499061 ) ) ;
#24347 = VECTOR ( 'NONE', #11257, 1000.000000000000114 ) ;
#24348 = VERTEX_POINT ( 'NONE', #25220 ) ;
#24349 = AXIS2_PLACEMENT_3D ( 'NONE', #24725, #3314, #20002 ) ;
#24350 = AXIS2_PLACEMENT_3D ( 'NONE', #29661, #1341, #27149 ) ;
#24351 = AXIS2_PLACEMENT_3D ( 'NONE', #5051, #7106, #17155 ) ;
#24352 = ORIENTED_EDGE ( 'NONE', *, *, #24664, .F. ) ;
#24353 = CARTESIAN_POINT ( 'NONE',  ( -17.38968115014047200, -25.66781448189618331, -23.39563497578856399 ) ) ;
#24354 = ORIENTED_EDGE ( 'NONE', *, *, #16389, .T. ) ;
#24355 = FACE_BOUND ( 'NONE', #26818, .T. ) ;
#24356 = DIRECTION ( 'NONE',  ( 0.6215393814730896249, -0.6030661632640409442, -0.5000000000040381032 ) ) ;
#24357 = CARTESIAN_POINT ( 'NONE',  ( -22.90527192528401201, 16.36193184990112570, 3.799999999999998046 ) ) ;
#24358 = CARTESIAN_POINT ( 'NONE',  ( 16.36439430656247040, 11.76631802980117669, -1.400000000000001910 ) ) ;
#24359 = DIRECTION ( 'NONE',  ( 0.000000000000000000, -0.3420201433259318913, 0.9396926207858126157 ) ) ;
#24360 = CARTESIAN_POINT ( 'NONE',  ( 3.904508939291349900, -1.994718106397494362, -11.41474735220000625 ) ) ;
#24361 =( GEOMETRIC_REPRESENTATION_CONTEXT ( 3 ) GLOBAL_UNCERTAINTY_ASSIGNED_CONTEXT ( ( #7782 ) ) GLOBAL_UNIT_ASSIGNED_CONTEXT ( ( #1485, #9015, #18766 ) ) REPRESENTATION_CONTEXT ( 'NONE', 'WORKASPACE' ) );
#24362 = LINE ( 'NONE', #29223, #11499 ) ;
#24363 = VERTEX_POINT ( 'NONE', #15312 ) ;
#24364 = CARTESIAN_POINT ( 'NONE',  ( 2.294646741299938952, -4.244716771087541751, -44.10000000002499121 ) ) ;
#24365 = CARTESIAN_POINT ( 'NONE',  ( -24.75645986059852177, -14.12045945554185522, 4.098702617000016701 ) ) ;
#24366 = CARTESIAN_POINT ( 'NONE',  ( 2.949882002856666130, 3.605460750137340131, -20.75622222230001057 ) ) ;
#24367 = CARTESIAN_POINT ( 'NONE',  ( 28.47939442936984733, 1.391723841383464277, 8.000000000000007105 ) ) ;
#24368 = CARTESIAN_POINT ( 'NONE',  ( 1.100000000000000089, -27.47799119300000115, 225.0000000000000000 ) ) ;
#24369 = B_SPLINE_SURFACE_WITH_KNOTS ( 'NONE', 5, 1, ( 
 ( #17316, #14359 ),
 ( #9778, #26923 ),
 ( #24247, #16855 ),
 ( #5359, #3000 ),
 ( #12592, #11978 ),
 ( #21590, #38 ),
 ( #19219, #28801 ),
 ( #7264, #26460 ),
 ( #28968, #7411 ),
 ( #13365, #961 ),
 ( #15114, #15563 ),
 ( #8018, #19846 ),
 ( #18074, #3774 ),
 ( #7862, #8319 ),
 ( #17465, #10551 ) ),
 .UNSPECIFIED., .F., .F., .F.,
 ( 6, 3, 3, 3, 6 ),
 ( 2, 2 ),
 ( 0.000000000000000000, 0.5777945772229999832, 1.155589154450000100, 2.022281020279999897, 2.888972886109999916 ),
 ( 6.550315845290000521E-15, 0.7031438909409999383 ),
 .UNSPECIFIED. ) ;
#24370 = VECTOR ( 'NONE', #21363, 1000.000000000000000 ) ;
#24371 = DIRECTION ( 'NONE',  ( 0.9316362575375356503, 0.3633921898465274913, 0.000000000000000000 ) ) ;
#24372 = AXIS2_PLACEMENT_3D ( 'NONE', #17362, #24760, #5254 ) ;
#24373 = DIRECTION ( 'NONE',  ( 0.000000000000000000, 0.000000000000000000, -1.000000000000000000 ) ) ;
#24374 = CARTESIAN_POINT ( 'NONE',  ( -3.130203125555106158, 5.106303518385050033, -45.05531229042499319 ) ) ;
#24375 = PLANE ( 'NONE',  #4182 ) ;
#24376 = CARTESIAN_POINT ( 'NONE',  ( -2.664535259099999568E-14, -26.80000000000000071, 223.8999999999999773 ) ) ;
#24377 = CARTESIAN_POINT ( 'NONE',  ( -12.29999999970000069, -27.00000000000000000, -28.40000000001083436 ) ) ;
#24378 = CARTESIAN_POINT ( 'NONE',  ( -23.94309786560000219, 13.28188914049999880, 230.0000000000000000 ) ) ;
#24379 = EDGE_CURVE ( 'NONE', #21319, #27710, #8235, .T. ) ;
#24380 = B_SPLINE_CURVE_WITH_KNOTS ( 'NONE', 3,
 ( #296, #19324, #26852, #29209, #24047, #28750, #24353, #7203, #7359, #2793, #7654 ),
 .UNSPECIFIED., .F., .F.,
 ( 4, 1, 1, 1, 2, 2, 4 ),
 ( 0.000000000000000000, 0.2499999999999976130, 0.3749999999999972244, 0.4374999999999980571, 0.4687499999999981681, 0.4999999999999983347, 1.000000000000000000 ),
 .UNSPECIFIED. ) ;
#24381 = LINE ( 'NONE', #14781, #28314 ) ;
#24383 = EDGE_LOOP ( 'NONE', ( #20782, #20780, #23700, #23114 ) ) ;
#24382 = CIRCLE ( 'NONE', #2774, 2.926829268290000119 ) ;
#24384 = CARTESIAN_POINT ( 'NONE',  ( -4.273414424137721213, 4.913340199448848367, -28.58728588869999143 ) ) ;
#24385 = AXIS2_PLACEMENT_3D ( 'NONE', #3281, #5177, #15242 ) ;
#24386 = ORIENTED_EDGE ( 'NONE', *, *, #30170, .F. ) ;
#24387 = CARTESIAN_POINT ( 'NONE',  ( 9.999999999971805664, -26.21475634739274696, -31.32191803010133668 ) ) ;
#24388 = CARTESIAN_POINT ( 'NONE',  ( 2.729852257651755210, -4.492922384981882011, -47.31669147672499776 ) ) ;
#24389 = VERTEX_POINT ( 'NONE', #20494 ) ;
#24390 = ADVANCED_FACE ( 'NONE', ( #30251 ), #20033, .F. ) ;
#24391 = VERTEX_POINT ( 'NONE', #18123 ) ;
#24392 = PRODUCT_CONTEXT ( 'NONE', #11779, 'mechanical' ) ;
#24393 = ORIENTED_EDGE ( 'NONE', *, *, #1449, .T. ) ;
#24394 = CARTESIAN_POINT ( 'NONE',  ( 20.27681456348847178, 20.00004247328156026, 229.2644764541421125 ) ) ;
#24395 = ORIENTED_EDGE ( 'NONE', *, *, #15863, .T. ) ;
#24396 = FACE_OUTER_BOUND ( 'NONE', #16367, .T. ) ;
#24397 = CARTESIAN_POINT ( 'NONE',  ( -16.81341597756113515, 9.900182044522454206, -0.6999999999999784173 ) ) ;
#24398 = DIRECTION ( 'NONE',  ( -0.7198537139083028835, 0.6941258031311204890, 0.000000000000000000 ) ) ;
#24399 = CARTESIAN_POINT ( 'NONE',  ( 0.3172472662966961954, 4.344971966744158642, -35.70000000000000284 ) ) ;
#24400 = CARTESIAN_POINT ( 'NONE',  ( -12.35171651922531666, -30.27052668731191432, -24.51507340929063616 ) ) ;
#24401 = CARTESIAN_POINT ( 'NONE',  ( -22.97593529893700648, 15.65128280014837081, 8.000000000000007105 ) ) ;
#24402 = CARTESIAN_POINT ( 'NONE',  ( 12.41421356240000051, 26.55509710711128335, -61.34142017886538412 ) ) ;
#24403 = CARTESIAN_POINT ( 'NONE',  ( -17.59696597919420213, 10.20816091468181774, -0.6999999999999784173 ) ) ;
#24404 = ORIENTED_EDGE ( 'NONE', *, *, #27456, .T. ) ;
#24405 = CARTESIAN_POINT ( 'NONE',  ( -5.680091681631305178, 1.608645723366325164, -8.310827254900006622 ) ) ;
#24406 = CARTESIAN_POINT ( 'NONE',  ( 5.869757812515316253, 0.5877190740209992104, -28.63116556699999649 ) ) ;
#24407 = CYLINDRICAL_SURFACE ( 'NONE', #10778, 3.000000000000002220 ) ;
#24408 = PRODUCT_DEFINITION_FORMATION_WITH_SPECIFIED_SOURCE ( 'ANY', '', #3119, .NOT_KNOWN. ) ;
#24409 = EDGE_CURVE ( 'NONE', #7124, #1598, #18810, .T. ) ;
#24410 = CARTESIAN_POINT ( 'NONE',  ( -7.999999999688209407, -9.149979919817011975, -35.02638174861068165 ) ) ;
#24411 = FACE_OUTER_BOUND ( 'NONE', #10806, .T. ) ;
#24412 = CARTESIAN_POINT ( 'NONE',  ( -2.290237947390000084, -7.805642660830000246, 227.7662452697800006 ) ) ;
#24413 = DIRECTION ( 'NONE',  ( 1.000000000000000000, -0.000000000000000000, 0.000000000000000000 ) ) ;
#24414 = CARTESIAN_POINT ( 'NONE',  ( -0.7560282158644084927, 4.289996408053712962, -19.83583244400000112 ) ) ;
#24415 = B_SPLINE_CURVE_WITH_KNOTS ( 'NONE', 3,
 ( #18859, #6433, #20596, #25800, #25648, #4078 ),
 .UNSPECIFIED., .F., .F.,
 ( 4, 2, 4 ),
 ( 0.000000000000000000, 0.5000000000000000000, 1.000000000000000000 ),
 .UNSPECIFIED. ) ;
#24416 = CARTESIAN_POINT ( 'NONE',  ( 1.605176535610508326, -27.75389821387976852, 5.104056378000016103 ) ) ;
#24417 = CARTESIAN_POINT ( 'NONE',  ( -24.54452542612009225, -14.48555670042145138, 3.920144560000005107 ) ) ;
#24418 = CARTESIAN_POINT ( 'NONE',  ( 353532.1637640000554, -353580.3905929999310, -28.39999994950992956 ) ) ;
#24419 = ORIENTED_EDGE ( 'NONE', *, *, #14790, .F. ) ;
#24420 = CARTESIAN_POINT ( 'NONE',  ( 18.23234009198083072, -8.693620616447864435, -0.6999999999999785283 ) ) ;
#24421 = CARTESIAN_POINT ( 'NONE',  ( -23.81569860410000317, -13.75000000000000000, 6.099999999630000502 ) ) ;
#24422 = VERTEX_POINT ( 'NONE', #17808 ) ;
#24423 = CARTESIAN_POINT ( 'NONE',  ( 3.040504021322313122, 1.733590290792417887, -0.6999999999999784173 ) ) ;
#24424 = CARTESIAN_POINT ( 'NONE',  ( 17.16657240410000185, -9.000000001100003644, -1.399999999999998579 ) ) ;
#24425 = VERTEX_POINT ( 'NONE', #20653 ) ;
#24426 = CARTESIAN_POINT ( 'NONE',  ( -4.883042975539221509, -0.7801726600661595956, -44.10000000002498410 ) ) ;
#24427 = VERTEX_POINT ( 'NONE', #27418 ) ;
#24428 = EDGE_CURVE ( 'NONE', #26831, #16211, #15708, .T. ) ;
#24429 = ORIENTED_EDGE ( 'NONE', *, *, #15918, .F. ) ;
#24430 = VERTEX_POINT ( 'NONE', #12794 ) ;
#24431 = B_SPLINE_CURVE_WITH_KNOTS ( 'NONE', 5,
 ( #9103, #18703, #15713, #28152, #13360, #30197 ),
 .UNSPECIFIED., .F., .F.,
 ( 6, 6 ),
 ( -16.82733224740000111, 0.000000000000000000 ),
 .UNSPECIFIED. ) ;
#24432 = CARTESIAN_POINT ( 'NONE',  ( 7.312007425309010600, -7.897185061697537201, -36.96526048002264986 ) ) ;
#24433 = DIRECTION ( 'NONE',  ( 0.3633921898465289901, 0.9316362575375348731, 0.000000000000000000 ) ) ;
#24434 = CARTESIAN_POINT ( 'NONE',  ( 16.89818815126293217, 9.923569363153179168, -0.6999999999999785283 ) ) ;
#24435 = VERTEX_POINT ( 'NONE', #26004 ) ;
#24436 = CARTESIAN_POINT ( 'NONE',  ( -24.70448872506469229, 12.74983733322420321, 5.760266710000017554 ) ) ;
#24437 = CARTESIAN_POINT ( 'NONE',  ( 28.35945635826399780, 7.983396865336832349, 1.000000000000000888 ) ) ;
#24438 = CARTESIAN_POINT ( 'NONE',  ( -17.35614611410398211, -31.99972351093158807, -29.95953050019675246 ) ) ;
#24439 = DIRECTION ( 'NONE',  ( 0.000000000000000000, -1.000000000000000000, 0.000000000000000000 ) ) ;
#24440 = EDGE_CURVE ( 'NONE', #28644, #23122, #10290, .T. ) ;
#24441 = ORIENTED_EDGE ( 'NONE', *, *, #4504, .T. ) ;
#24442 = EDGE_CURVE ( 'NONE', #2785, #18386, #23337, .T. ) ;
#24443 = CARTESIAN_POINT ( 'NONE',  ( -10.69999999989999928, -25.00000000000000000, -7.274962171499997687 ) ) ;
#24444 = CARTESIAN_POINT ( 'NONE',  ( 0.6713911862884133219, -5.438992117826878747, -17.37054674910000074 ) ) ;
#24445 = CARTESIAN_POINT ( 'NONE',  ( 18.26639035967037827, -8.979988381807324060, -0.6999999999999784173 ) ) ;
#24446 = DIRECTION ( 'NONE',  ( 0.9316362575375356503, 0.3633921898465274913, 0.000000000000000000 ) ) ;
#24447 = CARTESIAN_POINT ( 'NONE',  ( 8.349999999921791982, -9.149979919791261906, -35.02638174844237540 ) ) ;
#24448 = CARTESIAN_POINT ( 'NONE',  ( 28.50000000000000000, 1.273924582309999984E-25, 222.0000000000000000 ) ) ;
#24449 = CARTESIAN_POINT ( 'NONE',  ( -24.83828966697487317, 12.48688602537153791, 4.853901705271463030 ) ) ;
#24450 = ADVANCED_FACE ( 'NONE', ( #4445 ), #17306, .F. ) ;
#24451 = CARTESIAN_POINT ( 'NONE',  ( 8.000000000473534101, -13.78877417416307871, -34.18207016520864983 ) ) ;
#24452 = CARTESIAN_POINT ( 'NONE',  ( 1.645560275461343203, -28.45273235261698019, 4.999998581000003384 ) ) ;
#24453 = CARTESIAN_POINT ( 'NONE',  ( 21.20256267760000313, 17.00023892710000339, 230.0000000000000000 ) ) ;
#24454 = CARTESIAN_POINT ( 'NONE',  ( -17.67198296649999634, -4.679706496339999688, 230.6999999999999886 ) ) ;
#24455 = ORIENTED_EDGE ( 'NONE', *, *, #20579, .T. ) ;
#24456 = CARTESIAN_POINT ( 'NONE',  ( 0.9406167415663759801, 5.909121140430885433, -53.93500058692499977 ) ) ;
#24457 = CARTESIAN_POINT ( 'NONE',  ( -8.699999999671032214, -18.09762814832684796, -34.21342158600526062 ) ) ;
#24458 = CARTESIAN_POINT ( 'NONE',  ( -17.83930458829795640, 19.99999999999961631, 0.000000000000000000 ) ) ;
#24459 = EDGE_CURVE ( 'NONE', #4649, #19818, #27347, .T. ) ;
#24460 = CARTESIAN_POINT ( 'NONE',  ( -4.556827411881193335, 0.9672853314650907697, -68.10000000002500542 ) ) ;
#24461 = ORIENTED_EDGE ( 'NONE', *, *, #2133, .T. ) ;
#24462 = B_SPLINE_CURVE_WITH_KNOTS ( 'NONE', 3,
 ( #15211, #27326, #5765, #10345, #24659, #12856 ),
 .UNSPECIFIED., .F., .F.,
 ( 4, 2, 4 ),
 ( 0.000000000000000000, 0.5000000000000008882, 1.000000000000000000 ),
 .UNSPECIFIED. ) ;
#24463 = CARTESIAN_POINT ( 'NONE',  ( -3.444197478484224195, 0.6290193840551402404, -91.21022378307108625 ) ) ;
#24464 = B_SPLINE_SURFACE_WITH_KNOTS ( 'NONE', 5, 5, ( 
 ( #13204, #1108, #22662, #17918, #25177, #27528, #5974, #10868, #13371 ),
 ( #29741, #15420, #18234, #3610, #15894, #18404, #27682, #6130, #20608 ),
 ( #3780, #25025, #5668, #5822, #22979, #30206, #6294, #25497, #27383 ),
 ( #11171, #16048, #18713, #25964, #11486, #30532, #21089, #16355, #28161 ),
 ( #18561, #30836, #28003, #23292, #4400, #14005, #23457, #4252, #13847 ),
 ( #1889, #25813, #23612, #4556, #11638, #11332, #2048, #25660, #14157 ) ),
 .UNSPECIFIED., .F., .F., .F.,
 ( 6, 6 ),
 ( 6, 3, 6 ),
 ( 65.40639850639999509, 88.68172752359998867 ),
 ( 8.011061266649999624, 9.371850724429998891, 10.73264018220000082 ),
 .UNSPECIFIED. ) ;
#24465 = SHAPE_REPRESENTATION_RELATIONSHIP ( 'NONE' , 'NONE' ,  #30659, #12524 ) ;
#24466 = ORIENTED_EDGE ( 'NONE', *, *, #23489, .F. ) ;
#24467 = DIRECTION ( 'NONE',  ( 0.000000000000000000, 0.000000000000000000, 1.000000000000000000 ) ) ;
#24468 = CARTESIAN_POINT ( 'NONE',  ( -10.00000000009909407, -126.3827248090510835, -33.44530783418806408 ) ) ;
#24469 = ORIENTED_EDGE ( 'NONE', *, *, #6937, .T. ) ;
#24470 = CARTESIAN_POINT ( 'NONE',  ( 5.307277461537168506, -2.951504967840870464, -26.93037294500000201 ) ) ;
#24471 = EDGE_CURVE ( 'NONE', #7965, #25224, #25483, .T. ) ;
#24472 = DIRECTION ( 'NONE',  ( 1.000000000000000000, 0.000000000000000000, 0.000000000000000000 ) ) ;
#24473 = CARTESIAN_POINT ( 'NONE',  ( 4.101176313917077820, -1.931410228222282921, -52.29872167392500160 ) ) ;
#24474 = CARTESIAN_POINT ( 'NONE',  ( -22.63992238019999803, -14.34133587289999845, 225.0000000000000000 ) ) ;
#24475 = CARTESIAN_POINT ( 'NONE',  ( -15.86808677770000209, 10.47263190749999495, -1.399999999599998990 ) ) ;
#24476 = PRODUCT_DEFINITION_CONTEXT ( 'detailed design', #30060, 'design' ) ;
#24477 = CARTESIAN_POINT ( 'NONE',  ( 23.55447120710000064, 16.04539730700000177, 222.0000000000000000 ) ) ;
#24478 = DIRECTION ( 'NONE',  ( 1.821459649777283484E-13, -0.9753733754015535551, 0.2205601472564346632 ) ) ;
#24479 = ORIENTED_EDGE ( 'NONE', *, *, #12709, .F. ) ;
#24480 = FACE_OUTER_BOUND ( 'NONE', #14833, .T. ) ;
#24481 = CARTESIAN_POINT ( 'NONE',  ( -24.98081131316241255, -13.71897606304888662, 4.999998581000003384 ) ) ;
#24482 = CARTESIAN_POINT ( 'NONE',  ( -0.8673174292429999266, -12.23557166350000003, 232.6627643349999914 ) ) ;
#24483 = CARTESIAN_POINT ( 'NONE',  ( -27.75400871128895375, 8.590834169133980680, 1.000000000000000888 ) ) ;
#24484 = CARTESIAN_POINT ( 'NONE',  ( 24.07552309629999954, -13.90001137839999856, 223.9000014189999774 ) ) ;
#24485 = CARTESIAN_POINT ( 'NONE',  ( -2.895630725101765890, -26.64812433595227503, 209.9519070181412701 ) ) ;
#24486 = CARTESIAN_POINT ( 'NONE',  ( 3.361768113024335758, -2.599356797695480115, -0.6999999999999992895 ) ) ;
#24487 = CARTESIAN_POINT ( 'NONE',  ( -4.627881920500872326, -30.66785676076818490, -0.5592437529999827461 ) ) ;
#24488 = CARTESIAN_POINT ( 'NONE',  ( 27.50000000000000000, -3.367667472999999580E-15, 143.6055512739999926 ) ) ;
#24489 = CARTESIAN_POINT ( 'NONE',  ( 23.77307140678977504, -14.41181874416537134, 4.895781291000017355 ) ) ;
#24490 = CARTESIAN_POINT ( 'NONE',  ( 0.000000000000000000, 0.000000000000000000, 190.0000000000000000 ) ) ;
#24491 = COLOUR_RGB ( '', 0.40784314, 0.44705882, 0.49803922) ;
#24492 = CARTESIAN_POINT ( 'NONE',  ( -7.999999999729964451, -28.19367756375590872, -25.64455236481611777 ) ) ;
#24493 = CARTESIAN_POINT ( 'NONE',  ( -0.9482832863833026149, -3.805503486056848406, -68.10000000002499121 ) ) ;
#24494 = EDGE_CURVE ( 'NONE', #20880, #17294, #14804, .T. ) ;
#24495 = EDGE_LOOP ( 'NONE', ( #10602, #18926, #6346, #7571 ) ) ;
#24496 = CARTESIAN_POINT ( 'NONE',  ( -4.960227444680000097, -16.90556345619999945, 230.0904314459999966 ) ) ;
#24497 = EDGE_CURVE ( 'NONE', #29115, #24684, #28354, .T. ) ;
#24498 = EDGE_CURVE ( 'NONE', #9514, #5024, #17162, .T. ) ;
#24499 = CARTESIAN_POINT ( 'NONE',  ( 24.60666743799999878, -12.93650359530000138, 225.0000014190000002 ) ) ;
#24500 = CARTESIAN_POINT ( 'NONE',  ( 5.506968775199813315, -0.09733528975458538568, -58.89793411332500739 ) ) ;
#24501 = ORIENTED_EDGE ( 'NONE', *, *, #5145, .F. ) ;
#24502 = B_SPLINE_CURVE_WITH_KNOTS ( 'NONE', 3,
 ( #30321, #18362, #27958, #7482, #14886, #2606, #16920, #15038, #21808, #24320, #14420, #21968, #265, #24166, #12200, #26830, #28885, #29182, #19601, #29036, #12359, #26527, #5427, #17076, #21658, #7629 ),
 .UNSPECIFIED., .F., .F.,
 ( 4, 2, 2, 1, 1, 2, 2, 2, 2, 2, 1, 1, 2, 2, 4 ),
 ( 0.000000000000000000, 0.1249999999999961142, 0.1874999999999943379, 0.2187499999999933109, 0.2343749999999934774, 0.2421874999999935885, 0.2499999999999936717, 0.4999999999999868994, 0.6249999999999825695, 0.6874999999999803491, 0.7187499999999782396, 0.7343749999999771294, 0.7421874999999775735, 0.7499999999999780176, 1.000000000000000000 ),
 .UNSPECIFIED. ) ;
#24503 = ORIENTED_EDGE ( 'NONE', *, *, #23291, .F. ) ;
#24504 = CIRCLE ( 'NONE', #13302, 26.80000000000000071 ) ;
#24505 = DIRECTION ( 'NONE',  ( -0.000000000000000000, 1.000000000000000000, -2.258510841069999963E-12 ) ) ;
#24506 = VERTEX_POINT ( 'NONE', #30723 ) ;
#24507 = FILL_AREA_STYLE_COLOUR ( '', #18181 ) ;
#24508 = CARTESIAN_POINT ( 'NONE',  ( -16.81341597763548990, -10.09981795544978311, -0.6999999999999784173 ) ) ;
#24509 = CARTESIAN_POINT ( 'NONE',  ( -22.90527192528401201, 16.36193184990112570, 2.400000000000013234 ) ) ;
#24510 = VECTOR ( 'NONE', #20278, 1000.000000000000000 ) ;
#24511 = UNCERTAINTY_MEASURE_WITH_UNIT (LENGTH_MEASURE( 1.000000000000000082E-05 ), #572, 'distance_accuracy_value', 'NONE');
#24512 = CARTESIAN_POINT ( 'NONE',  ( 17.93289043380325154, 11.80217809782661398, -1.400000000000001910 ) ) ;
#24513 = AXIS2_PLACEMENT_3D ( 'NONE', #23632, #2381, #16221 ) ;
#24514 = CARTESIAN_POINT ( 'NONE',  ( 24.54884435365858053, -13.04717673649832044, 6.002806400000004317 ) ) ;
#24515 = CARTESIAN_POINT ( 'NONE',  ( 0.3624384587677526026, -4.645391411234340850, -9.393384211799999051 ) ) ;
#24516 = CARTESIAN_POINT ( 'NONE',  ( 27.98121187870611593, -9.706323496128696604, 8.000000000000007105 ) ) ;
#24517 = ORIENTED_EDGE ( 'NONE', *, *, #25675, .T. ) ;
#24518 = CARTESIAN_POINT ( 'NONE',  ( 2.821870666190524179, -3.684768625846054135, -44.10000000002499831 ) ) ;
#24519 = CARTESIAN_POINT ( 'NONE',  ( 24.54452541844319668, 14.48555669908156851, 3.920144559000027229 ) ) ;
#24520 = B_SPLINE_CURVE_WITH_KNOTS ( 'NONE', 1,
 ( #20594, #30034 ),
 .UNSPECIFIED., .F., .F.,
 ( 2, 2 ),
 ( -2.555882182119999914E-06, 0.7000000000009999335 ),
 .UNSPECIFIED. ) ;
#24521 = CARTESIAN_POINT ( 'NONE',  ( -2.618143654921863295, 3.481518582925488658, -19.63064294430000345 ) ) ;
#24522 = CARTESIAN_POINT ( 'NONE',  ( -12.35171651922521718, -23.72947331268410309, -32.28492659110577279 ) ) ;
#24523 = B_SPLINE_CURVE_WITH_KNOTS ( 'NONE', 5,
 ( #17875, #27479, #15525, #4046, #20409, #29997, #3567, #11128, #18030 ),
 .UNSPECIFIED., .F., .F.,
 ( 6, 3, 6 ),
 ( 8.011061266649999624, 9.405960541640000727, 10.80085981660000094 ),
 .UNSPECIFIED. ) ;
#24524 = CARTESIAN_POINT ( 'NONE',  ( -27.54391550559999757, 3.373045393730000103E-15, 187.0437466829999948 ) ) ;
#24525 = CARTESIAN_POINT ( 'NONE',  ( -23.50695179570000093, -14.84192241259999889, 225.0000014190000002 ) ) ;
#24526 = CARTESIAN_POINT ( 'NONE',  ( 3.314820598666778917, -5.455691467570147779, -46.56669147682499954 ) ) ;
#24527 = CARTESIAN_POINT ( 'NONE',  ( -7.999999999971132425, -116.4789120197461187, 10.39182877040068931 ) ) ;
#24528 = CARTESIAN_POINT ( 'NONE',  ( 0.9876156986561913653, -26.78228253905960798, 224.5086268448359874 ) ) ;
#24529 = DIRECTION ( 'NONE',  ( 1.000000000000000000, 0.000000000000000000, 0.000000000000000000 ) ) ;
#24530 = CARTESIAN_POINT ( 'NONE',  ( -27.53132592989999949, 4.642205353319999617, 229.7313259299999686 ) ) ;
#24531 = AXIS2_PLACEMENT_3D ( 'NONE', #9915, #4570, #11655 ) ;
#24532 = EDGE_CURVE ( 'NONE', #15209, #3166, #9150, .T. ) ;
#24533 = CARTESIAN_POINT ( 'NONE',  ( -4.299999999899999814, -29.92682926828999967, -28.39999999989999324 ) ) ;
#24534 = ORIENTED_EDGE ( 'NONE', *, *, #6301, .T. ) ;
#24535 = CARTESIAN_POINT ( 'NONE',  ( -6.085238278930475531, -0.01014600953121863602, -28.16856466009999593 ) ) ;
#24536 = AXIS2_PLACEMENT_3D ( 'NONE', #5495, #12734, #24549 ) ;
#24537 = EDGE_CURVE ( 'NONE', #6463, #3666, #13572, .T. ) ;
#24538 = VERTEX_POINT ( 'NONE', #2087 ) ;
#24539 = CARTESIAN_POINT ( 'NONE',  ( 24.82162974202869421, -12.51998933900577349, 4.689351482000003735 ) ) ;
#24540 = CARTESIAN_POINT ( 'NONE',  ( 4.432674687120906398, 4.607520344841867121, -49.17426496242499923 ) ) ;
#24541 = EDGE_LOOP ( 'NONE', ( #21793, #7692, #15693, #5116 ) ) ;
#24542 = ORIENTED_EDGE ( 'NONE', *, *, #2234, .T. ) ;
#24543 = DIRECTION ( 'NONE',  ( 0.000000000000000000, 0.000000000000000000, 1.000000000000000000 ) ) ;
#24544 = EDGE_LOOP ( 'NONE', ( #19815, #8974, #818, #17889, #15205 ) ) ;
#24545 = CARTESIAN_POINT ( 'NONE',  ( 20.06951727433725452, 19.99997495482045551, 229.7339536094710581 ) ) ;
#24546 = ORIENTED_EDGE ( 'NONE', *, *, #6052, .F. ) ;
#24547 = CARTESIAN_POINT ( 'NONE',  ( -12.51085694169142926, 20.99999999990085087, -69.72135916458235272 ) ) ;
#24548 = DIRECTION ( 'NONE',  ( 0.000000000000000000, 0.000000000000000000, -1.000000000000000000 ) ) ;
#24549 = DIRECTION ( 'NONE',  ( 0.7071067811865475727, 0.7071067811865475727, 0.000000000000000000 ) ) ;
#24550 = CARTESIAN_POINT ( 'NONE',  ( -27.63177356679999974, 3.383804547729999744E-15, 87.36052363810000543 ) ) ;
#24551 = AXIS2_PLACEMENT_3D ( 'NONE', #2684, #29114, #18394 ) ;
#24552 = CARTESIAN_POINT ( 'NONE',  ( -12.48413792322954308, -31.09676965128281978, -24.99217446298782619 ) ) ;
#24553 = CARTESIAN_POINT ( 'NONE',  ( -3.737088657310626338, 2.230226196412739892, -0.6999999999999992895 ) ) ;
#24554 = CARTESIAN_POINT ( 'NONE',  ( 0.6465148687819723961, -4.727082501359223699, 0.5643759519999985708 ) ) ;
#24555 = CARTESIAN_POINT ( 'NONE',  ( -23.93396852079376202, -14.14368280436500491, 223.9267465465173927 ) ) ;
#24556 = CIRCLE ( 'NONE', #8447, 5.400000000370001274 ) ;
#24557 = EDGE_LOOP ( 'NONE', ( #4306, #8300, #27028, #24614 ) ) ;
#24558 = CARTESIAN_POINT ( 'NONE',  ( 0.3624384587677526026, -4.645391411234340850, -9.393384211799999051 ) ) ;
#24559 = CARTESIAN_POINT ( 'NONE',  ( 1.882647771056453756, 3.960165260869607629, -31.65113063600000487 ) ) ;
#24560 = CARTESIAN_POINT ( 'NONE',  ( 0.000000000000000000, 0.000000000000000000, 142.0603150149999863 ) ) ;
#24561 = AXIS2_PLACEMENT_3D ( 'NONE', #16035, #20442, #11009 ) ;
#24562 = DIRECTION ( 'NONE',  ( 0.000000000000000000, 0.000000000000000000, 1.000000000000000000 ) ) ;
#24563 = DIRECTION ( 'NONE',  ( 1.000000000000000000, -1.381176317861079950E-13, 9.436729139529790430E-14 ) ) ;
#24564 = SURFACE_STYLE_FILL_AREA ( #5360 ) ;
#24565 = CARTESIAN_POINT ( 'NONE',  ( 9.499999999636983716, -18.24529294700720783, -35.03355057858191657 ) ) ;
#24566 = CARTESIAN_POINT ( 'NONE',  ( -17.93324555128263142, -9.020011618190519442, -0.6999999999999784173 ) ) ;
#24567 = EDGE_CURVE ( 'NONE', #20670, #20967, #12644, .T. ) ;
#24568 = B_SPLINE_CURVE_WITH_KNOTS ( 'NONE', 3,
 ( #19371, #29575, #24555, #29263, #19838, #2836, #9766, #21896, #17149, #26915, #22048, #12280 ),
 .UNSPECIFIED., .F., .F.,
 ( 4, 2, 2, 2, 2, 4 ),
 ( 0.000000000000000000, 0.2500000000000155986, 0.5000000000000311973, 0.6250000000000234257, 0.7500000000000156541, 1.000000000000000000 ),
 .UNSPECIFIED. ) ;
#24569 = DIRECTION ( 'NONE',  ( -6.901835126637476841E-14, 5.775494631892377345E-13, -1.000000000000000000 ) ) ;
#24570 = CARTESIAN_POINT ( 'NONE',  ( -3.510330247570000228, -1.917702154400000136, -43.40000000037299799 ) ) ;
#24571 = CARTESIAN_POINT ( 'NONE',  ( 0.3123980048451518443, -3.499890163169941726, 230.8301842479583286 ) ) ;
#24572 = EDGE_LOOP ( 'NONE', ( #27635, #17337, #24517, #1862 ) ) ;
#24573 = VECTOR ( 'NONE', #5923, 1000.000000000000000 ) ;
#24574 = CARTESIAN_POINT ( 'NONE',  ( 1.533144572060379796, -28.45911136072525238, 4.493506933999996455 ) ) ;
#24575 = CARTESIAN_POINT ( 'NONE',  ( -3.687990083126857499, -19.94926840187814676, -27.74926085347921045 ) ) ;
#24576 = ORIENTED_EDGE ( 'NONE', *, *, #18279, .F. ) ;
#24577 = CARTESIAN_POINT ( 'NONE',  ( 26.87806031854113087, 10.31605756234181115, 8.000000000000007105 ) ) ;
#24578 = DIRECTION ( 'NONE',  ( 0.000000000000000000, 0.000000000000000000, -1.000000000000000000 ) ) ;
#24579 = ORIENTED_EDGE ( 'NONE', *, *, #10234, .T. ) ;
#24580 = CARTESIAN_POINT ( 'NONE',  ( -4.827739145450332892, 0.2194149372997978298, -44.10000000002499121 ) ) ;
#24581 = VERTEX_POINT ( 'NONE', #8838 ) ;
#24582 = ORIENTED_EDGE ( 'NONE', *, *, #18072, .F. ) ;
#24583 = ORIENTED_EDGE ( 'NONE', *, *, #21800, .F. ) ;
#24584 = CARTESIAN_POINT ( 'NONE',  ( 25.32889099250000342, 14.06639286550000101, 229.7625741969999922 ) ) ;
#24585 = VECTOR ( 'NONE', #14733, 1000.000000000000114 ) ;
#24586 = DIRECTION ( 'NONE',  ( 0.000000000000000000, -1.000000000000000000, 0.000000000000000000 ) ) ;
#24587 = CARTESIAN_POINT ( 'NONE',  ( 16.37473331892315542, -8.236461616552139375, -0.6999999999999784173 ) ) ;
#24588 = EDGE_LOOP ( 'NONE', ( #30307, #21608, #23082, #4304 ) ) ;
#24589 = CARTESIAN_POINT ( 'NONE',  ( -24.78871709450119809, 12.58522962245461585, 5.507123707999994622 ) ) ;
#24590 =( BOUNDED_SURFACE ( )  B_SPLINE_SURFACE ( 5, 5, ( 
 ( #2359, #7377, #26428, #2047, #21236, #2654 ),
 ( #315, #14623, #19182, #12247, #21867, #11941 ),
 ( #29085, #4707, #30989, #9419, #7531, #2203 ),
 ( #30835, #4868, #9894, #7066, #9265, #19026 ),
 ( #28769, #18871, #16656, #28468, #14471, #14156 ),
 ( #11793, #5784, #29392, #7673, #26886, #7829 ),
 ( #20114, #14929, #8129, #10206, #24677, #24374 ),
 ( #3111, #12708, #22317, #2812, #27341, #7981 ),
 ( #24981, #13018, #771, #29852, #1072, #17431 ),
 ( #24833, #19804, #5627, #10662, #10055, #17581 ),
 ( #27036, #15382, #10362, #27189, #19954, #24526 ),
 ( #22475, #19650, #5473, #12404, #924, #29546 ),
 ( #20255, #29233, #17276, #17727, #15080, #15228 ),
 ( #22629, #472, #8287, #17882, #5325, #2964 ),
 ( #3265, #12871, #12557, #27487, #22165, #10515 ),
 ( #3417, #622, #29703, #14772, #22016, #10981 ),
 ( #27809, #25138, #13168, #20734, #3574, #30169 ),
 ( #30007, #6089, #6256, #25623, #15859, #6411 ),
 ( #10828, #3897, #3735, #8601, #13489, #6562 ),
 ( #4055, #18674, #4207, #5933, #25463, #13334 ),
 ( #27968, #23256, #13808, #23422, #23105, #16162 ),
 ( #25776, #1547, #18201, #1852, #11137, #22942 ),
 ( #11452, #15687, #8440, #15533, #30335, #13651 ),
 ( #30498, #1386, #20415, #8764, #18523, #20573 ),
 ( #18373, #16010, #1697, #21051, #22778, #20899 ),
 ( #18039, #11295, #8923, #28125, #25301, #30652 ),
 ( #9078, #1227, #27646, #16624, #7035, #26656 ),
 ( #10135, #21944, #6869, #7760, #26966, #14705 ),
 ( #15011, #30956, #7609, #17203, #2165, #19579 ),
 ( #23579, #395, #26809, #11754, #29313, #5094 ),
 ( #24294, #16471, #19734, #17361, #5253, #2012 ),
 ( #18834, #9383, #23729, #24609, #28436, #14865 ),
 ( #5402, #3041, #9227, #12634, #24456, #9981 ),
 ( #2890, #22245, #12483, #25930, #2742, #702 ),
 ( #554, #29162, #30799, #12338, #18989, #22097 ),
 ( #10292, #28275, #6717, #4365, #21361, #16319 ),
 ( #13968, #4523, #11603, #21201, #28594, #26084 ),
 ( #14121, #10442, #1005, #1471, #8365, #20186 ),
 ( #27420, #23025, #10593, #20340, #5706, #22867 ),
 ( #27728, #1310, #5553, #851, #22561, #5858 ),
 ( #20035, #29778, #7909, #27119, #3500, #17513 ),
 ( #29632, #19892, #29473, #6173, #15773, #8061 ),
 ( #24917, #15156, #25386, #25067, #24758, #10905 ),
 ( #1146, #13249, #27572, #8209, #17811, #17960 ),
 ( #13410, #3193, #20496, #13096, #3824, #15616 ),
 ( #30097, #8524, #15463, #22704, #12798, #10740 ),
 ( #15315, #22405, #17657, #27269, #3343, #29937 ),
 ( #12951, #18125, #6018, #25222, #3652, #9152 ),
 ( #6802, #30574, #28199, #23339, #28356, #21278 ),
 ( #23500, #2089, #1934, #16399, #9002, #6641 ),
 ( #26006, #11062, #30725, #11527, #11679, #21129 ),
 ( #18755, #1622, #4447, #18445, #1782, #30253 ),
 ( #14049, #18602, #20657, #23653, #8682, #18285 ),
 ( #20968, #27892, #6336, #15933, #25541, #28043 ),
 ( #16239, #4294, #3978, #13574, #23181, #11212 ),
 ( #25856, #20814, #11372, #8840, #13889, #30421 ),
 ( #6487, #16088, #25700, #4131, #13728, #25406 ),
 ( #24930, #27134, #3209, #3669, #12964, #3513 ),
 ( #30115, #17526, #22574, #8543, #13271, #5568 ),
 ( #3357, #17829, #5723, #864, #1018, #19903 ),
 ( #15482, #29485, #10605, #10457, #24773, #20052 ),
 ( #27746, #29647, #27283, #15330, #10307, #18143 ),
 ( #3839, #22884, #12817, #13111, #25240, #8381 ),
 ( #20201, #20359, #25082, #13426, #716, #1325 ),
 ( #6192, #27591, #8225, #10920, #20515, #29793 ),
 ( #15793, #27436, #8075, #17670, #7924, #5872 ),
 ( #22421, #22720, #1164, #10759, #15169, #29952 ),
 ( #17980, #6032, #15630, #25719, #9020, #1951 ),
 ( #18929, #30900, #20676, #6506, #21144, #3995 ),
 ( #30440, #25876, #11546, #16106, #9168, #6658 ),
 ( #13593, #18463, #18771, #28528, #20988, #25558 ),
 ( #4152, #4312, #27912, #21296, #8699, #13746 ),
 ( #4466, #18308, #23198, #23361, #18617, #28063 ),
 ( #1800, #11080, #30272, #16256, #6353, #11391 ),
 ( #15951, #1641, #30592, #30738, #28215, #23518 ),
 ( #11229, #13907, #20835, #28379, #6819, #23669 ),
 ( #16415, #4609, #9330, #23044, #26023, #8860 ),
 ( #14065, #2103, #6978, #16567, #11696, #26173 ) ),
 .UNSPECIFIED., .F., .F., .T. ) 
 B_SPLINE_SURFACE_WITH_KNOTS ( ( 6, 3, 3, 3, 3, 3, 3, 3, 3, 3, 3, 3, 3, 3, 3, 3, 3, 3, 3, 3, 3, 3, 3, 3, 3, 6 ),
 ( 6, 6 ),
 ( 0.000000000000000000, 11.49596029219999949, 23.35952330949999833, 35.23214498380000492, 46.71570041140000029, 58.48118637179999979, 70.16173614769999745, 81.99711437660000968, 93.33986353700001359, 104.8204913790000035, 116.3828353250000021, 128.2105526469999859, 137.7231253239999944, 147.2120576640000138, 156.6774103699999898, 168.4624398839999913, 180.2684855139999911, 192.1268167670000082, 203.5147100690000173, 215.0810220189999882, 226.8492753339999979, 238.4740513719999910, 250.2932425120000062, 262.1023078380000015, 273.4723917590000042, 284.7968047250000154 ),
 ( 0.000000000000000000, 6.674405137519999975 ),
 .UNSPECIFIED. ) 
 GEOMETRIC_REPRESENTATION_ITEM ( )  RATIONAL_B_SPLINE_SURFACE ( (
 ( 1.000000000000000000, 0.5999999999999999778, 0.4000000000000000222, 0.2999999999999999889, 0.2500000000000000000, 0.2500000000000000000),
 ( 1.000000000000000000, 0.5999999999999999778, 0.4000000000000000222, 0.2999999999999999889, 0.2500000000000000000, 0.2500000000000000000),
 ( 1.000000000000000000, 0.5999999999999999778, 0.4000000000000000222, 0.2999999999999999889, 0.2500000000000000000, 0.2500000000000000000),
 ( 1.000000000000000000, 0.5999999999999999778, 0.4000000000000000222, 0.2999999999999999889, 0.2500000000000000000, 0.2500000000000000000),
 ( 1.000000000000000000, 0.5999999999999999778, 0.4000000000000000222, 0.2999999999999999889, 0.2500000000000000000, 0.2500000000000000000),
 ( 1.000000000000000000, 0.5999999999999999778, 0.4000000000000000222, 0.2999999999999999889, 0.2500000000000000000, 0.2500000000000000000),
 ( 1.000000000000000000, 0.5999999999999999778, 0.4000000000000000222, 0.2999999999999999889, 0.2500000000000000000, 0.2500000000000000000),
 ( 1.000000000000000000, 0.5999999999999999778, 0.4000000000000000222, 0.2999999999999999889, 0.2500000000000000000, 0.2500000000000000000),
 ( 1.000000000000000000, 0.5999999999999999778, 0.4000000000000000222, 0.2999999999999999889, 0.2500000000000000000, 0.2500000000000000000),
 ( 1.000000000000000000, 0.5999999999999999778, 0.4000000000000000222, 0.2999999999999999889, 0.2500000000000000000, 0.2500000000000000000),
 ( 1.000000000000000000, 0.5999999999999999778, 0.4000000000000000222, 0.2999999999999999889, 0.2500000000000000000, 0.2500000000000000000),
 ( 1.000000000000000000, 0.5999999999999999778, 0.4000000000000000222, 0.2999999999999999889, 0.2500000000000000000, 0.2500000000000000000),
 ( 1.000000000000000000, 0.5999999999999999778, 0.4000000000000000222, 0.2999999999999999889, 0.2500000000000000000, 0.2500000000000000000),
 ( 1.000000000000000000, 0.5999999999999999778, 0.4000000000000000222, 0.2999999999999999889, 0.2500000000000000000, 0.2500000000000000000),
 ( 1.000000000000000000, 0.5999999999999999778, 0.4000000000000000222, 0.2999999999999999889, 0.2500000000000000000, 0.2500000000000000000),
 ( 1.000000000000000000, 0.5999999999999999778, 0.4000000000000000222, 0.2999999999999999889, 0.2500000000000000000, 0.2500000000000000000),
 ( 1.000000000000000000, 0.5999999999999999778, 0.4000000000000000222, 0.2999999999999999889, 0.2500000000000000000, 0.2500000000000000000),
 ( 1.000000000000000000, 0.5999999999999999778, 0.4000000000000000222, 0.2999999999999999889, 0.2500000000000000000, 0.2500000000000000000),
 ( 1.000000000000000000, 0.5999999999999999778, 0.4000000000000000222, 0.2999999999999999889, 0.2500000000000000000, 0.2500000000000000000),
 ( 1.000000000000000000, 0.5999999999999999778, 0.4000000000000000222, 0.2999999999999999889, 0.2500000000000000000, 0.2500000000000000000),
 ( 1.000000000000000000, 0.5999999999999999778, 0.4000000000000000222, 0.2999999999999999889, 0.2500000000000000000, 0.2500000000000000000),
 ( 1.000000000000000000, 0.5999999999999999778, 0.4000000000000000222, 0.2999999999999999889, 0.2500000000000000000, 0.2500000000000000000),
 ( 1.000000000000000000, 0.5999999999999999778, 0.4000000000000000222, 0.2999999999999999889, 0.2500000000000000000, 0.2500000000000000000),
 ( 1.000000000000000000, 0.5999999999999999778, 0.4000000000000000222, 0.2999999999999999889, 0.2500000000000000000, 0.2500000000000000000),
 ( 1.000000000000000000, 0.5999999999999999778, 0.4000000000000000222, 0.2999999999999999889, 0.2500000000000000000, 0.2500000000000000000),
 ( 1.000000000000000000, 0.5999999999999999778, 0.4000000000000000222, 0.2999999999999999889, 0.2500000000000000000, 0.2500000000000000000),
 ( 1.000000000000000000, 0.5999999999999999778, 0.4000000000000000222, 0.2999999999999999889, 0.2500000000000000000, 0.2500000000000000000),
 ( 1.000000000000000000, 0.5999999999999999778, 0.4000000000000000222, 0.2999999999999999889, 0.2500000000000000000, 0.2500000000000000000),
 ( 1.000000000000000000, 0.5999999999999999778, 0.4000000000000000222, 0.2999999999999999889, 0.2500000000000000000, 0.2500000000000000000),
 ( 1.000000000000000000, 0.5999999999999999778, 0.4000000000000000222, 0.2999999999999999889, 0.2500000000000000000, 0.2500000000000000000),
 ( 1.000000000000000000, 0.5999999999999999778, 0.4000000000000000222, 0.2999999999999999889, 0.2500000000000000000, 0.2500000000000000000),
 ( 1.000000000000000000, 0.5999999999999999778, 0.4000000000000000222, 0.2999999999999999889, 0.2500000000000000000, 0.2500000000000000000),
 ( 1.000000000000000000, 0.5999999999999999778, 0.4000000000000000222, 0.2999999999999999889, 0.2500000000000000000, 0.2500000000000000000),
 ( 1.000000000000000000, 0.5999999999999999778, 0.4000000000000000222, 0.2999999999999999889, 0.2500000000000000000, 0.2500000000000000000),
 ( 1.000000000000000000, 0.5999999999999999778, 0.4000000000000000222, 0.2999999999999999889, 0.2500000000000000000, 0.2500000000000000000),
 ( 1.000000000000000000, 0.5999999999999999778, 0.4000000000000000222, 0.2999999999999999889, 0.2500000000000000000, 0.2500000000000000000),
 ( 1.000000000000000000, 0.5999999999999999778, 0.4000000000000000222, 0.2999999999999999889, 0.2500000000000000000, 0.2500000000000000000),
 ( 1.000000000000000000, 0.5999999999999999778, 0.4000000000000000222, 0.2999999999999999889, 0.2500000000000000000, 0.2500000000000000000),
 ( 1.000000000000000000, 0.5999999999999999778, 0.4000000000000000222, 0.2999999999999999889, 0.2500000000000000000, 0.2500000000000000000),
 ( 1.000000000000000000, 0.5999999999999999778, 0.4000000000000000222, 0.2999999999999999889, 0.2500000000000000000, 0.2500000000000000000),
 ( 1.000000000000000000, 0.5999999999999999778, 0.4000000000000000222, 0.2999999999999999889, 0.2500000000000000000, 0.2500000000000000000),
 ( 1.000000000000000000, 0.5999999999999999778, 0.4000000000000000222, 0.2999999999999999889, 0.2500000000000000000, 0.2500000000000000000),
 ( 1.000000000000000000, 0.5999999999999999778, 0.4000000000000000222, 0.2999999999999999889, 0.2500000000000000000, 0.2500000000000000000),
 ( 1.000000000000000000, 0.5999999999999999778, 0.4000000000000000222, 0.2999999999999999889, 0.2500000000000000000, 0.2500000000000000000),
 ( 1.000000000000000000, 0.5999999999999999778, 0.4000000000000000222, 0.2999999999999999889, 0.2500000000000000000, 0.2500000000000000000),
 ( 1.000000000000000000, 0.5999999999999999778, 0.4000000000000000222, 0.2999999999999999889, 0.2500000000000000000, 0.2500000000000000000),
 ( 1.000000000000000000, 0.5999999999999999778, 0.4000000000000000222, 0.2999999999999999889, 0.2500000000000000000, 0.2500000000000000000),
 ( 1.000000000000000000, 0.5999999999999999778, 0.4000000000000000222, 0.2999999999999999889, 0.2500000000000000000, 0.2500000000000000000),
 ( 1.000000000000000000, 0.5999999999999999778, 0.4000000000000000222, 0.2999999999999999889, 0.2500000000000000000, 0.2500000000000000000),
 ( 1.000000000000000000, 0.5999999999999999778, 0.4000000000000000222, 0.2999999999999999889, 0.2500000000000000000, 0.2500000000000000000),
 ( 1.000000000000000000, 0.5999999999999999778, 0.4000000000000000222, 0.2999999999999999889, 0.2500000000000000000, 0.2500000000000000000),
 ( 1.000000000000000000, 0.5999999999999999778, 0.4000000000000000222, 0.2999999999999999889, 0.2500000000000000000, 0.2500000000000000000),
 ( 1.000000000000000000, 0.5999999999999999778, 0.4000000000000000222, 0.2999999999999999889, 0.2500000000000000000, 0.2500000000000000000),
 ( 1.000000000000000000, 0.5999999999999999778, 0.4000000000000000222, 0.2999999999999999889, 0.2500000000000000000, 0.2500000000000000000),
 ( 1.000000000000000000, 0.5999999999999999778, 0.4000000000000000222, 0.2999999999999999889, 0.2500000000000000000, 0.2500000000000000000),
 ( 1.000000000000000000, 0.5999999999999999778, 0.4000000000000000222, 0.2999999999999999889, 0.2500000000000000000, 0.2500000000000000000),
 ( 1.000000000000000000, 0.5999999999999999778, 0.4000000000000000222, 0.2999999999999999889, 0.2500000000000000000, 0.2500000000000000000),
 ( 1.000000000000000000, 0.5999999999999999778, 0.4000000000000000222, 0.2999999999999999889, 0.2500000000000000000, 0.2500000000000000000),
 ( 1.000000000000000000, 0.5999999999999999778, 0.4000000000000000222, 0.2999999999999999889, 0.2500000000000000000, 0.2500000000000000000),
 ( 1.000000000000000000, 0.5999999999999999778, 0.4000000000000000222, 0.2999999999999999889, 0.2500000000000000000, 0.2500000000000000000),
 ( 1.000000000000000000, 0.5999999999999999778, 0.4000000000000000222, 0.2999999999999999889, 0.2500000000000000000, 0.2500000000000000000),
 ( 1.000000000000000000, 0.5999999999999999778, 0.4000000000000000222, 0.2999999999999999889, 0.2500000000000000000, 0.2500000000000000000),
 ( 1.000000000000000000, 0.5999999999999999778, 0.4000000000000000222, 0.2999999999999999889, 0.2500000000000000000, 0.2500000000000000000),
 ( 1.000000000000000000, 0.5999999999999999778, 0.4000000000000000222, 0.2999999999999999889, 0.2500000000000000000, 0.2500000000000000000),
 ( 1.000000000000000000, 0.5999999999999999778, 0.4000000000000000222, 0.2999999999999999889, 0.2500000000000000000, 0.2500000000000000000),
 ( 1.000000000000000000, 0.5999999999999999778, 0.4000000000000000222, 0.2999999999999999889, 0.2500000000000000000, 0.2500000000000000000),
 ( 1.000000000000000000, 0.5999999999999999778, 0.4000000000000000222, 0.2999999999999999889, 0.2500000000000000000, 0.2500000000000000000),
 ( 1.000000000000000000, 0.5999999999999999778, 0.4000000000000000222, 0.2999999999999999889, 0.2500000000000000000, 0.2500000000000000000),
 ( 1.000000000000000000, 0.5999999999999999778, 0.4000000000000000222, 0.2999999999999999889, 0.2500000000000000000, 0.2500000000000000000),
 ( 1.000000000000000000, 0.5999999999999999778, 0.4000000000000000222, 0.2999999999999999889, 0.2500000000000000000, 0.2500000000000000000),
 ( 1.000000000000000000, 0.5999999999999999778, 0.4000000000000000222, 0.2999999999999999889, 0.2500000000000000000, 0.2500000000000000000),
 ( 1.000000000000000000, 0.5999999999999999778, 0.4000000000000000222, 0.2999999999999999889, 0.2500000000000000000, 0.2500000000000000000),
 ( 1.000000000000000000, 0.5999999999999999778, 0.4000000000000000222, 0.2999999999999999889, 0.2500000000000000000, 0.2500000000000000000),
 ( 1.000000000000000000, 0.5999999999999999778, 0.4000000000000000222, 0.2999999999999999889, 0.2500000000000000000, 0.2500000000000000000),
 ( 1.000000000000000000, 0.5999999999999999778, 0.4000000000000000222, 0.2999999999999999889, 0.2500000000000000000, 0.2500000000000000000),
 ( 1.000000000000000000, 0.5999999999999999778, 0.4000000000000000222, 0.2999999999999999889, 0.2500000000000000000, 0.2500000000000000000),
 ( 1.000000000000000000, 0.5999999999999999778, 0.4000000000000000222, 0.2999999999999999889, 0.2500000000000000000, 0.2500000000000000000),
 ( 1.000000000000000000, 0.5999999999999999778, 0.4000000000000000222, 0.2999999999999999889, 0.2500000000000000000, 0.2500000000000000000) ) ) 
 REPRESENTATION_ITEM ( '' )  SURFACE ( )  );
#24591 = CARTESIAN_POINT ( 'NONE',  ( -23.96314403019941608, -14.09350462245096125, 6.073177660868579686 ) ) ;
#24592 = DIRECTION ( 'NONE',  ( -6.386904893851405129E-12, -0.3322662713817149949, 0.9431856258987901809 ) ) ;
#24593 = CARTESIAN_POINT ( 'NONE',  ( -10.70000000000073470, -25.58868802739137038, -25.72767439687939728 ) ) ;
#24594 = ORIENTED_EDGE ( 'NONE', *, *, #8484, .T. ) ;
#24595 = EDGE_CURVE ( 'NONE', #22078, #1634, #22836, .T. ) ;
#24596 = CARTESIAN_POINT ( 'NONE',  ( 27.06563795990000187, -3.314475221579999886E-15, 41.94026860139999258 ) ) ;
#24597 = CARTESIAN_POINT ( 'NONE',  ( -2.554946692801202346, -3.999086378171832212, -20.77141267860000795 ) ) ;
#24598 = DIRECTION ( 'NONE',  ( 0.8783853955697265015, -0.4779530278697008971, 2.498001805408841824E-13 ) ) ;
#24599 = CARTESIAN_POINT ( 'NONE',  ( 10.69999999999999929, -25.00000000000000000, -26.16393202249999916 ) ) ;
#24600 = LINE ( 'NONE', #12788, #10667 ) ;
#24601 = FACE_OUTER_BOUND ( 'NONE', #30842, .T. ) ;
#24602 = DIRECTION ( 'NONE',  ( -2.966217977826874882E-25, -1.000000000000000000, 2.257145581549900232E-12 ) ) ;
#24603 = ADVANCED_FACE ( 'NONE', ( #2397 ), #29125, .T. ) ;
#24604 = CIRCLE ( 'NONE', #11037, 28.50000000000000000 ) ;
#24605 = DIRECTION ( 'NONE',  ( -0.9316362575375349842, 0.3633921898465292122, -0.000000000000000000 ) ) ;
#24606 = CARTESIAN_POINT ( 'NONE',  ( 18.48841959639999644, 20.72769515089999715, 229.2930775960000176 ) ) ;
#24607 = CARTESIAN_POINT ( 'NONE',  ( -7.999999999721752353, -29.89895010230364392, -27.53380090445090289 ) ) ;
#24608 = VERTEX_POINT ( 'NONE', #14513 ) ;
#24609 = CARTESIAN_POINT ( 'NONE',  ( -3.882843611328785638, 4.424263292013742799, -53.18587006832499497 ) ) ;
#24610 = CARTESIAN_POINT ( 'NONE',  ( -12.34929264640405577, -25.24897882093459245, -23.63770812723453574 ) ) ;
#24611 = CARTESIAN_POINT ( 'NONE',  ( -21.38751961657293066, 17.02472927140214054, 0.000000000000000000 ) ) ;
#24612 = CARTESIAN_POINT ( 'NONE',  ( -4.296780221824271884, 1.072976733195472931, -68.10000000002501963 ) ) ;
#24613 = EDGE_CURVE ( 'NONE', #30479, #25858, #30890, .T. ) ;
#24614 = ORIENTED_EDGE ( 'NONE', *, *, #30256, .T. ) ;
#24615 = CARTESIAN_POINT ( 'NONE',  ( -3.813212237922182002, -1.735188837432927178, -96.08088653434137427 ) ) ;
#24616 = ORIENTED_EDGE ( 'NONE', *, *, #24982, .F. ) ;
#24617 = CARTESIAN_POINT ( 'NONE',  ( 0.000000000000000000, 0.000000000000000000, 229.6412452697800006 ) ) ;
#24618 = DIRECTION ( 'NONE',  ( 0.3633921898465289901, 0.9316362575375348731, 2.168404344971007290E-15 ) ) ;
#24619 = VERTEX_POINT ( 'NONE', #21595 ) ;
#24620 = CARTESIAN_POINT ( 'NONE',  ( 3.430850994441077439, -5.010772104901466406, -27.13292313650000764 ) ) ;
#24621 = DIRECTION ( 'NONE',  ( -0.3090169943750401549, -0.9510565162951233331, 0.000000000000000000 ) ) ;
#24622 = PRODUCT_DEFINITION ( 'UNKNOWN', '', #5308, #11588 ) ;
#24623 = CARTESIAN_POINT ( 'NONE',  ( -27.55801272791059731, -0.5014288284349446290, -0.5592437529999827461 ) ) ;
#24624 = CARTESIAN_POINT ( 'NONE',  ( 18.95046173579999760, -18.95046173579999760, 115.0000000000000000 ) ) ;
#24625 = CARTESIAN_POINT ( 'NONE',  ( 8.700000000229927366, -28.07050130669910715, -25.59757157921452020 ) ) ;
#24626 = ORIENTED_EDGE ( 'NONE', *, *, #30030, .T. ) ;
#24627 = DIRECTION ( 'NONE',  ( 0.000000000000000000, -0.3420201433259318913, 0.9396926207858126157 ) ) ;
#24628 = EDGE_CURVE ( 'NONE', #7590, #26174, #28365, .T. ) ;
#24629 = DIRECTION ( 'NONE',  ( 0.000000000000000000, 0.000000000000000000, -1.000000000000000000 ) ) ;
#24630 = ORIENTED_EDGE ( 'NONE', *, *, #17325, .F. ) ;
#24631 = CARTESIAN_POINT ( 'NONE',  ( 9.738910687886868089, -24.96785170200598358, 36.78285841123148003 ) ) ;
#24632 = CARTESIAN_POINT ( 'NONE',  ( 8.700000000244115128, -26.99999999999395328, -28.39999999994493862 ) ) ;
#24633 = CARTESIAN_POINT ( 'NONE',  ( -12.05432023370000039, -0.5681652772719999467, 231.9999989789999972 ) ) ;
#24634 = PLANE ( 'NONE',  #13257 ) ;
#24635 = CARTESIAN_POINT ( 'NONE',  ( 23.50667118420000179, -14.84174322970000048, 225.0000014190000002 ) ) ;
#24636 = CARTESIAN_POINT ( 'NONE',  ( 1.484924240490000047, -1.484924240490000047, 227.6412452697800006 ) ) ;
#24637 = B_SPLINE_CURVE_WITH_KNOTS ( 'NONE', 5,
 ( #26935, #5370, #29281, #7723, #14978, #24575, #3009, #12602, #19858 ),
 .UNSPECIFIED., .F., .F.,
 ( 6, 3, 6 ),
 ( 0.000000000000000000, 2.405120302929999898, 3.339306056309999438 ),
 .UNSPECIFIED. ) ;
#24638 = CIRCLE ( 'NONE', #13954, 27.50000000000000000 ) ;
#24639 = CARTESIAN_POINT ( 'NONE',  ( 3.119449978080022667, -2.770394852667431351, -0.6999999999999992895 ) ) ;
#24640 = CARTESIAN_POINT ( 'NONE',  ( -24.45890872495081680, -14.61494978185785421, -0.6999999999999784173 ) ) ;
#24641 = CARTESIAN_POINT ( 'NONE',  ( -26.80000000000000071, 4.518892556989999143, 230.0000000000000000 ) ) ;
#24642 = CARTESIAN_POINT ( 'NONE',  ( -10.69999999999999929, -29.12132034360000077, -30.52132034359999935 ) ) ;
#24643 = CARTESIAN_POINT ( 'NONE',  ( -7.999999999677900320, -14.01599944959732369, -33.92178631050306592 ) ) ;
#24644 = EDGE_CURVE ( 'NONE', #8060, #21911, #17322, .T. ) ;
#24646 = CARTESIAN_POINT ( 'NONE',  ( -19.81582138730396636, -18.05844329259051051, 93.21714158843887787 ) ) ;
#24645 = APPLICATION_CONTEXT ( 'automotive_design' ) ;
#24647 = CARTESIAN_POINT ( 'NONE',  ( 0.5184513693225726305, -28.49550581263314086, 6.099998581000020792 ) ) ;
#24648 = VERTEX_POINT ( 'NONE', #16859 ) ;
#24649 = AXIS2_PLACEMENT_3D ( 'NONE', #27551, #6733, #7048 ) ;
#24650 = DIRECTION ( 'NONE',  ( 1.000000000000000000, 0.000000000000000000, 0.000000000000000000 ) ) ;
#24651 = DIRECTION ( 'NONE',  ( 0.000000000000000000, -0.3420201433259318913, 0.9396926207858126157 ) ) ;
#24652 = ADVANCED_FACE ( 'NONE', ( #17017 ), #3743, .F. ) ;
#24653 = CARTESIAN_POINT ( 'NONE',  ( 1.094823181362614140, 5.872682718251108547, -63.42744533522500205 ) ) ;
#24654 = ORIENTED_EDGE ( 'NONE', *, *, #26517, .F. ) ;
#24655 = ORIENTED_EDGE ( 'NONE', *, *, #24317, .T. ) ;
#24656 = CARTESIAN_POINT ( 'NONE',  ( -4.499842235593497719, -29.81936866046843093, 0.000000000000000000 ) ) ;
#24657 = VERTEX_POINT ( 'NONE', #5057 ) ;
#24658 = ORIENTED_EDGE ( 'NONE', *, *, #4381, .F. ) ;
#24659 = CARTESIAN_POINT ( 'NONE',  ( 9.999999999978641085, -28.84364016088975546, -30.79900052649311348 ) ) ;
#24660 = CARTESIAN_POINT ( 'NONE',  ( -23.73463268736954035, -12.44713172136066248, 225.2180667906550298 ) ) ;
#24661 = DIRECTION ( 'NONE',  ( 0.000000000000000000, 0.000000000000000000, -1.000000000000000000 ) ) ;
#24662 = B_SPLINE_CURVE_WITH_KNOTS ( 'NONE', 3,
 ( #9178, #16267, #13917, #14076, #18780, #23528, #6202, #11557, #15804, #28389 ),
 .UNSPECIFIED., .F., .F.,
 ( 4, 2, 2, 2, 4 ),
 ( 0.000000000000000000, 0.2500000000000001665, 0.5000000000000001110, 0.7500000000000000000, 1.000000000000000000 ),
 .UNSPECIFIED. ) ;
#24663 = CARTESIAN_POINT ( 'NONE',  ( 4.414854054520000126, 11.17832006019999902, 231.9999991140000191 ) ) ;
#24664 = EDGE_CURVE ( 'NONE', #15209, #18136, #12297, .T. ) ;
#24665 = CARTESIAN_POINT ( 'NONE',  ( 24.83827472153076599, -12.48687851163286133, 4.999998581000003384 ) ) ;
#24666 = FACE_BOUND ( 'NONE', #14525, .T. ) ;
#24667 = ORIENTED_EDGE ( 'NONE', *, *, #23697, .T. ) ;
#24668 = CARTESIAN_POINT ( 'NONE',  ( 2.753318369310237657, -3.444419153943022671, -44.10000000002499121 ) ) ;
#24669 = LINE ( 'NONE', #29227, #29349 ) ;
#24670 = EDGE_CURVE ( 'NONE', #12454, #13996, #2852, .T. ) ;
#24671 = TOROIDAL_SURFACE ( 'NONE', #8078, 24.50000000000000000, 3.200000000000000178 ) ;
#24672 = CARTESIAN_POINT ( 'NONE',  ( -4.047971700345533996, -2.476765951014430200, -22.84549200639999711 ) ) ;
#24673 = CARTESIAN_POINT ( 'NONE',  ( 23.73992238019999945, -12.43607998449999918, 5.000000000000000000 ) ) ;
#24674 = DIRECTION ( 'NONE',  ( -0.4353787270609792981, -0.9002473904559574747, 0.000000000000000000 ) ) ;
#24675 = CARTESIAN_POINT ( 'NONE',  ( -27.63177356800000339, 3.383804547869999678E-15, 187.3605236429999934 ) ) ;
#24676 = DIRECTION ( 'NONE',  ( 1.000000000000000000, 0.000000000000000000, 0.000000000000000000 ) ) ;
#24677 = CARTESIAN_POINT ( 'NONE',  ( -3.130203125555106158, 5.106303518385050033, -44.57531229042499632 ) ) ;
#24678 = EDGE_CURVE ( 'NONE', #13797, #11577, #21301, .T. ) ;
#24679 = CARTESIAN_POINT ( 'NONE',  ( -9.499999999560001740, 21.70000000000000284, -60.10000000000000142 ) ) ;
#24680 = CARTESIAN_POINT ( 'NONE',  ( -0.2757844036473713900, 2.086681040193929082, 226.6412452697800290 ) ) ;
#24681 = CARTESIAN_POINT ( 'NONE',  ( -19.55772779817724683, 19.99999847704128797, 230.2366316984319781 ) ) ;
#24682 = CARTESIAN_POINT ( 'NONE',  ( -27.79999999980000069, 4.687507935210000198, 229.0000000000000000 ) ) ;
#24683 = CARTESIAN_POINT ( 'NONE',  ( 9.481612630793602392, -25.06681236668577384, 25.90123088588473976 ) ) ;
#24684 = VERTEX_POINT ( 'NONE', #44 ) ;
#24685 = CARTESIAN_POINT ( 'NONE',  ( -3.357682761866084498, 3.860481585313637609, -29.52478588869999854 ) ) ;
#24686 = ORIENTED_EDGE ( 'NONE', *, *, #30446, .T. ) ;
#24687 = CARTESIAN_POINT ( 'NONE',  ( -8.699999998994179862, -29.73863906514459643, -27.17531388891805477 ) ) ;
#24688 = CARTESIAN_POINT ( 'NONE',  ( 2.776548632478544665, -3.583402058917912747, -52.90430438132499802 ) ) ;
#24689 = ORIENTED_EDGE ( 'NONE', *, *, #4045, .F. ) ;
#24690 = ORIENTED_EDGE ( 'NONE', *, *, #3871, .T. ) ;
#24691 = DIRECTION ( 'NONE',  ( 1.000000000000000000, 0.000000000000000000, 0.000000000000000000 ) ) ;
#24692 = VECTOR ( 'NONE', #28661, 1000.000000000000000 ) ;
#24693 = ORIENTED_EDGE ( 'NONE', *, *, #16916, .T. ) ;
#24694 = B_SPLINE_CURVE_WITH_KNOTS ( 'NONE', 5,
 ( #3377, #12982, #29190, #2776, #12367, #21976, #6527, #3857, #27932 ),
 .UNSPECIFIED., .F., .F.,
 ( 6, 3, 6 ),
 ( 0.000000000000000000, 0.7281981308589999813, 1.224410036190000106 ),
 .UNSPECIFIED. ) ;
#24695 = VERTEX_POINT ( 'NONE', #9469 ) ;
#24696 = CARTESIAN_POINT ( 'NONE',  ( 16.37473331892315542, -8.236461616552139375, 0.000000000000000000 ) ) ;
#24697 = CARTESIAN_POINT ( 'NONE',  ( -17.89938223473397017, 10.69263420681399346, -0.6999999999999784173 ) ) ;
#24698 = CARTESIAN_POINT ( 'NONE',  ( 10.69999999999999929, -25.00000000000000000, -26.16393202249999916 ) ) ;
#24699 = CARTESIAN_POINT ( 'NONE',  ( -1.841797396446221091, -26.73663745407121795, 210.0000000000000284 ) ) ;
#24700 = CARTESIAN_POINT ( 'NONE',  ( 10.14902473063354194, -26.01926976387845158, 192.0603150150000147 ) ) ;
#24701 = EDGE_CURVE ( 'NONE', #2338, #20042, #303, .T. ) ;
#24702 = CARTESIAN_POINT ( 'NONE',  ( -4.895789606679002759, -1.770905548711505295, -0.6999999999999992895 ) ) ;
#24703 = CARTESIAN_POINT ( 'NONE',  ( -10.69999999989999928, -30.49251257979999963, -21.04205368470000082 ) ) ;
#24704 = CARTESIAN_POINT ( 'NONE',  ( -22.36193249936582816, 17.71394520520996707, 6.000000042999998229 ) ) ;
#24705 = CARTESIAN_POINT ( 'NONE',  ( -5.527020701484460119, 0.1640065206915941320, -14.18304957890000040 ) ) ;
#24706 = CARTESIAN_POINT ( 'NONE',  ( -5.984522419796141079, -1.167122196978044535, -31.09652066320001040 ) ) ;
#24707 = CARTESIAN_POINT ( 'NONE',  ( 2.125375073177956597, -3.761816432237487628, -70.24751875706795090 ) ) ;
#24708 = EDGE_CURVE ( 'NONE', #26831, #22535, #661, .T. ) ;
#24709 = EDGE_CURVE ( 'NONE', #14079, #24098, #14564, .T. ) ;
#24710 = CARTESIAN_POINT ( 'NONE',  ( 24.90302311548996883, -13.86047864964742793, 6.098655051000018368 ) ) ;
#24711 = CARTESIAN_POINT ( 'NONE',  ( -17.49999999969999820, -32.00000000000000000, -25.51324865424999899 ) ) ;
#24712 = LINE ( 'NONE', #8164, #23200 ) ;
#24713 = CARTESIAN_POINT ( 'NONE',  ( -1.419173393160000125E-06, -27.80022181310000207, 226.1000014189999945 ) ) ;
#24714 = CARTESIAN_POINT ( 'NONE',  ( -4.339197174995631734, 0.6278332542688225271, -34.25783976329999092 ) ) ;
#24715 = VECTOR ( 'NONE', #29895, 1000.000000000000000 ) ;
#24716 = CARTESIAN_POINT ( 'NONE',  ( -28.49528339128749366, -0.5184828350247674411, 1.000000000000000888 ) ) ;
#24717 = CARTESIAN_POINT ( 'NONE',  ( 14.84775334008999970, -24.60220466919999893, -24.01086508770000094 ) ) ;
#24718 = CARTESIAN_POINT ( 'NONE',  ( 1.089891362619999970, -28.47934442809999922, 224.6898179359999972 ) ) ;
#24719 = VERTEX_POINT ( 'NONE', #19994 ) ;
#24720 = VECTOR ( 'NONE', #1491, 1000.000000000000227 ) ;
#24721 = DIRECTION ( 'NONE',  ( 5.962915006522623408E-16, 0.4383711467890811231, 0.8987940462991652613 ) ) ;
#24722 = CARTESIAN_POINT ( 'NONE',  ( 11.54917764160000004, 19.99999999999999645, -0.6999999992999966780 ) ) ;
#24723 = ORIENTED_EDGE ( 'NONE', *, *, #2240, .T. ) ;
#24724 = CARTESIAN_POINT ( 'NONE',  ( 18.63941909573550859, 10.97998838177520931, 0.5194763363741546902 ) ) ;
#24725 = CARTESIAN_POINT ( 'NONE',  ( -1.092383471258445704, -3.930924299782534437, -38.89973510835866222 ) ) ;
#24726 = ORIENTED_EDGE ( 'NONE', *, *, #20654, .F. ) ;
#24727 = CARTESIAN_POINT ( 'NONE',  ( -9.506387914194311506, -25.80482363264563972, 25.14863730271530073 ) ) ;
#24728 = ORIENTED_EDGE ( 'NONE', *, *, #14280, .T. ) ;
#24729 = ORIENTED_EDGE ( 'NONE', *, *, #17346, .T. ) ;
#24730 = ORIENTED_EDGE ( 'NONE', *, *, #5915, .T. ) ;
#24731 = DIRECTION ( 'NONE',  ( 0.000000000000000000, 0.000000000000000000, 1.000000000000000000 ) ) ;
#24732 = VECTOR ( 'NONE', #19630, 1000.000000000000000 ) ;
#24733 = CIRCLE ( 'NONE', #19211, 0.9999999999999991118 ) ;
#24734 = EDGE_CURVE ( 'NONE', #4633, #19859, #25024, .T. ) ;
#24735 = CARTESIAN_POINT ( 'NONE',  ( -16.17397428794474479, 11.89215903497504456, -0.6999999999999783062 ) ) ;
#24736 = CARTESIAN_POINT ( 'NONE',  ( 16.06409288148108416, -8.873734595567666972, -0.6999999999999784173 ) ) ;
#24737 = EDGE_CURVE ( 'NONE', #27983, #22821, #10557, .T. ) ;
#24738 = CARTESIAN_POINT ( 'NONE',  ( 4.276011752470107119, -102.7755780389287281, 17.20706796827408169 ) ) ;
#24739 = CARTESIAN_POINT ( 'NONE',  ( -19.80526803560000104, 19.50877411510000314, 227.0000000000000000 ) ) ;
#24740 = B_SPLINE_CURVE_WITH_KNOTS ( 'NONE', 3,
 ( #5237, #9538, #14265, #19135, #17349, #28581 ),
 .UNSPECIFIED., .F., .F.,
 ( 4, 2, 4 ),
 ( 0.000000000000000000, 0.5000000000000000000, 1.000000000000000000 ),
 .UNSPECIFIED. ) ;
#24741 = PRODUCT ( 'Drive Spring', 'Drive Spring', '', ( #25315 ) ) ;
#24742 = CARTESIAN_POINT ( 'NONE',  ( -24.15628151204887786, -13.75958218676210087, 5.886532584766007936 ) ) ;
#24743 = CARTESIAN_POINT ( 'NONE',  ( 7.554893095320836416, -26.44255681430371041, 207.8813784578385935 ) ) ;
#24744 = CARTESIAN_POINT ( 'NONE',  ( 24.48837202150000181, -14.58033361329999877, 223.9575292099999899 ) ) ;
#24745 = CARTESIAN_POINT ( 'NONE',  ( 8.903108651239925564, -22.82508830966962421, 140.0000000000000000 ) ) ;
#24746 = CARTESIAN_POINT ( 'NONE',  ( 4.129834804009608007, 5.047645050193429128, -19.65622222229999849 ) ) ;
#24747 = CARTESIAN_POINT ( 'NONE',  ( -0.1472904996853126869, -28.50022958377793358, 223.9000014189999774 ) ) ;
#24748 = AXIS2_PLACEMENT_3D ( 'NONE', #10638, #20229, #29823 ) ;
#24749 = CARTESIAN_POINT ( 'NONE',  ( -6.000000000000000000, -29.61802109059427934, -80.72258539628914775 ) ) ;
#24750 = CARTESIAN_POINT ( 'NONE',  ( 23.47117976016943430, -14.33053685725933235, 225.8804910026547077 ) ) ;
#24751 = CARTESIAN_POINT ( 'NONE',  ( -18.97091445539999910, 21.26865671770000077, 229.2404163060000144 ) ) ;
#24752 = CARTESIAN_POINT ( 'NONE',  ( 3.458129700889219116, -0.5397582531354573332, -88.52261276322501260 ) ) ;
#24753 = B_SPLINE_CURVE_WITH_KNOTS ( 'NONE', 1,
 ( #4752, #16231 ),
 .UNSPECIFIED., .F., .F.,
 ( 2, 2 ),
 ( -0.7031447686210000603, 1.118726812310288921E-05 ),
 .UNSPECIFIED. ) ;
#24754 = CARTESIAN_POINT ( 'NONE',  ( -10.69999999999999929, -26.66060153629999974, -31.39999999999999858 ) ) ;
#24755 = CARTESIAN_POINT ( 'NONE',  ( 21.92823313370000093, 17.58202518589999741, 229.4485716779999791 ) ) ;
#24756 = CARTESIAN_POINT ( 'NONE',  ( 2.607517555921732288, -3.483231422657013354, -39.11808951420159275 ) ) ;
#24757 = ORIENTED_EDGE ( 'NONE', *, *, #3020, .F. ) ;
#24758 = CARTESIAN_POINT ( 'NONE',  ( -0.06606756225350368661, 5.646037861211643083, -56.83818518972499589 ) ) ;
#24759 = CIRCLE ( 'NONE', #30283, 2.999999999999999556 ) ;
#24760 = DIRECTION ( 'NONE',  ( -1.000000000000000000, 5.687698019341907056E-16, -6.771501495046482653E-12 ) ) ;
#24761 = CARTESIAN_POINT ( 'NONE',  ( -0.1113126277073478027, 4.304903297084355707, -39.57881079973518723 ) ) ;
#24762 = CARTESIAN_POINT ( 'NONE',  ( -4.567159517660123846, 0.9507996984954559805, -68.10000000002500542 ) ) ;
#24763 = ADVANCED_FACE ( 'NONE', ( #19852 ), #17621, .F. ) ;
#24764 = EDGE_LOOP ( 'NONE', ( #22683, #5642, #3433, #20687 ) ) ;
#24765 = EDGE_CURVE ( 'NONE', #13324, #13818, #29533, .T. ) ;
#24766 = ORIENTED_EDGE ( 'NONE', *, *, #11389, .T. ) ;
#24767 = CARTESIAN_POINT ( 'NONE',  ( 1.423903527214286813, 1.992729285291204633, -95.48173244568418738 ) ) ;
#24768 = PRESENTATION_STYLE_ASSIGNMENT (( #15020 ) ) ;
#24769 = ORIENTED_EDGE ( 'NONE', *, *, #22408, .F. ) ;
#24770 = CARTESIAN_POINT ( 'NONE',  ( -10.93705068780284684, 21.00000000000141753, -55.10811849999506506 ) ) ;
#24771 = CARTESIAN_POINT ( 'NONE',  ( 23.23277125981546476, 15.26692728828886025, 5.104183903999998329 ) ) ;
#24772 = ORIENTED_EDGE ( 'NONE', *, *, #6620, .T. ) ;
#24773 = CARTESIAN_POINT ( 'NONE',  ( 3.705709820302785396, 4.685590126413917034, -63.15768011632499679 ) ) ;
#24774 = EDGE_CURVE ( 'NONE', #13449, #9797, #14163, .T. ) ;
#24775 = CARTESIAN_POINT ( 'NONE',  ( -13.61743661210000056, -27.34210457880000078, 229.7313233489999789 ) ) ;
#24776 = CARTESIAN_POINT ( 'NONE',  ( -28.49528339128749366, -0.5184828350247461248, 1.000000000000000888 ) ) ;
#24777 = CARTESIAN_POINT ( 'NONE',  ( 8.999999999540001738, 19.99999999999999645, -44.09999999970998630 ) ) ;
#24778 = B_SPLINE_CURVE_WITH_KNOTS ( 'NONE', 3,
 ( #4913, #6810, #2094, #16406 ),
 .UNSPECIFIED., .F., .F.,
 ( 4, 4 ),
 ( 0.000000000000000000, 1.000000000000000000 ),
 .UNSPECIFIED. ) ;
#24779 = DIRECTION ( 'NONE',  ( 0.2815395311419987556, 0.9595496299849963773, 0.000000000000000000 ) ) ;
#24780 = CARTESIAN_POINT ( 'NONE',  ( 8.999999999770000869, 21.70000000000000284, -48.10000000000000142 ) ) ;
#24781 = EDGE_LOOP ( 'NONE', ( #1246, #19912, #31080, #27088 ) ) ;
#24782 = CARTESIAN_POINT ( 'NONE',  ( 24.92013865993870425, -13.82966158318416738, 3.899998581000013509 ) ) ;
#24783 = CARTESIAN_POINT ( 'NONE',  ( -27.06563795990000187, 3.314475221589999487E-15, 91.94026860140000679 ) ) ;
#24784 = VERTEX_POINT ( 'NONE', #3456 ) ;
#24785 = CARTESIAN_POINT ( 'NONE',  ( 14.75521759265346589, -31.99975232932909108, -29.68276772680201603 ) ) ;
#24786 = ADVANCED_FACE ( 'NONE', ( #7869 ), #29590, .T. ) ;
#24787 = CARTESIAN_POINT ( 'NONE',  ( -24.31416968206321627, -13.47842985394946780, 5.506973469000003618 ) ) ;
#24788 = DIRECTION ( 'NONE',  ( 0.000000000000000000, 0.000000000000000000, 1.000000000000000000 ) ) ;
#24789 = B_SPLINE_CURVE_WITH_KNOTS ( 'NONE', 3,
 ( #11, #12103, #27165, #3239 ),
 .UNSPECIFIED., .F., .F.,
 ( 4, 4 ),
 ( -0.5999999999999999778, 0.000000000000000000 ),
 .UNSPECIFIED. ) ;
#24790 = CARTESIAN_POINT ( 'NONE',  ( 18.82264457159015691, 10.97998838177520931, 0.05106179917585291356 ) ) ;
#24791 = CARTESIAN_POINT ( 'NONE',  ( 8.000000000645206555, -18.51472853907661786, -35.46135205997079254 ) ) ;
#24792 = CARTESIAN_POINT ( 'NONE',  ( -2.017871889752692383, -3.161030873707806332, -0.6999999999999992895 ) ) ;
#24793 = CARTESIAN_POINT ( 'NONE',  ( 24.06826093652101051, -20.50742065841456707, 1.000000000000000888 ) ) ;
#24794 = CARTESIAN_POINT ( 'NONE',  ( -1.100000000000000089, -26.77741585740000119, 225.0000000000000000 ) ) ;
#24795 = EDGE_CURVE ( 'NONE', #12078, #16428, #23374, .T. ) ;
#24796 = AXIS2_PLACEMENT_3D ( 'NONE', #14843, #17342, #26785 ) ;
#24797 = DIRECTION ( 'NONE',  ( 0.000000000000000000, 0.000000000000000000, 1.000000000000000000 ) ) ;
#24798 = CARTESIAN_POINT ( 'NONE',  ( -7.999999999676562723, -13.83675952871606007, -34.17038780918873897 ) ) ;
#24799 = CARTESIAN_POINT ( 'NONE',  ( -2.898287520842993015, -26.64792758275492446, 20.04810862688719553 ) ) ;
#24800 = CARTESIAN_POINT ( 'NONE',  ( 7.366762595500000241E-07, 20.00000000000000000, 230.6999999999999886 ) ) ;
#24801 = ORIENTED_EDGE ( 'NONE', *, *, #23516, .T. ) ;
#24802 = CARTESIAN_POINT ( 'NONE',  ( 3.267430459712248325, 1.335589245137589254, -0.6999999999999783062 ) ) ;
#24803 =( NAMED_UNIT ( * ) SI_UNIT ( $, .STERADIAN. ) SOLID_ANGLE_UNIT ( ) );
#24804 = CARTESIAN_POINT ( 'NONE',  ( -7.999999999650326821, -14.98959907041461292, -37.84242876710612791 ) ) ;
#24805 = FACE_OUTER_BOUND ( 'NONE', #7538, .T. ) ;
#24806 = CARTESIAN_POINT ( 'NONE',  ( 4.831710525212951524, -2.520823095555479565, -62.11790713612500525 ) ) ;
#24807 = EDGE_LOOP ( 'NONE', ( #20094, #2364, #14839, #641 ) ) ;
#24808 = EDGE_CURVE ( 'NONE', #23376, #12887, #28433, .T. ) ;
#24809 = ORIENTED_EDGE ( 'NONE', *, *, #14060, .F. ) ;
#24810 = CARTESIAN_POINT ( 'NONE',  ( 23.47715715125384861, -20.00370206677004958, 0.8585801419999927742 ) ) ;
#24811 = ORIENTED_EDGE ( 'NONE', *, *, #20600, .T. ) ;
#24812 = ORIENTED_EDGE ( 'NONE', *, *, #4611, .F. ) ;
#24813 = AXIS2_PLACEMENT_3D ( 'NONE', #2330, #26696, #9392 ) ;
#24814 = PLANE ( 'NONE',  #2501 ) ;
#24815 = AXIS2_PLACEMENT_3D ( 'NONE', #12756, #663, #7572 ) ;
#24816 = LINE ( 'NONE', #22615, #29056 ) ;
#24817 = CARTESIAN_POINT ( 'NONE',  ( -26.80000000069999899, 3.281945028329999726E-15, 143.2171415869999862 ) ) ;
#24818 = UNCERTAINTY_MEASURE_WITH_UNIT (LENGTH_MEASURE( 1.000000000000000082E-05 ), #13550, 'distance_accuracy_value', 'NONE');
#24819 = VECTOR ( 'NONE', #7994, 1000.000000000000000 ) ;
#24820 = CARTESIAN_POINT ( 'NONE',  ( -23.55444264242456498, 16.04540112444970390, 8.000000000000007105 ) ) ;
#24821 = CARTESIAN_POINT ( 'NONE',  ( 24.35797964201644561, -13.39969403546014703, 6.098655031999994591 ) ) ;
#24822 = CARTESIAN_POINT ( 'NONE',  ( -14.89999999913999851, -26.99999999940830264, -34.17350269244000316 ) ) ;
#24823 = ORIENTED_EDGE ( 'NONE', *, *, #1054, .F. ) ;
#24824 = CARTESIAN_POINT ( 'NONE',  ( 2.596444431213495996, -3.474660147395747689, -44.10000000002498410 ) ) ;
#24825 = EDGE_CURVE ( 'NONE', #8453, #7951, #15656, .T. ) ;
#24826 = CARTESIAN_POINT ( 'NONE',  ( -24.43659368756648576, -14.66646236829179450, 3.899998581000013509 ) ) ;
#24827 = EDGE_CURVE ( 'NONE', #6068, #30855, #8512, .T. ) ;
#24828 = CARTESIAN_POINT ( 'NONE',  ( 0.2309929099465236890, 4.358477053493579056, -23.44418644580000333 ) ) ;
#24829 = CARTESIAN_POINT ( 'NONE',  ( -12.37073348361115954, -23.58440183081340535, -32.20121653530289763 ) ) ;
#24830 = CARTESIAN_POINT ( 'NONE',  ( -16.04158851046123502, 10.23646161653652875, 0.000000000000000000 ) ) ;
#24831 = CARTESIAN_POINT ( 'NONE',  ( 3.466821295769682159E-14, -2.890242878314739659E-13, 202.0000000000000000 ) ) ;
#24832 = FACE_BOUND ( 'NONE', #18093, .T. ) ;
#24833 = CARTESIAN_POINT ( 'NONE',  ( 4.531630834892032667, -0.6723478992683162847, -46.13818262062499542 ) ) ;
#24834 = ADVANCED_FACE ( 'NONE', ( #11021 ), #4242, .T. ) ;
#24835 = CARTESIAN_POINT ( 'NONE',  ( -26.80000000000000071, 1.065814103639999922E-14, 86.78285841159998881 ) ) ;
#24836 = CARTESIAN_POINT ( 'NONE',  ( 8.700000000277906764, -15.94902145836247342, -35.53273252485295330 ) ) ;
#24837 = CARTESIAN_POINT ( 'NONE',  ( -19.20323824044135463, 20.00026142946846264, 230.4259854455875995 ) ) ;
#24838 = CARTESIAN_POINT ( 'NONE',  ( 2.131628207279999844E-14, 1.421085471519999843E-14, 230.0904314459999966 ) ) ;
#24839 = CIRCLE ( 'NONE', #11274, 3.199999983039998774 ) ;
#24840 = AXIS2_PLACEMENT_3D ( 'NONE', #6806, #16402, #28670 ) ;
#24841 = VECTOR ( 'NONE', #18825, 1000.000000000000000 ) ;
#24842 = CARTESIAN_POINT ( 'NONE',  ( 24.34131725956216030, -12.79741914639830647, 225.2179249505068981 ) ) ;
#24843 = ORIENTED_EDGE ( 'NONE', *, *, #27337, .F. ) ;
#24844 = VECTOR ( 'NONE', #21351, 1000.000000000000000 ) ;
#24845 = CARTESIAN_POINT ( 'NONE',  ( -3.500772897184941446, -3.093025330206539802, -34.33447003410000775 ) ) ;
#24846 = EDGE_CURVE ( 'NONE', #3911, #26986, #18715, .T. ) ;
#24847 = ORIENTED_EDGE ( 'NONE', *, *, #19642, .F. ) ;
#24848 = DIRECTION ( 'NONE',  ( 0.7071067811896794009, 0.6355433650254204148, -0.3099752105697101690 ) ) ;
#24849 = CARTESIAN_POINT ( 'NONE',  ( 0.8648632234848976363, -6.342619565911398638, -50.24468436622500178 ) ) ;
#24850 = VERTEX_POINT ( 'NONE', #13532 ) ;
#24851 = ORIENTED_EDGE ( 'NONE', *, *, #2083, .F. ) ;
#24852 = DIRECTION ( 'NONE',  ( 0.9375380573047102928, -3.301521078471322125E-18, 0.3478827260806571231 ) ) ;
#24853 = VERTEX_POINT ( 'NONE', #20611 ) ;
#24854 = ORIENTED_EDGE ( 'NONE', *, *, #380, .T. ) ;
#24855 = MECHANICAL_DESIGN_GEOMETRIC_PRESENTATION_REPRESENTATION (  '', ( #24341 ), #9787 ) ;
#24856 = CARTESIAN_POINT ( 'NONE',  ( -12.84364016057614855, 20.99999999990135535, -69.49900052649185511 ) ) ;
#24857 = CARTESIAN_POINT ( 'NONE',  ( 24.36130769279719033, 13.39283555502935208, 4.791638082000004850 ) ) ;
#24858 = EDGE_CURVE ( 'NONE', #13946, #30352, #21692, .T. ) ;
#24859 = FACE_OUTER_BOUND ( 'NONE', #9271, .T. ) ;
#24860 = CYLINDRICAL_SURFACE ( 'NONE', #5408, 3.000000000000003997 ) ;
#24861 = CARTESIAN_POINT ( 'NONE',  ( 8.000000000470132377, -15.51547315099485935, -38.04330875429763381 ) ) ;
#24862 = CARTESIAN_POINT ( 'NONE',  ( -1.421085471519999843E-14, -1.065814103639999922E-14, 136.7828584120000244 ) ) ;
#24863 = CARTESIAN_POINT ( 'NONE',  ( -4.140124079000881530, 2.264562353281220908, -0.6999999999999992895 ) ) ;
#24864 = CARTESIAN_POINT ( 'NONE',  ( 10.69999999999999929, -30.49251257979999963, -21.04205368479999905 ) ) ;
#24865 = AXIS2_PLACEMENT_3D ( 'NONE', #28629, #5020, #9588 ) ;
#24866 = CARTESIAN_POINT ( 'NONE',  ( -27.92857142909999979, 3.420150602519999655E-15, 42.06031501480000401 ) ) ;
#24867 = CARTESIAN_POINT ( 'NONE',  ( -18.39373989079361138, 20.00001178696177462, -0.6589525304462929833 ) ) ;
#24868 = VECTOR ( 'NONE', #17549, 1000.000000000000000 ) ;
#24869 = CARTESIAN_POINT ( 'NONE',  ( -4.992376002455611861, -2.377191163393747253, -13.97655742010000779 ) ) ;
#24870 = CARTESIAN_POINT ( 'NONE',  ( -4.274658871253798509, -0.8336587121505270037, -31.09652066320001040 ) ) ;
#24871 = CARTESIAN_POINT ( 'NONE',  ( -2.220446049249999755E-16, -0.1455297029551360921, -71.05965357398815740 ) ) ;
#24872 = CARTESIAN_POINT ( 'NONE',  ( -2.728640529166729944, -2.273855967885826779, 227.6754430268740634 ) ) ;
#24873 = LINE ( 'NONE', #1104, #16176 ) ;
#24874 = CARTESIAN_POINT ( 'NONE',  ( -3.878879136156893281, -1.961445906012333706, -27.96472909260000606 ) ) ;
#24875 = CARTESIAN_POINT ( 'NONE',  ( 22.63992238021891978, -14.34133587286723532, 225.0964353485933600 ) ) ;
#24876 =( REPRESENTATION_RELATIONSHIP ('NONE','NONE', #2712, #24039 ) REPRESENTATION_RELATIONSHIP_WITH_TRANSFORMATION ( #1864 )SHAPE_REPRESENTATION_RELATIONSHIP( ) );
#24877 = FACE_OUTER_BOUND ( 'NONE', #21558, .T. ) ;
#24878 = CARTESIAN_POINT ( 'NONE',  ( 22.36170820408901960, 17.71391973664089292, 6.000000000000005329 ) ) ;
#24879 = AXIS2_PLACEMENT_3D ( 'NONE', #1336, #24627, #17837 ) ;
#24880 = ORIENTED_EDGE ( 'NONE', *, *, #27532, .T. ) ;
#24881 = CARTESIAN_POINT ( 'NONE',  ( 23.81776757409229361, 15.65134803726813217, 4.999998581000003384 ) ) ;
#24882 = DIRECTION ( 'NONE',  ( -0.8660254037843290176, 0.5000000000001899592, 0.000000000000000000 ) ) ;
#24883 = ORIENTED_EDGE ( 'NONE', *, *, #21795, .T. ) ;
#24884 = CARTESIAN_POINT ( 'NONE',  ( -9.000000000229999131, 21.70000000000000284, -56.09999999999999432 ) ) ;
#24885 = CARTESIAN_POINT ( 'NONE',  ( 16.06675444876397307, -9.020011618195203695, -0.6999999989999727834 ) ) ;
#24886 = EDGE_CURVE ( 'NONE', #1366, #20223, #28313, .T. ) ;
#24887 = ORIENTED_EDGE ( 'NONE', *, *, #21569, .T. ) ;
#24888 = CARTESIAN_POINT ( 'NONE',  ( -5.656593618302445670, -26.91642256435905978, 20.78194026202293543 ) ) ;
#24889 = VECTOR ( 'NONE', #15278, 1000.000000000000000 ) ;
#24890 = VERTEX_POINT ( 'NONE', #6761 ) ;
#24891 = ORIENTED_EDGE ( 'NONE', *, *, #18050, .T. ) ;
#24892 = EDGE_CURVE ( 'NONE', #25954, #68, #4022, .T. ) ;
#24893 = VERTEX_POINT ( 'NONE', #23614 ) ;
#24894 = CARTESIAN_POINT ( 'NONE',  ( -9.897162125400482680, -25.37356426577147417, 88.33953982530000815 ) ) ;
#24895 = EDGE_CURVE ( 'NONE', #14716, #19543, #8920, .T. ) ;
#24896 = DIRECTION ( 'NONE',  ( -0.3090169943750401549, -0.9510565162951233331, 0.000000000000000000 ) ) ;
#24897 = DIRECTION ( 'NONE',  ( 1.000000000000000000, -1.224606353819999582E-16, 0.000000000000000000 ) ) ;
#24898 = CARTESIAN_POINT ( 'NONE',  ( -3.441895295100000141, -11.73074823080000151, 232.6627637660000119 ) ) ;
#24899 = FACE_OUTER_BOUND ( 'NONE', #8450, .T. ) ;
#24900 = CYLINDRICAL_SURFACE ( 'NONE', #28107, 3.000000000000002220 ) ;
#24901 = CARTESIAN_POINT ( 'NONE',  ( 19.80526555962148549, 19.50877392102342256, 1.000000000000000888 ) ) ;
#24902 = TOROIDAL_SURFACE ( 'NONE', #21377, 12.03781779390000040, 5.000000000000000000 ) ;
#24903 =( GEOMETRIC_REPRESENTATION_CONTEXT ( 3 ) GLOBAL_UNCERTAINTY_ASSIGNED_CONTEXT ( ( #3366 ) ) GLOBAL_UNIT_ASSIGNED_CONTEXT ( ( #11960, #26441, #9284 ) ) REPRESENTATION_CONTEXT ( 'NONE', 'WORKASPACE' ) );
#24904 = CARTESIAN_POINT ( 'NONE',  ( 24.62873585949999722, -14.34148440729999940, 223.9040349389999847 ) ) ;
#24905 = CARTESIAN_POINT ( 'NONE',  ( 0.8228371056950706253, -6.016286819831330845, -0.3731240480000022619 ) ) ;
#24906 = CARTESIAN_POINT ( 'NONE',  ( 1.265035515811500089, -4.453021097817299712, -20.79535708920001014 ) ) ;
#24907 = CARTESIAN_POINT ( 'NONE',  ( -1.007063440337249816, -28.48249027448747839, 224.5017099588716007 ) ) ;
#24908 = LINE ( 'NONE', #15000, #16018 ) ;
#24909 = CARTESIAN_POINT ( 'NONE',  ( -27.50000000000000000, 3.367667473009999970E-15, 136.7190980919999959 ) ) ;
#24910 = DIRECTION ( 'NONE',  ( -5.962915006522622422E-16, -0.4383711467890810676, -0.8987940462991651502 ) ) ;
#24911 = DIRECTION ( 'NONE',  ( 1.000000000000000000, -1.224606353820000075E-16, 0.000000000000000000 ) ) ;
#24912 = B_SPLINE_CURVE_WITH_KNOTS ( 'NONE', 3,
 ( #20479, #11356, #28025, #20638, #4114, #6320, #13713, #3960, #8667, #8986, #11195, #23318 ),
 .UNSPECIFIED., .F., .F.,
 ( 4, 2, 2, 2, 2, 4 ),
 ( 0.000000000000000000, 0.2500000000000037192, 0.3750000000000043299, 0.5000000000000049960, 0.7500000000000024425, 1.000000000000000000 ),
 .UNSPECIFIED. ) ;
#24913 = CARTESIAN_POINT ( 'NONE',  ( 2.813577582285908818, 2.131591337306447453, -0.6999999999999784173 ) ) ;
#24914 = CYLINDRICAL_SURFACE ( 'NONE', #2208, 26.80000000000002203 ) ;
#24915 = DIRECTION ( 'NONE',  ( 0.000000000000000000, -2.257145581549999994E-12, -1.000000000000000000 ) ) ;
#24916 = ORIENTED_EDGE ( 'NONE', *, *, #11755, .T. ) ;
#24917 = CARTESIAN_POINT ( 'NONE',  ( -0.05052225346893063351, 4.317558364482401601, -57.31818518972499987 ) ) ;
#24918 = CYLINDRICAL_SURFACE ( 'NONE', #26376, 1.099999999999998979 ) ;
#24919 = DIRECTION ( 'NONE',  ( -1.000000000000000000, 5.063197467948052462E-16, -2.257212216284997029E-12 ) ) ;
#24920 = CARTESIAN_POINT ( 'NONE',  ( -26.91170281299162426, 9.095659093862945355, 0.7069222149999887517 ) ) ;
#24921 = CARTESIAN_POINT ( 'NONE',  ( -4.203413175848027983, 0.5343955542015218496, -68.10000000002501963 ) ) ;
#24922 = VERTEX_POINT ( 'NONE', #11488 ) ;
#24923 = VERTEX_POINT ( 'NONE', #25815 ) ;
#24924 = CARTESIAN_POINT ( 'NONE',  ( 2.105377028506504988, 2.977322161815887380, -92.06382165379619664 ) ) ;
#24925 =( NAMED_UNIT ( * ) PLANE_ANGLE_UNIT ( ) SI_UNIT ( $, .RADIAN. ) );
#24926 = EDGE_LOOP ( 'NONE', ( #26474, #11552, #10524, #7274 ) ) ;
#24927 = CARTESIAN_POINT ( 'NONE',  ( -24.74993094845043018, 14.13250375615880117, 3.957489350000009676 ) ) ;
#24928 = ADVANCED_FACE ( 'NONE', ( #13373 ), #2050, .T. ) ;
#24929 = CARTESIAN_POINT ( 'NONE',  ( -7.999999999718343524, -24.19750589173343869, -27.32947359979155166 ) ) ;
#24930 = CARTESIAN_POINT ( 'NONE',  ( -4.543473910928012671, 0.02303893552233621245, -62.57122063472500884 ) ) ;
#24931 = CARTESIAN_POINT ( 'NONE',  ( 1.615442258875288362, -28.45452079205452733, 5.290483759618271442 ) ) ;
#24932 = FACE_OUTER_BOUND ( 'NONE', #14100, .T. ) ;
#24933 = CARTESIAN_POINT ( 'NONE',  ( 1.110223024630000146E-16, 0.000000000000000000, -43.39999999999999858 ) ) ;
#24934 = PRESENTATION_STYLE_ASSIGNMENT (( #720 ) ) ;
#24935 = CARTESIAN_POINT ( 'NONE',  ( -10.00000000050000004, -24.95850565390000142, -26.20104569390000293 ) ) ;
#24936 = ORIENTED_EDGE ( 'NONE', *, *, #2788, .T. ) ;
#24937 = CARTESIAN_POINT ( 'NONE',  ( -27.06563795990000187, 3.314475221589999487E-15, 41.94026860139999258 ) ) ;
#24938 = CARTESIAN_POINT ( 'NONE',  ( -26.80000000069999899, 3.281945028329999726E-15, 93.21714158910000947 ) ) ;
#24939 = VERTEX_POINT ( 'NONE', #25663 ) ;
#24940 = CARTESIAN_POINT ( 'NONE',  ( 14.76126683899760117, -31.99975590309085760, -29.64037414300432616 ) ) ;
#24941 = CARTESIAN_POINT ( 'NONE',  ( -24.43659368756648576, -14.66646236829179450, 6.099998581000020792 ) ) ;
#24942 = DIRECTION ( 'NONE',  ( 0.000000000000000000, 0.3420201433259318913, -0.9396926207858126157 ) ) ;
#24943 = CARTESIAN_POINT ( 'NONE',  ( 23.66291322330000213, -14.59162663150000050, 224.2398658380000143 ) ) ;
#24944 = DIRECTION ( 'NONE',  ( 0.8086898285215826654, 0.000000000000000000, 0.5882352941176968164 ) ) ;
#24945 = CARTESIAN_POINT ( 'NONE',  ( 3.357972723926252456, -2.601985670799683348, -0.6999999999999992895 ) ) ;
#24946 = CARTESIAN_POINT ( 'NONE',  ( -12.57906051704346595, 20.99999999997321964, -55.96254875484549984 ) ) ;
#24947 = CARTESIAN_POINT ( 'NONE',  ( 22.75759212980393187, -14.15424219578301113, 224.3233986261513451 ) ) ;
#24948 = ORIENTED_EDGE ( 'NONE', *, *, #12589, .T. ) ;
#24949 = PLANE ( 'NONE',  #1210 ) ;
#24950 = CARTESIAN_POINT ( 'NONE',  ( 17.29052662034098020, 12.10243747006436799, 1.385610376436474667E-13 ) ) ;
#24951 = ADVANCED_FACE ( 'NONE', ( #9269 ), #18875, .F. ) ;
#24952 = B_SPLINE_CURVE_WITH_KNOTS ( 'NONE', 3,
 ( #12898, #17909, #3443, #18067, #10544, #20756 ),
 .UNSPECIFIED., .F., .F.,
 ( 4, 2, 4 ),
 ( 0.000000000000000000, 0.5000000000000000000, 1.000000000000000000 ),
 .UNSPECIFIED. ) ;
#24953 = CARTESIAN_POINT ( 'NONE',  ( -6.076762841307600915, -26.10292173851732400, 21.17116608273227740 ) ) ;
#24954 = CARTESIAN_POINT ( 'NONE',  ( -0.3076636919214117971, -28.49867017228250177, 5.759626916000016195 ) ) ;
#24955 = ORIENTED_EDGE ( 'NONE', *, *, #25435, .T. ) ;
#24956 = DIRECTION ( 'NONE',  ( 1.000000000000000000, -1.843431230208684274E-12, 2.650498504958264790E-12 ) ) ;
#24957 =( NAMED_UNIT ( * ) PLANE_ANGLE_UNIT ( ) SI_UNIT ( $, .RADIAN. ) );
#24958 = CARTESIAN_POINT ( 'NONE',  ( 14.65905325913535684, -26.09901808550156943, -33.65287045170772728 ) ) ;
#24959 = CARTESIAN_POINT ( 'NONE',  ( -17.79876841389999598, 11.52736809249999617, -0.7000000003999986564 ) ) ;
#24960 = CARTESIAN_POINT ( 'NONE',  ( -4.300317018729668206, 2.364939115720640750, -60.21908057272500514 ) ) ;
#24961 = VERTEX_POINT ( 'NONE', #1585 ) ;
#24962 = ORIENTED_EDGE ( 'NONE', *, *, #7521, .T. ) ;
#24963 = CARTESIAN_POINT ( 'NONE',  ( 22.63260994176697238, -19.28417101125922883, 0.000000000000000000 ) ) ;
#24964 = VERTEX_POINT ( 'NONE', #8640 ) ;
#24965 = ADVANCED_FACE ( 'NONE', ( #22981 ), #7380, .F. ) ;
#24966 = CARTESIAN_POINT ( 'NONE',  ( -11.51892196954422154, 21.69999999997437712, -55.45368347834880041 ) ) ;
#24967 = CARTESIAN_POINT ( 'NONE',  ( -12.29999999990041459, -26.60730091830127009, -31.40000000019999860 ) ) ;
#24968 = CARTESIAN_POINT ( 'NONE',  ( 1.630907769230000026, 5.558498091359999727, 229.6412452697800006 ) ) ;
#24969 = CARTESIAN_POINT ( 'NONE',  ( -17.37283180965889784, -25.76431098467556424, -33.46007730646741152 ) ) ;
#24970 = CARTESIAN_POINT ( 'NONE',  ( 25.46368747440213198, -12.80129684534102807, 4.999998581000003384 ) ) ;
#24971 = DIRECTION ( 'NONE',  ( 1.595945597898660305E-12, 0.7071067811865475727, -0.7071067811865475727 ) ) ;
#24972 = ORIENTED_EDGE ( 'NONE', *, *, #13427, .T. ) ;
#24973 = CARTESIAN_POINT ( 'NONE',  ( 1.456882742358924565, -3.834140411209185473, -44.10000000002499121 ) ) ;
#24974 = CARTESIAN_POINT ( 'NONE',  ( -8.699999999710087195, -24.01208115640663010, -28.87640755789744063 ) ) ;
#24975 = CIRCLE ( 'NONE', #11416, 8.134694044909998922 ) ;
#24976 = CARTESIAN_POINT ( 'NONE',  ( 4.692682656939434871, -1.014318600726540787, -24.72786215649999519 ) ) ;
#24977 = CARTESIAN_POINT ( 'NONE',  ( 23.68794489801944181, -12.53584098811867698, 4.508626838105977086 ) ) ;
#24978 = LINE ( 'NONE', #29850, #8984 ) ;
#24979 = DIRECTION ( 'NONE',  ( 0.000000000000000000, 1.000000000000000000, 9.516197338740001367E-15 ) ) ;
#24980 = PLANE ( 'NONE',  #23741 ) ;
#24981 = CARTESIAN_POINT ( 'NONE',  ( 4.315256771988532414, 1.538274589489400990, -45.92627377572499370 ) ) ;
#24982 = EDGE_CURVE ( 'NONE', #409, #2487, #16659, .T. ) ;
#24983 = DIRECTION ( 'NONE',  ( 0.000000000000000000, -0.9396926207858125046, -0.3420201433259318358 ) ) ;
#24984 = DIRECTION ( 'NONE',  ( -2.764840495839172514E-12, -0.9128796883888952163, 0.4082287037029530552 ) ) ;
#24985 = CARTESIAN_POINT ( 'NONE',  ( -19.14227085988751043, 20.00032846726916347, 230.4526156311602847 ) ) ;
#24986 = CARTESIAN_POINT ( 'NONE',  ( -21.27344192715450433, -16.32329153680506195, 43.21714158846668141 ) ) ;
#24987 = CARTESIAN_POINT ( 'NONE',  ( 3.918707624292984804, -26.51317744985242797, 20.25387219759830160 ) ) ;
#24988 = ORIENTED_EDGE ( 'NONE', *, *, #13486, .F. ) ;
#24989 = PRODUCT_DEFINITION_SHAPE ( 'NONE', 'NONE',  #31129 ) ;
#24990 = CARTESIAN_POINT ( 'NONE',  ( 2.635706879431563898, 5.544231365240147369, -32.75113063600000629 ) ) ;
#24991 = ORIENTED_EDGE ( 'NONE', *, *, #23342, .F. ) ;
#24992 = EDGE_CURVE ( 'NONE', #2860, #13706, #4558, .T. ) ;
#24993 = CARTESIAN_POINT ( 'NONE',  ( 10.14902473063354549, -26.01926976387845869, 142.0603150149999863 ) ) ;
#24994 = CARTESIAN_POINT ( 'NONE',  ( -0.7556487780321572423, 4.453147011089724217, -51.25792092402500089 ) ) ;
#24995 = VERTEX_POINT ( 'NONE', #12098 ) ;
#24996 = VERTEX_POINT ( 'NONE', #7535 ) ;
#24997 = AXIS2_PLACEMENT_3D ( 'NONE', #1408, #8462, #27985 ) ;
#24998 = EDGE_CURVE ( 'NONE', #26453, #5171, #9899, .T. ) ;
#24999 = EDGE_LOOP ( 'NONE', ( #1967, #20911, #786, #10466 ) ) ;
#25000 = TOROIDAL_SURFACE ( 'NONE', #6407, 12.03781779390000040, 6.000000000000000000 ) ;
#25001 = VERTEX_POINT ( 'NONE', #9736 ) ;
#25002 = CARTESIAN_POINT ( 'NONE',  ( 24.47278418934676836, 14.60601539428441598, 3.904031772999999816 ) ) ;
#25003 = DIRECTION ( 'NONE',  ( 0.000000000000000000, 0.000000000000000000, 1.000000000000000000 ) ) ;
#25004 = CARTESIAN_POINT ( 'NONE',  ( 3.242686849810665795, 3.944686721199032853, -35.69999999999999574 ) ) ;
#25005 = CARTESIAN_POINT ( 'NONE',  ( 7.999999999974046538, -116.8591659214849159, 11.34031266730467813 ) ) ;
#25006 = CARTESIAN_POINT ( 'NONE',  ( -12.41081696006088819, -28.32863187924899862, -23.39381857568974965 ) ) ;
#25007 = CARTESIAN_POINT ( 'NONE',  ( -3.793660607282320463, 2.420557939024130967, -0.6999999999999991784 ) ) ;
#25008 = DIRECTION ( 'NONE',  ( 1.000000000000000000, 0.000000000000000000, 0.000000000000000000 ) ) ;
#25009 = CARTESIAN_POINT ( 'NONE',  ( -3.862245930668567251, -0.3103938167503151324, 227.8554272724453824 ) ) ;
#25010 = FACE_OUTER_BOUND ( 'NONE', #16568, .T. ) ;
#25011 = EDGE_LOOP ( 'NONE', ( #26323, #25712, #12678, #23346 ) ) ;
#25012 = AXIS2_PLACEMENT_3D ( 'NONE', #18358, #3719, #25125 ) ;
#25013 = CARTESIAN_POINT ( 'NONE',  ( -0.6370991518874399295, 4.292107257743936977, -11.36772091660000150 ) ) ;
#25014 = CARTESIAN_POINT ( 'NONE',  ( 4.904813032679735230, 3.691647504909488564, -31.76032172560000433 ) ) ;
#25015 = AXIS2_PLACEMENT_3D ( 'NONE', #29951, #30271, #20987 ) ;
#25016 = EDGE_CURVE ( 'NONE', #16634, #6458, #18272, .T. ) ;
#25017 = DIRECTION ( 'NONE',  ( 0.000000000000000000, 0.000000000000000000, 1.000000000000000000 ) ) ;
#25018 = FACE_OUTER_BOUND ( 'NONE', #4356, .T. ) ;
#25019 = CARTESIAN_POINT ( 'NONE',  ( 28.68577476828162531, -9.950727360111285336, 1.000000000000000888 ) ) ;
#25020 = CARTESIAN_POINT ( 'NONE',  ( 0.4702670923949999748, -27.79645255899999867, 226.0025203910000187 ) ) ;
#25021 = CARTESIAN_POINT ( 'NONE',  ( 3.802779202691175531, 1.094990851247104491, -35.53910482769999390 ) ) ;
#25022 = CIRCLE ( 'NONE', #20509, 27.23548387060000309 ) ;
#25023 = B_SPLINE_CURVE_WITH_KNOTS ( 'NONE', 3,
 ( #5156, #14768, #468, #920 ),
 .UNSPECIFIED., .F., .F.,
 ( 4, 4 ),
 ( 0.000000000000000000, 1.000000000000000000 ),
 .UNSPECIFIED. ) ;
#25025 = CARTESIAN_POINT ( 'NONE',  ( 24.03830838765967925, 13.56270118689358206, -0.6999999999999784173 ) ) ;
#25024 = B_SPLINE_CURVE_WITH_KNOTS ( 'NONE', 5,
 ( #8170, #13206, #10701, #3153, #966, #17772, #5670, #5823, #15422 ),
 .UNSPECIFIED., .F., .F.,
 ( 6, 3, 6 ),
 ( 67.22752578339999729, 77.81866039000000512, 88.40979499649999696 ),
 .UNSPECIFIED. ) ;
#25026 = CARTESIAN_POINT ( 'NONE',  ( -8.699999999660121830, -13.53288334731636233, -36.25379057756155277 ) ) ;
#25027 = CARTESIAN_POINT ( 'NONE',  ( 20.30396079662882158, 20.00000000004802203, 3.000000000000002665 ) ) ;
#25028 = ORIENTED_EDGE ( 'NONE', *, *, #64, .F. ) ;
#25029 = ORIENTED_EDGE ( 'NONE', *, *, #27492, .T. ) ;
#25030 = ADVANCED_FACE ( 'NONE', ( #29089, #16975 ), #17126, .T. ) ;
#25031 = CARTESIAN_POINT ( 'NONE',  ( 18.26639035967037827, -8.979988381807324060, -1.000005633855494125E-09 ) ) ;
#25032 = DIRECTION ( 'NONE',  ( -0.9316362575375349842, 0.3633921898465292122, -0.000000000000000000 ) ) ;
#25033 = ORIENTED_EDGE ( 'NONE', *, *, #29108, .F. ) ;
#25034 = CARTESIAN_POINT ( 'NONE',  ( -22.77614505619871110, -14.12431931101418492, 224.2880739206591727 ) ) ;
#25035 = LINE ( 'NONE', #29749, #30819 ) ;
#25036 = ORIENTED_EDGE ( 'NONE', *, *, #7021, .T. ) ;
#25037 = CARTESIAN_POINT ( 'NONE',  ( -7.554893095320830199, -26.44255681430371396, 22.11862154216139942 ) ) ;
#25038 = ORIENTED_EDGE ( 'NONE', *, *, #4217, .T. ) ;
#25039 = ORIENTED_EDGE ( 'NONE', *, *, #27899, .T. ) ;
#25040 = VECTOR ( 'NONE', #5190, 1000.000000000000000 ) ;
#25041 = ORIENTED_EDGE ( 'NONE', *, *, #3341, .F. ) ;
#25042 = CARTESIAN_POINT ( 'NONE',  ( 28.04325408099999706, 4.735556750389999792, 230.2432540810000319 ) ) ;
#25043 = EDGE_CURVE ( 'NONE', #4605, #8967, #15270, .T. ) ;
#25044 = CARTESIAN_POINT ( 'NONE',  ( -4.041451884379999804, 9.156941871420000667E-11, 229.2412452703699728 ) ) ;
#25045 = CARTESIAN_POINT ( 'NONE',  ( -7.999999999652283478, -16.96959321758620476, -37.81493174591201978 ) ) ;
#25046 = CARTESIAN_POINT ( 'NONE',  ( -28.50000000000000000, 1.776356839399999922E-14, 222.0000000000000000 ) ) ;
#25047 = CARTESIAN_POINT ( 'NONE',  ( -20.30396346370000060, 20.00000000000000000, 228.5999999999999943 ) ) ;
#25048 = CARTESIAN_POINT ( 'NONE',  ( -2.299991308520000465E-10, 20.99999999990000887, -70.09999999999999432 ) ) ;
#25049 = AXIS2_PLACEMENT_3D ( 'NONE', #16462, #26076, #16922 ) ;
#25050 = CARTESIAN_POINT ( 'NONE',  ( 9.736208184377293406, -25.71890933281309444, 204.0979242502758666 ) ) ;
#25051 = CARTESIAN_POINT ( 'NONE',  ( 24.25493619443923876, -13.58601077461538509, 3.899998581000038378 ) ) ;
#25052 = ORIENTED_EDGE ( 'NONE', *, *, #10234, .F. ) ;
#25053 = CARTESIAN_POINT ( 'NONE',  ( -5.478535709405480958, -2.209361269785813153, -1.997197434499998758 ) ) ;
#25054 = CARTESIAN_POINT ( 'NONE',  ( -4.448701673712592175, 0.6187532242676700989, -18.75159460730000660 ) ) ;
#25055 = CARTESIAN_POINT ( 'NONE',  ( 4.239428892460699881E-14, 6.006117008548172241E-13, 232.1412452697749984 ) ) ;
#25056 = EDGE_CURVE ( 'NONE', #3279, #11498, #4767, .T. ) ;
#25057 = DIRECTION ( 'NONE',  ( 0.000000000000000000, 0.3420201433259318913, -0.9396926207858126157 ) ) ;
#25058 = CARTESIAN_POINT ( 'NONE',  ( 25.22625794089999829, -13.26224522399999906, 225.0000014190000002 ) ) ;
#25059 = CARTESIAN_POINT ( 'NONE',  ( -21.20818545079999851, 16.99505982179999819, 230.6999999999999886 ) ) ;
#25060 = CARTESIAN_POINT ( 'NONE',  ( -10.69999999969999926, -30.19999999925000012, -28.40000000000000213 ) ) ;
#25061 = AXIS2_PLACEMENT_3D ( 'NONE', #108, #24629, #14726 ) ;
#25062 = EDGE_CURVE ( 'NONE', #3709, #19797, #22417, .T. ) ;
#25063 = CARTESIAN_POINT ( 'NONE',  ( 27.79999999999999716, 2.344791028010000161E-11, 222.0000000000000000 ) ) ;
#25064 = CARTESIAN_POINT ( 'NONE',  ( -26.80000000069999899, -2.537339890029999712, 230.6999999999999886 ) ) ;
#25065 = CARTESIAN_POINT ( 'NONE',  ( 4.011748363780728077, -0.5882954696724371768, -40.53004412028315784 ) ) ;
#25066 = ORIENTED_EDGE ( 'NONE', *, *, #14214, .F. ) ;
#25067 = CARTESIAN_POINT ( 'NONE',  ( -0.06088579265679563285, 5.203211362304668519, -56.51818518972498850 ) ) ;
#25068 = CARTESIAN_POINT ( 'NONE',  ( -24.12437076912601341, -15.17512416476963111, 5.965434395632247977 ) ) ;
#25069 = CARTESIAN_POINT ( 'NONE',  ( -2.564224011391953884, 5.541743391097003979, -7.731725184300000997 ) ) ;
#25070 = ORIENTED_EDGE ( 'NONE', *, *, #22251, .T. ) ;
#25071 = CARTESIAN_POINT ( 'NONE',  ( -2.698832034861248896, 3.511840374587876568, -39.19200816765035000 ) ) ;
#25072 = VECTOR ( 'NONE', #21506, 1000.000000000000000 ) ;
#25073 = CARTESIAN_POINT ( 'NONE',  ( -4.468241980872267760, 1.080773483108106614, -68.10000000002501963 ) ) ;
#25074 = ORIENTED_EDGE ( 'NONE', *, *, #7347, .T. ) ;
#25075 = ORIENTED_EDGE ( 'NONE', *, *, #12881, .T. ) ;
#25076 = ORIENTED_EDGE ( 'NONE', *, *, #11422, .F. ) ;
#25077 = CARTESIAN_POINT ( 'NONE',  ( -3.331151133293480893, 0.6533045715718522883, -94.29636648343951322 ) ) ;
#25078 = VERTEX_POINT ( 'NONE', #14775 ) ;
#25079 = CARTESIAN_POINT ( 'NONE',  ( -24.93720648713954446, 13.79881813474513486, 3.899998581000013509 ) ) ;
#25080 = B_SPLINE_CURVE_WITH_KNOTS ( 'NONE', 5,
 ( #20714, #30151, #7696, #19972, #1527, #23237, #8743, #10075, #791, #30313, #19670, #22496 ),
 .UNSPECIFIED., .F., .F.,
 ( 6, 3, 3, 6 ),
 ( -1.429360140840000071, -1.143488112680000057, -0.5717440563379999618, 2.220446049250313081E-16 ),
 .UNSPECIFIED. ) ;
#25081 = CARTESIAN_POINT ( 'NONE',  ( -2.100000000000000089, -6.661338147749999512E-16, 226.6412452697800006 ) ) ;
#25082 = CARTESIAN_POINT ( 'NONE',  ( 1.165515511291096873, -4.760067307274400861, -63.95397119102499772 ) ) ;
#25083 = DIRECTION ( 'NONE',  ( 1.000000000000000000, -0.000000000000000000, -2.257150022439999944E-12 ) ) ;
#25084 = AXIS2_PLACEMENT_3D ( 'NONE', #10196, #7518, #17113 ) ;
#25085 = B_SPLINE_CURVE_WITH_KNOTS ( 'NONE', 3,
 ( #1821, #21013, #30617, #23538, #25896, #23841 ),
 .UNSPECIFIED., .F., .F.,
 ( 4, 2, 4 ),
 ( 0.000000000000000000, 0.5000000000000000000, 1.000000000000000000 ),
 .UNSPECIFIED. ) ;
#25086 = CARTESIAN_POINT ( 'NONE',  ( -27.12080906453036278, 4.172318231302202030, -0.6999999999999784173 ) ) ;
#25087 = CARTESIAN_POINT ( 'NONE',  ( 9.775610180800001103, 19.99999999999999645, -43.93713984030800646 ) ) ;
#25088 = CARTESIAN_POINT ( 'NONE',  ( -27.50000000000000000, 3.367667473009999970E-15, 193.2809019210000088 ) ) ;
#25089 = CARTESIAN_POINT ( 'NONE',  ( -25.35851007062240114, 13.00862288638852959, 4.319165764000016061 ) ) ;
#25090 = ORIENTED_EDGE ( 'NONE', *, *, #6413, .F. ) ;
#25091 = PRODUCT_DEFINITION_CONTEXT ( 'detailed design', #2950, 'design' ) ;
#25092 = AXIS2_PLACEMENT_3D ( 'NONE', #13116, #17673, #22725 ) ;
#25093 = CARTESIAN_POINT ( 'NONE',  ( -4.338779899226326009, -4.343559731693466652, -9.213991631000000737 ) ) ;
#25094 = CARTESIAN_POINT ( 'NONE',  ( -27.23548387100000312, 8.881784196999999612E-15, 41.66046017469999896 ) ) ;
#25095 = DIRECTION ( 'NONE',  ( -1.000000000000000000, 0.000000000000000000, -6.771000000000000128E-12 ) ) ;
#25096 = ORIENTED_EDGE ( 'NONE', *, *, #3346, .T. ) ;
#25097 = CARTESIAN_POINT ( 'NONE',  ( 24.19477113890000197, -13.69187437440000110, 223.9201473980000117 ) ) ;
#25098 = CARTESIAN_POINT ( 'NONE',  ( -23.87170005649112525, -14.24726900567271493, 6.095965388000001539 ) ) ;
#25099 = CARTESIAN_POINT ( 'NONE',  ( -14.09657507470000226, -28.30410041510000241, 222.0000000000000000 ) ) ;
#25100 = CARTESIAN_POINT ( 'NONE',  ( 27.79539923781770483, 0.5057481688777786255, 0.8585786439999909536 ) ) ;
#25101 = CARTESIAN_POINT ( 'NONE',  ( -9.543143524407900813, -25.04338540923419743, 203.8394562065719811 ) ) ;
#25102 = CARTESIAN_POINT ( 'NONE',  ( 5.363076718300177959, -2.525690298526013677, -52.29872167392500160 ) ) ;
#25103 = DIRECTION ( 'NONE',  ( 0.7071067811865475727, 0.6644630243886071597, 0.2418447626481610435 ) ) ;
#25105 = ADVANCED_FACE ( 'NONE', ( #19029 ), #24345, .T. ) ;
#25104 = CARTESIAN_POINT ( 'NONE',  ( 22.63992238019999803, -14.34133587289999845, 225.0000000000000000 ) ) ;
#25106 = ORIENTED_EDGE ( 'NONE', *, *, #29259, .T. ) ;
#25107 = CARTESIAN_POINT ( 'NONE',  ( 23.79228474585360686, -14.38012950158411662, 4.689353541000001790 ) ) ;
#25108 = CARTESIAN_POINT ( 'NONE',  ( 27.79999999990000248, 4.333901782529999025, 224.8000000000000114 ) ) ;
#25109 = CARTESIAN_POINT ( 'NONE',  ( -4.433903769297805830, -26.43189459824145615, 20.40472646930128775 ) ) ;
#25110 = CARTESIAN_POINT ( 'NONE',  ( 0.1280637868466714679, -3.973485157313911387, -68.10000000002500542 ) ) ;
#25111 = B_SPLINE_CURVE_WITH_KNOTS ( 'NONE', 1,
 ( #18835, #28128 ),
 .UNSPECIFIED., .F., .F.,
 ( 2, 2 ),
 ( -2.557514682700000071E-06, 0.7000000000009999335 ),
 .UNSPECIFIED. ) ;
#25112 = CARTESIAN_POINT ( 'NONE',  ( 11.14649462760000098, -24.37257236010000128, -0.7852065437999946607 ) ) ;
#25113 = AXIS2_PLACEMENT_3D ( 'NONE', #4348, #18655, #28255 ) ;
#25114 = CARTESIAN_POINT ( 'NONE',  ( -10.32522729140000095, -24.73114799960000099, -1.399999999999998579 ) ) ;
#25115 = CARTESIAN_POINT ( 'NONE',  ( 0.7914749696353690078, 2.922173311402426865, -42.24221414595644575 ) ) ;
#25116 = CARTESIAN_POINT ( 'NONE',  ( -4.050122923326508584, -2.059172231882750559, -62.36424626872499033 ) ) ;
#25117 = ORIENTED_EDGE ( 'NONE', *, *, #13303, .F. ) ;
#25118 = CARTESIAN_POINT ( 'NONE',  ( 17.91270342211725008, 20.00000026367296968, 230.7000000000000739 ) ) ;
#25119 = ORIENTED_EDGE ( 'NONE', *, *, #10974, .F. ) ;
#25120 = CARTESIAN_POINT ( 'NONE',  ( -19.53673505992006554, -20.39066108913833020, 0.000000000000000000 ) ) ;
#25121 = ORIENTED_EDGE ( 'NONE', *, *, #22699, .T. ) ;
#25122 = DIRECTION ( 'NONE',  ( 1.000000000000000000, 0.000000000000000000, 0.000000000000000000 ) ) ;
#25123 = EDGE_CURVE ( 'NONE', #26249, #12816, #2515, .T. ) ;
#25124 = CARTESIAN_POINT ( 'NONE',  ( 9.993285220779439371, -25.61999708228226069, 186.3944487260000074 ) ) ;
#25125 = DIRECTION ( 'NONE',  ( 1.000000000000000000, 0.000000000000000000, 0.000000000000000000 ) ) ;
#25126 = CARTESIAN_POINT ( 'NONE',  ( -17.47972357343276428, -24.02078344067320970, -32.45345120959760976 ) ) ;
#25127 = CARTESIAN_POINT ( 'NONE',  ( 0.000000000000000000, 0.000000000000000000, 210.0000000000000284 ) ) ;
#25128 = CYLINDRICAL_SURFACE ( 'NONE', #17529, 2.000000000000000444 ) ;
#25129 = EDGE_LOOP ( 'NONE', ( #1112, #2666, #3836, #22453 ) ) ;
#25130 = FACE_OUTER_BOUND ( 'NONE', #24544, .T. ) ;
#25131 = DIRECTION ( 'NONE',  ( 0.000000000000000000, 0.000000000000000000, -1.000000000000000000 ) ) ;
#25132 = MECHANICAL_DESIGN_GEOMETRIC_PRESENTATION_REPRESENTATION (  '', ( #9047 ), #19614 ) ;
#25133 = CARTESIAN_POINT ( 'NONE',  ( 3.375516224911112584, -2.766870103071181308, -23.99674734060000603 ) ) ;
#25134 = DIRECTION ( 'NONE',  ( 0.000000000000000000, 0.000000000000000000, 1.000000000000000000 ) ) ;
#25135 = CARTESIAN_POINT ( 'NONE',  ( 19.80538173989999962, 19.50875420239999869, 228.5999999789999890 ) ) ;
#25136 = DIRECTION ( 'NONE',  ( 0.9880370573969197157, -0.1542166437529880474, 0.000000000000000000 ) ) ;
#25137 = CARTESIAN_POINT ( 'NONE',  ( 0.2820261973285071999, -27.79909623906206662, 223.9267880206792540 ) ) ;
#25138 = CARTESIAN_POINT ( 'NONE',  ( 3.389692407805919849, 3.523397910813145906, -48.29426496242500377 ) ) ;
#25139 = CYLINDRICAL_SURFACE ( 'NONE', #26798, 2.926829268290000119 ) ;
#25140 = PRODUCT_DEFINITION_SHAPE ( 'NONE', 'NONE',  #5604 ) ;
#25141 = CARTESIAN_POINT ( 'NONE',  ( -2.947640775130000104E-14, -27.50000000000000000, 210.0000000000000284 ) ) ;
#25142 = CARTESIAN_POINT ( 'NONE',  ( -20.04009859691944584, 19.99997709909766641, 229.7758549911204398 ) ) ;
#25143 = CARTESIAN_POINT ( 'NONE',  ( -4.175165894169885483, -50.49316738903675628, -43.39999999999999858 ) ) ;
#25144 = CARTESIAN_POINT ( 'NONE',  ( -2.099999999790000960, 0.2762902854420857257, 226.6412452697799722 ) ) ;
#25145 = ORIENTED_EDGE ( 'NONE', *, *, #14635, .T. ) ;
#25146 = CARTESIAN_POINT ( 'NONE',  ( -0.4593365651765490831, 6.553622599173768215, -34.89518930509999706 ) ) ;
#25147 = B_SPLINE_CURVE_WITH_KNOTS ( 'NONE', 5,
 ( #6371, #23686, #20858, #18635, #1818, #4482, #28549, #25734, #11407, #23838, #21009, #13926 ),
 .UNSPECIFIED., .F., .F.,
 ( 6, 3, 3, 6 ),
 ( 0.2292465732300000003, 0.5717440563929999664, 1.143488112780000066, 1.429360140980000082 ),
 .UNSPECIFIED. ) ;
#25148 = ORIENTED_EDGE ( 'NONE', *, *, #20474, .T. ) ;
#25149 = EDGE_CURVE ( 'NONE', #19664, #27935, #17279, .T. ) ;
#25150 = B_SPLINE_CURVE_WITH_KNOTS ( 'NONE', 3,
 ( #10419, #20011, #26784, #15287, #10112, #2866 ),
 .UNSPECIFIED., .F., .F.,
 ( 4, 2, 4 ),
 ( 0.000000000000000000, 0.5000000000000000000, 1.000000000000000000 ),
 .UNSPECIFIED. ) ;
#25151 = CARTESIAN_POINT ( 'NONE',  ( -4.000000000000000000, -29.27600094726834712, -81.66227801707495360 ) ) ;
#25152 = CARTESIAN_POINT ( 'NONE',  ( -4.652656055762370180, -1.626095028925849562, -51.15743646232500197 ) ) ;
#25153 = ORIENTED_EDGE ( 'NONE', *, *, #22132, .T. ) ;
#25154 = EDGE_CURVE ( 'NONE', #12078, #13677, #21554, .T. ) ;
#25155 = APPLICATION_PROTOCOL_DEFINITION ( 'draft international standard', 'automotive_design', 1998, #10172 ) ;
#25156 = ORIENTED_EDGE ( 'NONE', *, *, #8459, .T. ) ;
#25157 = EDGE_LOOP ( 'NONE', ( #5824, #10751, #18844, #15546, #14327, #9473 ) ) ;
#25158 = DIRECTION ( 'NONE',  ( 0.000000000000000000, 0.000000000000000000, -1.000000000000000000 ) ) ;
#25159 = EDGE_CURVE ( 'NONE', #22644, #15738, #8118, .T. ) ;
#25160 = FACE_OUTER_BOUND ( 'NONE', #328, .T. ) ;
#25161 = CARTESIAN_POINT ( 'NONE',  ( -27.54391550599999761, 3.373045393779999685E-15, 87.04374668509998969 ) ) ;
#25162 = CARTESIAN_POINT ( 'NONE',  ( -27.79999999999999716, -2.354383354940000152E-11, 222.0000000000000000 ) ) ;
#25163 = CARTESIAN_POINT ( 'NONE',  ( -0.4949169567396824454, -27.49533956265154799, 4.006901989143670129 ) ) ;
#25164 = CARTESIAN_POINT ( 'NONE',  ( -5.045264861105531295, 0.3129595611791647913, -0.6999999999999992895 ) ) ;
#25165 = CARTESIAN_POINT ( 'NONE',  ( 4.360957369889332469, -0.1505632777267530420, -2.185409721200005428 ) ) ;
#25166 = CARTESIAN_POINT ( 'NONE',  ( 12.00723796141030775, 26.18431201388056095, -59.34801937115905446 ) ) ;
#25167 = CARTESIAN_POINT ( 'NONE',  ( 8.000000000654496901, -17.81372394443670615, -37.29648778942958387 ) ) ;
#25168 = ORIENTED_EDGE ( 'NONE', *, *, #7964, .F. ) ;
#25169 = CARTESIAN_POINT ( 'NONE',  ( 4.294959833232216972, -2.194189917041240445, -12.85224735220000092 ) ) ;
#25170 = CARTESIAN_POINT ( 'NONE',  ( -2.539202180960155264, -4.449342792696782567, -29.73892233980000910 ) ) ;
#25171 = DIRECTION ( 'NONE',  ( 2.257102469710000208E-12, 0.000000000000000000, 1.000000000000000000 ) ) ;
#25172 = ADVANCED_FACE ( 'NONE', ( #19957 ), #15085, .F. ) ;
#25173 = FACE_OUTER_BOUND ( 'NONE', #8691, .T. ) ;
#25174 = CARTESIAN_POINT ( 'NONE',  ( 0.000000000000000000, 3.552713678799999608E-15, 191.6604601750000256 ) ) ;
#25175 = CARTESIAN_POINT ( 'NONE',  ( 0.07063658732340000190, -28.50016343120000073, 226.0986540789999992 ) ) ;
#25176 = DIRECTION ( 'NONE',  ( -1.000000000000000000, 0.000000000000000000, 0.000000000000000000 ) ) ;
#25177 = CARTESIAN_POINT ( 'NONE',  ( 18.66688021548718979, 20.92780155529449715, -0.2432540810000105580 ) ) ;
#25178 = DIRECTION ( 'NONE',  ( -1.000000000000000000, 5.665498452320000818E-16, 0.000000000000000000 ) ) ;
#25179 = CARTESIAN_POINT ( 'NONE',  ( 0.03533597110129999691, -28.50021994999999819, 223.9000014189999774 ) ) ;
#25180 = ORIENTED_EDGE ( 'NONE', *, *, #19270, .T. ) ;
#25181 = ORIENTED_EDGE ( 'NONE', *, *, #11873, .T. ) ;
#25182 = CARTESIAN_POINT ( 'NONE',  ( 23.83861932470720291, 15.61961844235199948, 5.310552110000033466 ) ) ;
#25183 = CARTESIAN_POINT ( 'NONE',  ( -8.903108651239966420, -22.82508830966961000, 140.0000000000000000 ) ) ;
#25184 = STYLED_ITEM ( 'NONE', ( #17615 ), #20871 ) ;
#25185 = ORIENTED_EDGE ( 'NONE', *, *, #23525, .T. ) ;
#25186 = CARTESIAN_POINT ( 'NONE',  ( -0.9568679087659598403, -3.500000000000000000, 227.7200428341212159 ) ) ;
#25187 = DIRECTION ( 'NONE',  ( 1.000000000000000000, 0.000000000000000000, -2.257150022439999944E-12 ) ) ;
#25188 = VERTEX_POINT ( 'NONE', #8134 ) ;
#25189 = CARTESIAN_POINT ( 'NONE',  ( -9.736208184377284525, -25.71890933281309444, 25.90207574972422577 ) ) ;
#25190 = ORIENTED_EDGE ( 'NONE', *, *, #25937, .F. ) ;
#25191 = ORIENTED_EDGE ( 'NONE', *, *, #26202, .T. ) ;
#25192 = SURFACE_STYLE_FILL_AREA ( #30222 ) ;
#25193 = EDGE_LOOP ( 'NONE', ( #14336, #25036, #20034 ) ) ;
#25194 = CARTESIAN_POINT ( 'NONE',  ( 24.38125476360000121, 13.54012337690000045, 230.6577119970000069 ) ) ;
#25195 = DIRECTION ( 'NONE',  ( 1.000000000000000000, 0.000000000000000000, 0.000000000000000000 ) ) ;
#25196 = CARTESIAN_POINT ( 'NONE',  ( 8.699999999550994900, -18.23122067933471158, -34.51216076559557422 ) ) ;
#25197 = CARTESIAN_POINT ( 'NONE',  ( 28.50000000000000000, 8.881784197000000993E-16, 222.0000000000000000 ) ) ;
#25198 = ADVANCED_FACE ( 'NONE', ( #626, #14932 ), #10833, .F. ) ;
#25199 = CARTESIAN_POINT ( 'NONE',  ( -24.54885679033566248, 13.04718334763902199, 6.002806401000010617 ) ) ;
#25200 = CARTESIAN_POINT ( 'NONE',  ( 3.043095095529606997, -3.198806979771088077, -95.69213427732501032 ) ) ;
#25201 = CARTESIAN_POINT ( 'NONE',  ( 9.219833965033643608, -25.90918750570072859, 205.5784319129419657 ) ) ;
#25202 = CARTESIAN_POINT ( 'NONE',  ( -27.15000000039999861, 3.324806250669999651E-15, 0.000000000000000000 ) ) ;
#25203 = ORIENTED_EDGE ( 'NONE', *, *, #7674, .F. ) ;
#25204 = AXIS2_PLACEMENT_3D ( 'NONE', #30494, #1848, #23101 ) ;
#25205 = CARTESIAN_POINT ( 'NONE',  ( -3.510061880997908279, 5.032561185093348044, -1.627651354100000169 ) ) ;
#25206 = CARTESIAN_POINT ( 'NONE',  ( -0.8316310374238428116, 4.718996048841939128, -18.89833244400000822 ) ) ;
#25207 = CARTESIAN_POINT ( 'NONE',  ( 2.290237947399999641, 7.805642660830000246, 227.7662452697800006 ) ) ;
#25208 = B_SPLINE_CURVE_WITH_KNOTS ( 'NONE', 1,
 ( #26840, #2775 ),
 .UNSPECIFIED., .F., .F.,
 ( 2, 2 ),
 ( -0.7000000000009999335, 0.002002273473630022949 ),
 .UNSPECIFIED. ) ;
#25209 = CARTESIAN_POINT ( 'NONE',  ( 24.36724931191508858, 13.38201648793566889, 5.145839562916747489 ) ) ;
#25210 = VECTOR ( 'NONE', #24586, 1000.000000000000000 ) ;
#25211 = CARTESIAN_POINT ( 'NONE',  ( -27.63177356790000161, 3.383804547869999678E-15, 137.3605236429999934 ) ) ;
#25212 = EDGE_CURVE ( 'NONE', #6605, #22456, #2969, .T. ) ;
#25213 = CARTESIAN_POINT ( 'NONE',  ( -26.58302938879999999, 9.294948734580000149, 230.5592437530000041 ) ) ;
#25214 = CARTESIAN_POINT ( 'NONE',  ( -28.49528339128749366, -0.5184828350247674411, 1.000000000000000888 ) ) ;
#25215 = DIRECTION ( 'NONE',  ( 0.000000000000000000, -1.000000000000000000, 0.000000000000000000 ) ) ;
#25216 = EDGE_CURVE ( 'NONE', #10061, #29716, #19404, .T. ) ;
#25217 = CARTESIAN_POINT ( 'NONE',  ( 24.33346004066275370, -12.81155130655225705, 224.7132485887567839 ) ) ;
#25218 = EDGE_CURVE ( 'NONE', #15990, #5093, #23543, .T. ) ;
#25219 = CARTESIAN_POINT ( 'NONE',  ( -19.80526803560000104, 19.50877411510000314, 228.1999999999999886 ) ) ;
#25220 = CARTESIAN_POINT ( 'NONE',  ( 13.67718073920000066, 20.99999999999999645, -57.16242423349999768 ) ) ;
#25221 = ORIENTED_EDGE ( 'NONE', *, *, #7083, .T. ) ;
#25222 = CARTESIAN_POINT ( 'NONE',  ( -3.552810942249358117, -4.212879106168850640, -58.37407541852499548 ) ) ;
#25223 = CARTESIAN_POINT ( 'NONE',  ( -23.90286779622075741, -15.52112778363645340, 5.560535487288766454 ) ) ;
#25224 = VERTEX_POINT ( 'NONE', #25628 ) ;
#25225 = EDGE_CURVE ( 'NONE', #9796, #27055, #25932, .T. ) ;
#25226 = CARTESIAN_POINT ( 'NONE',  ( 5.067327387632984959, 4.072231104569050686, -8.354586407999999409 ) ) ;
#25227 = VERTEX_POINT ( 'NONE', #1549 ) ;
#25228 = SHAPE_REPRESENTATION ( 'Handle Housing', ( #17722 ), #10330 ) ;
#25229 = CARTESIAN_POINT ( 'NONE',  ( -24.05205707537934856, 13.94194077903211593, 4.038530408134264782 ) ) ;
#25230 = CARTESIAN_POINT ( 'NONE',  ( 23.81866167241657806, 14.33570040768432996, 3.899998581000013509 ) ) ;
#25231 = VERTEX_POINT ( 'NONE', #23259 ) ;
#25232 = ORIENTED_EDGE ( 'NONE', *, *, #17499, .F. ) ;
#25233 = ORIENTED_EDGE ( 'NONE', *, *, #20793, .F. ) ;
#25234 = CARTESIAN_POINT ( 'NONE',  ( 9.999999999919999993, -25.00000000000000000, -4.837481085799996805 ) ) ;
#25235 = SURFACE_STYLE_FILL_AREA ( #20196 ) ;
#25236 = ORIENTED_EDGE ( 'NONE', *, *, #9471, .T. ) ;
#25237 = CARTESIAN_POINT ( 'NONE',  ( 9.993285220779503319, -25.61999708228222872, 193.6055512739999926 ) ) ;
#25238 = EDGE_CURVE ( 'NONE', #7991, #23341, #27650, .T. ) ;
#25239 = CARTESIAN_POINT ( 'NONE',  ( -8.699999999633703851, -22.22846246279628346, -40.15612242420909439 ) ) ;
#25240 = CARTESIAN_POINT ( 'NONE',  ( 3.916181512753878824, -4.480608557854155904, -64.01605006312500734 ) ) ;
#25241 = CARTESIAN_POINT ( 'NONE',  ( -10.69999999999960494, -29.15099216419329053, -26.30554312108708714 ) ) ;
#25242 = B_SPLINE_CURVE_WITH_KNOTS ( 'NONE', 5,
 ( #25162, #23128, #25482, #20279, #18063, #6114, #13042, #30033, #13355 ),
 .UNSPECIFIED., .F., .F.,
 ( 6, 3, 6 ),
 ( 0.000000000000000000, 53.95537973340000093, 92.42745556099998794 ),
 .UNSPECIFIED. ) ;
#25243 = APPLICATION_CONTEXT ( 'automotive_design' ) ;
#25244 = CARTESIAN_POINT ( 'NONE',  ( -28.54231846005005835, 4.391006012848424511, 0.5017677510000262409 ) ) ;
#25245 = CARTESIAN_POINT ( 'NONE',  ( 7.638687372290001498, 3.108070149090397472, -40.66397918109543497 ) ) ;
#25246 = LINE ( 'NONE', #29957, #23647 ) ;
#25247 = EDGE_CURVE ( 'NONE', #3948, #4408, #6975, .T. ) ;
#25248 = DIRECTION ( 'NONE',  ( 0.6343890248118320141, 0.7730139489027949562, 0.000000000000000000 ) ) ;
#25249 = ORIENTED_EDGE ( 'NONE', *, *, #908, .T. ) ;
#25250 = CARTESIAN_POINT ( 'NONE',  ( 3.619519562537643065, 2.908736503316577959, -8.354586408000006514 ) ) ;
#25251 = CARTESIAN_POINT ( 'NONE',  ( 16.59519732805809156, -8.049072271192613925, -4.336808689942017243E-16 ) ) ;
#25252 = CARTESIAN_POINT ( 'NONE',  ( 14.76039189740110658, -30.57853635232509504, -32.10743376547878825 ) ) ;
#25253 = VECTOR ( 'NONE', #19218, 1000.000000000000114 ) ;
#25254 = VERTEX_POINT ( 'NONE', #25304 ) ;
#25255 = CARTESIAN_POINT ( 'NONE',  ( 25.22625794089999829, -13.26224522399999906, 224.8958210039999983 ) ) ;
#25256 = CARTESIAN_POINT ( 'NONE',  ( 1.915963263359339530, -10.42012882710465682, -88.85875473022500159 ) ) ;
#25257 = CARTESIAN_POINT ( 'NONE',  ( 26.05511440539999768, -14.93230011240000010, 229.0000000000000000 ) ) ;
#25258 = CARTESIAN_POINT ( 'NONE',  ( 18.44984352795534832, 20.68448143878967826, 0.5514271650000068803 ) ) ;
#25259 = CARTESIAN_POINT ( 'NONE',  ( 0.000000000000000000, 0.000000000000000000, 40.00000000000000000 ) ) ;
#25260 = CARTESIAN_POINT ( 'NONE',  ( -3.794322484923305705, -3.503605959878534293, -44.22295181582499168 ) ) ;
#25261 = CARTESIAN_POINT ( 'NONE',  ( -11.48163258379999974, -24.28840542069999842, -1.419991652300001128 ) ) ;
#25262 = CARTESIAN_POINT ( 'NONE',  ( 23.06578384731929532, -13.64653153667426544, 223.9278743037292543 ) ) ;
#25263 = ORIENTED_EDGE ( 'NONE', *, *, #13506, .F. ) ;
#25264 = FILL_AREA_STYLE_COLOUR ( '', #18296 ) ;
#25265 = CARTESIAN_POINT ( 'NONE',  ( 22.83442928010000017, 16.43389279790000046, 224.8000000000000114 ) ) ;
#25266 = CARTESIAN_POINT ( 'NONE',  ( 2.842970026702535513, -3.450524644270692498, -68.10000000002500542 ) ) ;
#25267 = CARTESIAN_POINT ( 'NONE',  ( 0.8926240813841433974, -3.415131430869944307, -0.6999999999999784173 ) ) ;
#25268 = CARTESIAN_POINT ( 'NONE',  ( -4.123648947899040351, -0.09406098493378543812, -44.10000000002499121 ) ) ;
#25269 = SURFACE_STYLE_FILL_AREA ( #8572 ) ;
#25270 = DIRECTION ( 'NONE',  ( -0.000000000000000000, 0.5000000000001900702, 0.8660254037843290176 ) ) ;
#25271 = DIRECTION ( 'NONE',  ( 0.000000000000000000, 0.000000000000000000, 1.000000000000000000 ) ) ;
#25272 = EDGE_CURVE ( 'NONE', #29062, #17095, #30656, .T. ) ;
#25273 = CARTESIAN_POINT ( 'NONE',  ( 4.883349601227576997, 0.1168011502185872796, -64.06686508972499894 ) ) ;
#25274 = ORIENTED_EDGE ( 'NONE', *, *, #27749, .T. ) ;
#25275 = CARTESIAN_POINT ( 'NONE',  ( 20.19118761472760326, 19.99999729016618133, 229.5203474167158504 ) ) ;
#25276 = EDGE_CURVE ( 'NONE', #30960, #4760, #6777, .T. ) ;
#25277 = ORIENTED_EDGE ( 'NONE', *, *, #15798, .T. ) ;
#25278 = EDGE_CURVE ( 'NONE', #20192, #23233, #27252, .T. ) ;
#25279 = CARTESIAN_POINT ( 'NONE',  ( -4.549046388969006038, -30.14545866191155810, 0.02487508500001456291 ) ) ;
#25280 = EDGE_CURVE ( 'NONE', #20223, #23118, #13970, .T. ) ;
#25281 = VERTEX_POINT ( 'NONE', #16165 ) ;
#25282 = LINE ( 'NONE', #4036, #998 ) ;
#25283 = CARTESIAN_POINT ( 'NONE',  ( 26.05511440539999768, -14.93230011240000010, 229.0000000000000000 ) ) ;
#25284 = CARTESIAN_POINT ( 'NONE',  ( -3.063912144317538111, 1.789060389098976911, 0.000000000000000000 ) ) ;
#25285 = CARTESIAN_POINT ( 'NONE',  ( 26.80000000000000071, 7.105427357599999217E-15, 36.78285841090000474 ) ) ;
#25286 = CARTESIAN_POINT ( 'NONE',  ( -12.67459614424639902, -22.00000000000000355, -25.78755258470928524 ) ) ;
#25287 = DIRECTION ( 'NONE',  ( 1.000000000000000000, 0.000000000000000000, 0.000000000000000000 ) ) ;
#25288 = ORIENTED_EDGE ( 'NONE', *, *, #2689, .T. ) ;
#25289 = CARTESIAN_POINT ( 'NONE',  ( 28.49528339128749366, 0.5184828350247835393, 8.000000000000007105 ) ) ;
#25290 = DIRECTION ( 'NONE',  ( 0.3633921898465272138, -0.9316362575375356503, -4.625929269271483744E-15 ) ) ;
#25291 = CIRCLE ( 'NONE', #14246, 1.472846691535505848 ) ;
#25292 = CARTESIAN_POINT ( 'NONE',  ( 1.755400582548710009, -3.970618665040213546, -70.32351655465652129 ) ) ;
#25293 = CARTESIAN_POINT ( 'NONE',  ( -2.656431219428132096, -2.398832595398723289, 230.7906780663903703 ) ) ;
#25294 = DIRECTION ( 'NONE',  ( -0.7071067811898219535, 0.2886612846638016983, 0.6455034180634624530 ) ) ;
#25295 =( GEOMETRIC_REPRESENTATION_CONTEXT ( 3 ) GLOBAL_UNCERTAINTY_ASSIGNED_CONTEXT ( ( #12825 ) ) GLOBAL_UNIT_ASSIGNED_CONTEXT ( ( #3705, #1357, #30302 ) ) REPRESENTATION_CONTEXT ( 'NONE', 'WORKASPACE' ) );
#25296 = DIRECTION ( 'NONE',  ( -1.000000000000000000, 0.000000000000000000, 0.000000000000000000 ) ) ;
#25297 = ADVANCED_BREP_SHAPE_REPRESENTATION ( '', ( #890, #17722 ), #11232 ) ;
#25298 = AXIS2_PLACEMENT_3D ( 'NONE', #5163, #16816, #12710 ) ;
#25299 = CARTESIAN_POINT ( 'NONE',  ( 9.999999999973411491, -24.37864083538289250, -29.91085694194880773 ) ) ;
#25300 = CARTESIAN_POINT ( 'NONE',  ( -17.86780073576266759, 11.40100527483982873, -1.400000000000001910 ) ) ;
#25301 = CARTESIAN_POINT ( 'NONE',  ( 5.782578939028539367, 2.564649547393091478, -51.39998794302498908 ) ) ;
#25302 = DIRECTION ( 'NONE',  ( 1.000000000000000000, 0.000000000000000000, 0.000000000000000000 ) ) ;
#25303 = CARTESIAN_POINT ( 'NONE',  ( 6.726015838937449587, -25.94607852067420595, 208.3934793376300547 ) ) ;
#25304 = CARTESIAN_POINT ( 'NONE',  ( 10.70000000009999930, -30.17682926915999886, -28.39999999989999679 ) ) ;
#25305 = CARTESIAN_POINT ( 'NONE',  ( -0.1113126277254997409, 0.6198477072577868174, -37.78148909789995002 ) ) ;
#25306 = CARTESIAN_POINT ( 'NONE',  ( -8.424250880209998925E-16, -2.000000000000000000, 230.8412452700000017 ) ) ;
#25307 = ORIENTED_EDGE ( 'NONE', *, *, #20885, .F. ) ;
#25308 = CARTESIAN_POINT ( 'NONE',  ( 3.503437880484509659, 2.636891074944046398, -32.36032172559999509 ) ) ;
#25309 = ORIENTED_EDGE ( 'NONE', *, *, #25216, .F. ) ;
#25310 = DIRECTION ( 'NONE',  ( -1.000000000000000000, 0.000000000000000000, 0.000000000000000000 ) ) ;
#25311 = CARTESIAN_POINT ( 'NONE',  ( 3.630871288588910506, -4.685987307826644965, -52.50430438132499944 ) ) ;
#25312 = AXIS2_PLACEMENT_3D ( 'NONE', #28007, #16052, #4093 ) ;
#25313 = ORIENTED_EDGE ( 'NONE', *, *, #25056, .F. ) ;
#25314 = AXIS2_PLACEMENT_3D ( 'NONE', #7676, #21705, #22022 ) ;
#25315 = PRODUCT_CONTEXT ( 'NONE', #25243, 'mechanical' ) ;
#25316 = ORIENTED_EDGE ( 'NONE', *, *, #28426, .T. ) ;
#25317 = ORIENTED_EDGE ( 'NONE', *, *, #11164, .T. ) ;
#25318 = CARTESIAN_POINT ( 'NONE',  ( 24.34942395458080000, 13.41447635809142724, 4.689458287000014991 ) ) ;
#25319 = CARTESIAN_POINT ( 'NONE',  ( -12.29999999969999891, -27.00000000000000000, -28.40000000020000215 ) ) ;
#25320 = CARTESIAN_POINT ( 'NONE',  ( -10.00000000000000000, -130.0000000000000000, -42.39999999999999858 ) ) ;
#25321 = LINE ( 'NONE', #15405, #4402 ) ;
#25322 = CARTESIAN_POINT ( 'NONE',  ( -0.8471243407022264194, -27.48706736360457015, 4.296916151638034975 ) ) ;
#25323 = CARTESIAN_POINT ( 'NONE',  ( -17.14079338756361892, 12.06595463930550238, -4.336808689942018722E-16 ) ) ;
#25324 = CARTESIAN_POINT ( 'NONE',  ( -2.507187057889194381, 3.594686560818127763, -1.627651354100000169 ) ) ;
#25325 = CARTESIAN_POINT ( 'NONE',  ( 12.22909344072123439, 26.04501283290617764, -59.39872012669144397 ) ) ;
#25326 = CARTESIAN_POINT ( 'NONE',  ( -1.419173372180000084E-06, -27.80022181310000207, 223.9000014189999774 ) ) ;
#25327 = VERTEX_POINT ( 'NONE', #27811 ) ;
#25328 = CARTESIAN_POINT ( 'NONE',  ( -2.929853409778804263, 3.622264489389753539, -14.10352819870000829 ) ) ;
#25329 = CARTESIAN_POINT ( 'NONE',  ( 6.081417161111781766, 6.156119086796980611, -40.48170906884572418 ) ) ;
#25330 = DIRECTION ( 'NONE',  ( 0.2815395311429196301, 0.9595496299847262600, 0.000000000000000000 ) ) ;
#25331 = EDGE_CURVE ( 'NONE', #5639, #1757, #28374, .T. ) ;
#25332 = CARTESIAN_POINT ( 'NONE',  ( -24.14787428015092274, -13.77541660134580326, 226.1000014189999376 ) ) ;
#25333 = CARTESIAN_POINT ( 'NONE',  ( -2.605043309123956430, -2.487932632674070721, 227.7052921205641098 ) ) ;
#25334 = AXIS2_PLACEMENT_3D ( 'NONE', #17880, #8438, #13017 ) ;
#25335 = CARTESIAN_POINT ( 'NONE',  ( -27.90784132687080898, -6.416341681828127363, 8.000000000000007105 ) ) ;
#25336 = CARTESIAN_POINT ( 'NONE',  ( 4.175165894169885483, -119.7166638525666826, -63.39999999999999858 ) ) ;
#25337 = AXIS2_PLACEMENT_3D ( 'NONE', #23806, #13893, #21439 ) ;
#25338 = CIRCLE ( 'NONE', #19322, 3.000000000000001332 ) ;
#25339 = CARTESIAN_POINT ( 'NONE',  ( 19.80538173989999962, 19.50875420239999869, 227.3999999149999951 ) ) ;
#25340 = DIRECTION ( 'NONE',  ( -0.9880370573969196046, 0.1542166437529879364, 0.000000000000000000 ) ) ;
#25341 = CARTESIAN_POINT ( 'NONE',  ( 0.000000000000000000, 0.000000000000000000, 227.6412452697800006 ) ) ;
#25342 = ORIENTED_EDGE ( 'NONE', *, *, #23946, .F. ) ;
#25343 = ORIENTED_EDGE ( 'NONE', *, *, #13369, .T. ) ;
#25344 = EDGE_CURVE ( 'NONE', #13298, #28330, #631, .T. ) ;
#25345 = DIRECTION ( 'NONE',  ( 0.000000000000000000, 0.000000000000000000, -1.000000000000000000 ) ) ;
#25346 = CARTESIAN_POINT ( 'NONE',  ( 2.605017075358218470, 2.487964477257813112, 230.7771899713955293 ) ) ;
#25347 = ORIENTED_EDGE ( 'NONE', *, *, #20417, .T. ) ;
#25348 = DIRECTION ( 'NONE',  ( -2.764840495839172918E-12, -0.9128796883888953273, 0.4082287037029531107 ) ) ;
#25349 = CARTESIAN_POINT ( 'NONE',  ( 2.167139767879371348, -2.450417181414907386, -36.28402085616472306 ) ) ;
#25350 = CARTESIAN_POINT ( 'NONE',  ( -0.08587345398629391002, -5.205186680070521987, -0.7000563607978648184 ) ) ;
#25351 = STYLED_ITEM ( 'NONE', ( #18497 ), #15531 ) ;
#25352 = ORIENTED_EDGE ( 'NONE', *, *, #7842, .F. ) ;
#25353 = CARTESIAN_POINT ( 'NONE',  ( -16.85343921402336775, -7.900182044543379689, -0.6999999989999727834 ) ) ;
#25354 = EDGE_LOOP ( 'NONE', ( #4227, #30932, #20711, #26591 ) ) ;
#25355 = VERTEX_POINT ( 'NONE', #12067 ) ;
#25356 = ORIENTED_EDGE ( 'NONE', *, *, #19819, .T. ) ;
#25357 = CARTESIAN_POINT ( 'NONE',  ( 18.34692404780000174, 20.56908522520000204, 230.5592437530000041 ) ) ;
#25358 = VECTOR ( 'NONE', #30208, 1000.000000000000000 ) ;
#25359 = EDGE_LOOP ( 'NONE', ( #11430, #7046, #10306, #25029 ) ) ;
#25361 = CARTESIAN_POINT ( 'NONE',  ( -24.09302906149999757, -13.87041066189999938, 226.1000014189999945 ) ) ;
#25360 = AXIS2_PLACEMENT_3D ( 'NONE', #1148, #17961, #13097 ) ;
#25362 = ORIENTED_EDGE ( 'NONE', *, *, #18671, .T. ) ;
#25363 = CARTESIAN_POINT ( 'NONE',  ( 0.000000000000000000, 0.000000000000000000, 115.0000000000000000 ) ) ;
#25364 = VECTOR ( 'NONE', #24140, 1000.000000000000000 ) ;
#25365 = AXIS2_PLACEMENT_3D ( 'NONE', #24711, #19987, #5509 ) ;
#25366 = FACE_OUTER_BOUND ( 'NONE', #4949, .T. ) ;
#25367 = CARTESIAN_POINT ( 'NONE',  ( 2.107992564109752998, -27.41908764619381245, 210.0000000000000284 ) ) ;
#25368 = CARTESIAN_POINT ( 'NONE',  ( 2.876933567438932027, -2.017004891198901362, 227.6466876223813927 ) ) ;
#25369 = EDGE_CURVE ( 'NONE', #3826, #1366, #23889, .T. ) ;
#25370 = CARTESIAN_POINT ( 'NONE',  ( 23.99428763615714644, -14.04082805276427592, 4.114052333822514562 ) ) ;
#25371 = VERTEX_POINT ( 'NONE', #14124 ) ;
#25372 = CARTESIAN_POINT ( 'NONE',  ( 4.360957369889332469, -0.1505632777267530420, -3.185409721200004984 ) ) ;
#25373 = CARTESIAN_POINT ( 'NONE',  ( 3.375516224911112584, -2.766870103071181308, -23.99674734060000603 ) ) ;
#25374 = CARTESIAN_POINT ( 'NONE',  ( -3.938336462418404516, -27.21777852796477504, 209.8041027071180338 ) ) ;
#25375 = VECTOR ( 'NONE', #7210, 1000.000000000000000 ) ;
#25376 = CARTESIAN_POINT ( 'NONE',  ( 24.83272649506304219, -12.49791454618707398, 5.208434320000010942 ) ) ;
#25377 = STYLED_ITEM ( 'NONE', ( #28820 ), #17428 ) ;
#25378 = CARTESIAN_POINT ( 'NONE',  ( -1.687520611373146684, -3.681674406733895122, -91.97391714452653844 ) ) ;
#25379 = CARTESIAN_POINT ( 'NONE',  ( -27.04662643769999875, 9.457048792620000199, 230.2432540810000319 ) ) ;
#25380 = CARTESIAN_POINT ( 'NONE',  ( 17.73945528731000110, 10.04965037119602655, -0.6999999999999784173 ) ) ;
#25381 = CARTESIAN_POINT ( 'NONE',  ( -24.68204616399999907, -14.25020164319999871, 226.1000014189999945 ) ) ;
#25382 = CARTESIAN_POINT ( 'NONE',  ( -17.78291068004000053, 10.42683423967575251, -0.000000000000000000 ) ) ;
#25383 = CARTESIAN_POINT ( 'NONE',  ( 0.000000000000000000, 0.000000000000000000, 115.0000000000000000 ) ) ;
#25384 = CARTESIAN_POINT ( 'NONE',  ( 6.438687372205746051, -7.245008774379918748, -33.94554228741176161 ) ) ;
#25385 = VERTEX_POINT ( 'NONE', #26543 ) ;
#25386 = CARTESIAN_POINT ( 'NONE',  ( -0.05440858064702409902, 4.649678238646714590, -56.56818518972501408 ) ) ;
#25387 = CARTESIAN_POINT ( 'NONE',  ( -24.06001628199535247, -15.27670956567710192, 5.888744255995201904 ) ) ;
#25388 = ORIENTED_EDGE ( 'NONE', *, *, #1054, .T. ) ;
#25389 = VECTOR ( 'NONE', #23660, 1000.000000000000000 ) ;
#25390 = ADVANCED_FACE ( 'NONE', ( #4838 ), #14595, .F. ) ;
#25391 = CARTESIAN_POINT ( 'NONE',  ( -3.360743903619262340, -4.083497937754941631, -0.7578093794999990473 ) ) ;
#25392 = ORIENTED_EDGE ( 'NONE', *, *, #19351, .F. ) ;
#25393 = CARTESIAN_POINT ( 'NONE',  ( 23.55447120710000064, 16.04539730700000177, 222.0000000000000000 ) ) ;
#25394 = CARTESIAN_POINT ( 'NONE',  ( -3.686970300939999667, 0.4978338539504151838, -70.82548838946271985 ) ) ;
#25395 = ORIENTED_EDGE ( 'NONE', *, *, #22969, .F. ) ;
#25396 = CARTESIAN_POINT ( 'NONE',  ( 10.95110162350000138, 19.99999999999999645, -1.734685620000002482 ) ) ;
#25397 = VERTEX_POINT ( 'NONE', #12215 ) ;
#25398 = ORIENTED_EDGE ( 'NONE', *, *, #6885, .F. ) ;
#25399 = CARTESIAN_POINT ( 'NONE',  ( -10.69999999999999929, -120.0000000000000000, -41.24671599700000257 ) ) ;
#25400 = ORIENTED_EDGE ( 'NONE', *, *, #12156, .F. ) ;
#25401 = DIRECTION ( 'NONE',  ( -1.000000000000000000, 0.000000000000000000, 0.000000000000000000 ) ) ;
#25402 = VECTOR ( 'NONE', #1137, 1000.000000000000000 ) ;
#25403 = AXIS2_PLACEMENT_3D ( 'NONE', #27358, #22336, #27053 ) ;
#25404 = CARTESIAN_POINT ( 'NONE',  ( -8.699999999638116321, -22.83323352287542463, -39.84673049988318638 ) ) ;
#25405 = EDGE_CURVE ( 'NONE', #1319, #7041, #24033, .T. ) ;
#25406 = CARTESIAN_POINT ( 'NONE',  ( -5.296314592117303377, -2.692763687817543161, -62.36424626872499033 ) ) ;
#25407 = CARTESIAN_POINT ( 'NONE',  ( -27.24857305700000154, -10.01116691310000029, 229.9172022069999741 ) ) ;
#25408 = EDGE_CURVE ( 'NONE', #25870, #11151, #9552, .T. ) ;
#25409 = CARTESIAN_POINT ( 'NONE',  ( -20.30396346370000060, 20.00000000000000000, 227.0000000000000000 ) ) ;
#25410 = FACE_OUTER_BOUND ( 'NONE', #24040, .T. ) ;
#25411 = CARTESIAN_POINT ( 'NONE',  ( -17.40256142130785832, -23.40875500259708986, -24.69991345770832680 ) ) ;
#25412 = ORIENTED_EDGE ( 'NONE', *, *, #18275, .F. ) ;
#25413 = CARTESIAN_POINT ( 'NONE',  ( -10.00000000070000183, -25.00000000000000000, -26.16393202249999916 ) ) ;
#25414 = PRODUCT_DEFINITION_CONTEXT ( 'detailed design', #9379, 'design' ) ;
#25415 = EDGE_CURVE ( 'NONE', #8936, #21696, #27632, .T. ) ;
#25416 = CARTESIAN_POINT ( 'NONE',  ( 4.310466091822801715, 1.786666325167806546, -10.99261350020000982 ) ) ;
#25417 = FACE_OUTER_BOUND ( 'NONE', #18570, .T. ) ;
#25418 = PRODUCT ( 'Rear Frame Plate', 'Rear Frame Plate', '', ( #27981 ) ) ;
#25419 = CARTESIAN_POINT ( 'NONE',  ( 14.80686173019985219, -30.24862743399516063, -32.29790676828473295 ) ) ;
#25420 = ORIENTED_EDGE ( 'NONE', *, *, #3808, .T. ) ;
#25421 = DIRECTION ( 'NONE',  ( -1.635844237846128888E-12, 0.6889064844488322903, -0.7248502298298253876 ) ) ;
#25422 = CARTESIAN_POINT ( 'NONE',  ( -24.14840830027149465, -13.77363891140888619, 5.901294544000013076 ) ) ;
#25423 = DIRECTION ( 'NONE',  ( 0.7071067811865469066, -0.6644630243886066046, -0.2418447626481643187 ) ) ;
#25424 = CARTESIAN_POINT ( 'NONE',  ( 27.71261514784184499, 0.5042418799608394675, 0.5514269430000329208 ) ) ;
#25425 = DIRECTION ( 'NONE',  ( -3.924189347185962345E-12, 0.4082287037029530552, 0.9128796883888953273 ) ) ;
#25426 = CARTESIAN_POINT ( 'NONE',  ( -5.939015604524707115, -0.1501891088408410790, -53.55673954922500002 ) ) ;
#25427 = EDGE_CURVE ( 'NONE', #21489, #24348, #21238, .T. ) ;
#25428 = CYLINDRICAL_SURFACE ( 'NONE', #23867, 2.000000000000002665 ) ;
#25429 = CARTESIAN_POINT ( 'NONE',  ( 22.92720033239275068, -13.87810118103447543, 224.0393715186460213 ) ) ;
#25430 = PRODUCT_DEFINITION_FORMATION_WITH_SPECIFIED_SOURCE ( 'ANY', '', #6042, .NOT_KNOWN. ) ;
#25431 = VERTEX_POINT ( 'NONE', #28901 ) ;
#25432 = CARTESIAN_POINT ( 'NONE',  ( 23.83006841374216833, -14.31758446293960141, 4.492876031999992748 ) ) ;
#25433 = CARTESIAN_POINT ( 'NONE',  ( 22.83442928010000017, 16.43389279790000046, 223.3999999999999773 ) ) ;
#25434 = CARTESIAN_POINT ( 'NONE',  ( 2.826807023972331745, -3.676508995340744157, -68.10000000002501963 ) ) ;
#25435 = EDGE_CURVE ( 'NONE', #5339, #17343, #2841, .T. ) ;
#25436 = CARTESIAN_POINT ( 'NONE',  ( 3.496762477039628614, -0.4822370993093180735, -0.6999999999999784173 ) ) ;
#25437 = CARTESIAN_POINT ( 'NONE',  ( -12.75378086759999796, -27.00000000059169736, -22.62649730796000114 ) ) ;
#25438 = CARTESIAN_POINT ( 'NONE',  ( 14.73716614373068801, -25.71543255174850984, -33.43156970936686889 ) ) ;
#25439 = CARTESIAN_POINT ( 'NONE',  ( -9.961462390591020011, -7.265484932597956913, 232.6627637660201628 ) ) ;
#25440 = CARTESIAN_POINT ( 'NONE',  ( -4.568101251964848508, -0.2431723019727845825, -65.96421022022501290 ) ) ;
#25441 = ORIENTED_EDGE ( 'NONE', *, *, #16079, .F. ) ;
#25442 = CARTESIAN_POINT ( 'NONE',  ( -8.699999999737658030, -25.77531388886905006, -25.66136093486021608 ) ) ;
#25443 = ORIENTED_EDGE ( 'NONE', *, *, #27977, .T. ) ;
#25444 = CARTESIAN_POINT ( 'NONE',  ( 3.373344672752164985, -1.082959996301563477, -88.52261276311425320 ) ) ;
#25445 = VERTEX_POINT ( 'NONE', #14743 ) ;
#25446 = CARTESIAN_POINT ( 'NONE',  ( 24.64642659020000082, -14.31106159850000026, 226.0986569330000293 ) ) ;
#25447 = CARTESIAN_POINT ( 'NONE',  ( -23.87963657974984955, -15.55698410977798929, 4.493007575000013354 ) ) ;
#25448 = CARTESIAN_POINT ( 'NONE',  ( -8.699999999663262429, -18.45724128289285204, -35.79059583716231430 ) ) ;
#25449 = CARTESIAN_POINT ( 'NONE',  ( -3.511914029060239528, -0.9171864698486590362, 230.7613442533420596 ) ) ;
#25450 = CARTESIAN_POINT ( 'NONE',  ( -22.97593508925929129, 15.65128309461163703, 8.000000000000007105 ) ) ;
#25451 = CARTESIAN_POINT ( 'NONE',  ( -12.39224864152920880, -22.00000000000000000, -29.62605183290172306 ) ) ;
#25452 = CARTESIAN_POINT ( 'NONE',  ( 9.799999999988044053, -17.90599344469555732, -35.94535904307270613 ) ) ;
#25453 = ORIENTED_EDGE ( 'NONE', *, *, #29536, .T. ) ;
#25454 = CARTESIAN_POINT ( 'NONE',  ( -28.49528339128749366, -0.5184828350247786544, 8.000000000000007105 ) ) ;
#25455 = CARTESIAN_POINT ( 'NONE',  ( 24.18069373756728524, 13.78367726165553009, 8.000000000000007105 ) ) ;
#25456 = CARTESIAN_POINT ( 'NONE',  ( -1.419173393149999842E-06, -27.80022181310000207, 226.1000014189999945 ) ) ;
#25457 = DIRECTION ( 'NONE',  ( 1.000000000000000000, 0.000000000000000000, 0.000000000000000000 ) ) ;
#25458 = LINE ( 'NONE', #9074, #13664 ) ;
#25459 = CARTESIAN_POINT ( 'NONE',  ( 19.80538173989999962, 19.50875420239999869, 228.1999999569999886 ) ) ;
#25460 = ADVANCED_FACE ( 'NONE', ( #19150 ), #28740, .F. ) ;
#25461 = FACE_OUTER_BOUND ( 'NONE', #2525, .T. ) ;
#25462 = CARTESIAN_POINT ( 'NONE',  ( 0.9498610579744216631, -27.78396626330503594, 224.4416736066579858 ) ) ;
#25463 = CARTESIAN_POINT ( 'NONE',  ( 0.8648632234848976363, -6.342619565911398638, -49.28468436622499382 ) ) ;
#25464 = EDGE_CURVE ( 'NONE', #28983, #10752, #26693, .T. ) ;
#25465 = ADVANCED_FACE ( 'NONE', ( #2783 ), #3345, .T. ) ;
#25466 = CARTESIAN_POINT ( 'NONE',  ( 0.000000000000000000, 0.000000000000000000, 231.1412452697749984 ) ) ;
#25467 = CARTESIAN_POINT ( 'NONE',  ( 6.760007715859398303, 5.672256964398498802, -40.24571374337934770 ) ) ;
#25468 = DIRECTION ( 'NONE',  ( -0.1090476345695678556, -0.6986477033489640887, -0.7071067811865475727 ) ) ;
#25469 = CARTESIAN_POINT ( 'NONE',  ( -4.175165894169885483, -50.49316738903675628, -63.39999999999999858 ) ) ;
#25470 = ORIENTED_EDGE ( 'NONE', *, *, #19444, .F. ) ;
#25471 = CARTESIAN_POINT ( 'NONE',  ( 0.09516252086846690994, -5.505278045713965618, -34.41110030500000505 ) ) ;
#25472 = VERTEX_POINT ( 'NONE', #15776 ) ;
#25473 = CARTESIAN_POINT ( 'NONE',  ( 3.599561039400463347, 4.779710538180673041, -54.62619010302499589 ) ) ;
#25474 = ORIENTED_EDGE ( 'NONE', *, *, #3129, .F. ) ;
#25475 = SHAPE_DEFINITION_REPRESENTATION ( #25140, #19621 ) ;
#25476 = ORIENTED_EDGE ( 'NONE', *, *, #31079, .T. ) ;
#25477 = ORIENTED_EDGE ( 'NONE', *, *, #10860, .T. ) ;
#25478 = CARTESIAN_POINT ( 'NONE',  ( 14.54659216920487452, -27.45739552686597307, -22.89087251491314845 ) ) ;
#25479 = FACE_OUTER_BOUND ( 'NONE', #30618, .T. ) ;
#25480 = CARTESIAN_POINT ( 'NONE',  ( -9.999999999539999962, -130.0000000000000000, -42.53299740480396451 ) ) ;
#25481 = TOROIDAL_SURFACE ( 'NONE', #11907, 30.50000000000000000, 3.000000000000000000 ) ;
#25482 = CARTESIAN_POINT ( 'NONE',  ( -23.10935684540000068, -20.42749692129999772, 222.0000000000000000 ) ) ;
#25483 = B_SPLINE_CURVE_WITH_KNOTS ( 'NONE', 3,
 ( #11837, #1619, #27890, #18753, #11370, #6334 ),
 .UNSPECIFIED., .F., .F.,
 ( 4, 2, 4 ),
 ( 0.000000000000000000, 0.5000000000000000000, 1.000000000000000000 ),
 .UNSPECIFIED. ) ;
#25484 = CARTESIAN_POINT ( 'NONE',  ( -16.06988921239048551, -8.208160914692745891, -0.6999999999999784173 ) ) ;
#25485 = DIRECTION ( 'NONE',  ( 1.000000000000000000, 0.000000000000000000, 0.000000000000000000 ) ) ;
#25486 = CARTESIAN_POINT ( 'NONE',  ( 1.334940606749785319, 4.973974987606708531, -1.115910702900006601 ) ) ;
#25487 = CARTESIAN_POINT ( 'NONE',  ( 0.5204573308370086249, -1.949186941335384837, 230.8412452700000301 ) ) ;
#25488 = DIRECTION ( 'NONE',  ( 0.8086898285215826654, 0.000000000000000000, 0.5882352941176968164 ) ) ;
#25489 = CARTESIAN_POINT ( 'NONE',  ( -4.706847372945446750, -0.8873292358359263776, -17.03699426529999883 ) ) ;
#25490 = CARTESIAN_POINT ( 'NONE',  ( -6.074876045044606876, 0.8789665559579967757, -33.65783976330000371 ) ) ;
#25491 = CARTESIAN_POINT ( 'NONE',  ( -13.88844840186909302, 21.69999999999906137, -57.58021927548519869 ) ) ;
#25492 = LINE ( 'NONE', #4086, #15817 ) ;
#25493 = CARTESIAN_POINT ( 'NONE',  ( 0.2402089773159999941, -27.79941220630000132, 223.9202078600000050 ) ) ;
#25494 = CARTESIAN_POINT ( 'NONE',  ( -7.999999999627648961, -16.75972747693622722, -40.88001126969393084 ) ) ;
#25495 = CARTESIAN_POINT ( 'NONE',  ( -20.30403093158959038, 20.00000000003189626, 0.8742661550000252468 ) ) ;
#25496 = EDGE_CURVE ( 'NONE', #21685, #23963, #15946, .T. ) ;
#25497 = CARTESIAN_POINT ( 'NONE',  ( 25.33584480268451600, 14.29478671887457608, 0.7595836940000044724 ) ) ;
#25498 = CARTESIAN_POINT ( 'NONE',  ( -23.48532358956344623, -12.91116100318319937, 4.042547419098327488 ) ) ;
#25499 = CARTESIAN_POINT ( 'NONE',  ( 8.700000000237981368, -29.94290473664190699, -29.10277714274672434 ) ) ;
#25500 = ADVANCED_FACE ( 'NONE', ( #28204 ), #23504, .F. ) ;
#25501 = VERTEX_POINT ( 'NONE', #30728 ) ;
#25502 = STYLED_ITEM ( 'NONE', ( #3478 ), #10658 ) ;
#25503 = CARTESIAN_POINT ( 'NONE',  ( 10.14902473071355793, -26.01926976408357817, 92.06031501460000754 ) ) ;
#25504 = EDGE_LOOP ( 'NONE', ( #6877, #30661, #5266, #15772 ) ) ;
#25505 = AXIS2_PLACEMENT_3D ( 'NONE', #9250, #21222, #16343 ) ;
#25506 = CARTESIAN_POINT ( 'NONE',  ( -23.20948082139999968, -13.40000000000000036, 223.8999999999999773 ) ) ;
#25507 = CARTESIAN_POINT ( 'NONE',  ( -25.11765555659999904, -13.46780168200000105, 224.3191686030000369 ) ) ;
#25508 = CARTESIAN_POINT ( 'NONE',  ( -0.7723098159415937580, -5.165446492250387323, -0.7000230395128266281 ) ) ;
#25509 = ORIENTED_EDGE ( 'NONE', *, *, #30008, .T. ) ;
#25510 = B_SPLINE_CURVE_WITH_KNOTS ( 'NONE', 3,
 ( #12406, #14626, #24215, #2657, #10057, #14473 ),
 .UNSPECIFIED., .F., .F.,
 ( 4, 2, 4 ),
 ( 0.000000000000000000, 0.5000000000000000000, 1.000000000000000000 ),
 .UNSPECIFIED. ) ;
#25511 = DIRECTION ( 'NONE',  ( 0.3633921898465273803, -0.9316362575375355393, 0.000000000000000000 ) ) ;
#25512 = ORIENTED_EDGE ( 'NONE', *, *, #6981, .T. ) ;
#25513 = ORIENTED_EDGE ( 'NONE', *, *, #18281, .F. ) ;
#25514 = PRODUCT_CONTEXT ( 'NONE', #23649, 'mechanical' ) ;
#25515 = EDGE_LOOP ( 'NONE', ( #6553, #23050, #3380, #9282, #21243 ) ) ;
#25516 = CARTESIAN_POINT ( 'NONE',  ( 18.97091807949999875, 21.26865672099999927, 229.0000000000000000 ) ) ;
#25517 = EDGE_LOOP ( 'NONE', ( #7437, #29750, #24354, #6580 ) ) ;
#25518 = DIRECTION ( 'NONE',  ( -1.000000000000000000, 5.687697999151106851E-16, -6.771501495036750356E-12 ) ) ;
#25519 = CARTESIAN_POINT ( 'NONE',  ( 8.000000000276081380, -16.84112630282697154, -33.19732204816383359 ) ) ;
#25520 = CARTESIAN_POINT ( 'NONE',  ( 3.163495726740022551, 2.135910292705673452, -35.69999999999998863 ) ) ;
#25521 = CARTESIAN_POINT ( 'NONE',  ( 0.4831567132674381426, -28.49614615030699838, 3.899998581000013509 ) ) ;
#25522 = CARTESIAN_POINT ( 'NONE',  ( 25.66636617707885648, -7.791308912181349022, -1.399999999999998357 ) ) ;
#25523 = CARTESIAN_POINT ( 'NONE',  ( -10.69999999996928963, -30.00000000000001066, -28.79379052075074696 ) ) ;
#25524 = CARTESIAN_POINT ( 'NONE',  ( -1.127665019380000189, -28.47796022459999676, 225.1040592169999854 ) ) ;
#25525 = VERTEX_POINT ( 'NONE', #21283 ) ;
#25526 = ADVANCED_FACE ( 'NONE', ( #9316 ), #16553, .F. ) ;
#25527 = CARTESIAN_POINT ( 'NONE',  ( -6.505526340832360255, -0.4164809035307331930, -4.148838774900000637 ) ) ;
#25528 = CARTESIAN_POINT ( 'NONE',  ( -3.579388909039125988, -3.189794392837340009, -23.90351932450001016 ) ) ;
#25529 = CARTESIAN_POINT ( 'NONE',  ( -9.509259942401930843, -25.80376675868339120, 204.8434573210849692 ) ) ;
#25530 = AXIS2_PLACEMENT_3D ( 'NONE', #18499, #8736, #8894 ) ;
#25531 = AXIS2_PLACEMENT_3D ( 'NONE', #6834, #4170, #13762 ) ;
#25532 = CARTESIAN_POINT ( 'NONE',  ( -9.000000000229999131, 20.99999999999999645, -51.10000000000000142 ) ) ;
#25533 = CARTESIAN_POINT ( 'NONE',  ( 3.250256321940253823, -1.871563930198836712, -93.44355375713804790 ) ) ;
#25534 = CARTESIAN_POINT ( 'NONE',  ( -1.158394559368730592, 3.499774879702899799, 227.7538236713963897 ) ) ;
#25535 = CARTESIAN_POINT ( 'NONE',  ( -1.841797396446221979, -26.73663745407121795, 20.00000000000000355 ) ) ;
#25536 = CARTESIAN_POINT ( 'NONE',  ( -2.746723693872569871, -2.614252338060372161, -0.8157167102000040249 ) ) ;
#25537 = CARTESIAN_POINT ( 'NONE',  ( 24.34663841809999951, -12.78636765230000094, 225.0000000000000000 ) ) ;
#25538 = CARTESIAN_POINT ( 'NONE',  ( 16.06675444876397307, -9.020011618195203695, -0.6999999999999784173 ) ) ;
#25539 = CARTESIAN_POINT ( 'NONE',  ( -9.999999999919999993, -25.00000000000000000, -7.274962171499997687 ) ) ;
#25540 = EDGE_LOOP ( 'NONE', ( #21448, #26932, #23638, #18384 ) ) ;
#25541 = CARTESIAN_POINT ( 'NONE',  ( 5.242919931573567283, -2.735361231296036699, -60.83790713612500412 ) ) ;
#25542 = CARTESIAN_POINT ( 'NONE',  ( -18.95046173579999760, -18.95046173579999760, 36.78285841159999592 ) ) ;
#25543 = ORIENTED_EDGE ( 'NONE', *, *, #4274, .F. ) ;
#25544 = AXIS2_PLACEMENT_3D ( 'NONE', #12891, #22498, #13186 ) ;
#25545 = CARTESIAN_POINT ( 'NONE',  ( -1.814319851916122772, 5.833166587536846137, -4.774955258300003891 ) ) ;
#25546 = VERTEX_POINT ( 'NONE', #2251 ) ;
#25547 = DIRECTION ( 'NONE',  ( 0.000000000000000000, 0.000000000000000000, 1.000000000000000000 ) ) ;
#25548 = LINE ( 'NONE', #27734, #8241 ) ;
#25549 = EDGE_LOOP ( 'NONE', ( #28056, #23665, #6928, #1481 ) ) ;
#25550 = ORIENTED_EDGE ( 'NONE', *, *, #14244, .T. ) ;
#25551 = ORIENTED_EDGE ( 'NONE', *, *, #28292, .T. ) ;
#25552 = AXIS2_PLACEMENT_3D ( 'NONE', #9286, #7244, #16837 ) ;
#25553 = CARTESIAN_POINT ( 'NONE',  ( 3.326321151026052636, -1.384230863725755878, -93.72782493932767522 ) ) ;
#25554 = PRESENTATION_STYLE_ASSIGNMENT (( #28371 ) ) ;
#25555 = VERTEX_POINT ( 'NONE', #11840 ) ;
#25556 = CARTESIAN_POINT ( 'NONE',  ( -12.29999999969999891, -27.00000000000000000, -28.40000000020000215 ) ) ;
#25557 = CYLINDRICAL_SURFACE ( 'NONE', #13975, 2.100000000000000977 ) ;
#25558 = CARTESIAN_POINT ( 'NONE',  ( 5.807653394784360934, -2.603268055249425394, -67.27841551502500295 ) ) ;
#25559 = EDGE_CURVE ( 'NONE', #11184, #1865, #2129, .T. ) ;
#25560 = CARTESIAN_POINT ( 'NONE',  ( 26.94142135619999934, -7.057848136739999667, 230.0000000000000000 ) ) ;
#25561 = CARTESIAN_POINT ( 'NONE',  ( -250010.8602219996974, 207571.5434020000394, 379978.1847439997364 ) ) ;
#25562 = CYLINDRICAL_SURFACE ( 'NONE', #22585, 0.9999999999999988898 ) ;
#25563 = CARTESIAN_POINT ( 'NONE',  ( 4.799848611324305736, -2.144583235354477591, -35.69999999999999574 ) ) ;
#25564 = EDGE_LOOP ( 'NONE', ( #5176, #11911, #14208, #14256 ) ) ;
#25565 = EDGE_CURVE ( 'NONE', #28783, #15300, #4911, .T. ) ;
#25566 = CARTESIAN_POINT ( 'NONE',  ( -26.87465790466033155, 0.8603305708294651799, -1.399999999999998579 ) ) ;
#25567 = CIRCLE ( 'NONE', #2454, 2.999999999999999556 ) ;
#25568 = CARTESIAN_POINT ( 'NONE',  ( 2.618538529469180531, 3.470429992801026042, -14.22796858840000311 ) ) ;
#25569 = CARTESIAN_POINT ( 'NONE',  ( 21.30888436558567633, -16.34772642260384856, 136.7828584119999960 ) ) ;
#25570 = FACE_OUTER_BOUND ( 'NONE', #18951, .T. ) ;
#25571 = VERTEX_POINT ( 'NONE', #19546 ) ;
#25572 = CARTESIAN_POINT ( 'NONE',  ( 17.83928249680000278, 19.99999999999999645, -1.399999999299995856 ) ) ;
#25573 = CARTESIAN_POINT ( 'NONE',  ( -22.68367506360150188, -14.27296989836904828, 4.579417935583666832 ) ) ;
#25574 = CARTESIAN_POINT ( 'NONE',  ( 24.32472724076343695, -13.45989056521276872, 3.899998581000013509 ) ) ;
#25575 = CARTESIAN_POINT ( 'NONE',  ( 26.15365760668691308, 9.467937797150383972, 0.08279779700001710374 ) ) ;
#25576 = CARTESIAN_POINT ( 'NONE',  ( 22.78048776663572639, -14.11708351801274297, 4.280684603339811822 ) ) ;
#25577 = CARTESIAN_POINT ( 'NONE',  ( -2.947640775130000104E-14, -27.50000000000000000, 0.000000000000000000 ) ) ;
#25578 = CIRCLE ( 'NONE', #19556, 3.200000000000002398 ) ;
#25579 = CARTESIAN_POINT ( 'NONE',  ( 10.46457122910000059, 21.70000000000000284, -54.63542873130000288 ) ) ;
#25580 = CARTESIAN_POINT ( 'NONE',  ( -13.00000000000000000, 25.22617105830878614, -61.82510970417090590 ) ) ;
#25581 = ORIENTED_EDGE ( 'NONE', *, *, #21634, .F. ) ;
#25582 = EDGE_CURVE ( 'NONE', #30054, #14645, #23965, .T. ) ;
#25583 = FILL_AREA_STYLE ('',( #25264 ) ) ;
#25584 = CARTESIAN_POINT ( 'NONE',  ( -28.50000000000000000, 5.427757009279999762E-15, 222.0000000000000000 ) ) ;
#25585 = EDGE_CURVE ( 'NONE', #16332, #13797, #15595, .T. ) ;
#25586 = B_SPLINE_CURVE_WITH_KNOTS ( 'NONE', 1,
 ( #30940, #24016 ),
 .UNSPECIFIED., .F., .F.,
 ( 2, 2 ),
 ( -0.6999999999459999289, 1.998401444325281773E-15 ),
 .UNSPECIFIED. ) ;
#25587 = CARTESIAN_POINT ( 'NONE',  ( 2.869929429076217620, -3.485336955729469111, -68.10000000002503384 ) ) ;
#25588 = CONICAL_SURFACE ( 'NONE', #29078, 1.303225372841142260, 0.9162978572969998625 ) ;
#25589 = CARTESIAN_POINT ( 'NONE',  ( 26.79556473285982321, 0.4875557887249851730, -0.6999999999999784173 ) ) ;
#25590 = CARTESIAN_POINT ( 'NONE',  ( -24.32472894358752313, 13.45989150749028873, 6.099998581000020792 ) ) ;
#25591 = PRODUCT_RELATED_PRODUCT_CATEGORY ( 'part', '', ( #29916 ) ) ;
#25592 =( NAMED_UNIT ( * ) SI_UNIT ( $, .STERADIAN. ) SOLID_ANGLE_UNIT ( ) );
#25593 = CARTESIAN_POINT ( 'NONE',  ( 14.71164558018262980, -25.85213278945484205, -33.51042165666717665 ) ) ;
#25594 = CARTESIAN_POINT ( 'NONE',  ( 0.6822309889224468238, 4.261764438830168089, -39.55777057273109421 ) ) ;
#25595 = CARTESIAN_POINT ( 'NONE',  ( -1.219854050253892153, 4.750520449216608654, -66.60876360982500444 ) ) ;
#25596 = VERTEX_POINT ( 'NONE', #24421 ) ;
#25597 = DIRECTION ( 'NONE',  ( 0.000000000000000000, -1.000000000000000000, 0.000000000000000000 ) ) ;
#25598 = ORIENTED_EDGE ( 'NONE', *, *, #5167, .F. ) ;
#25601 = EDGE_CURVE ( 'NONE', #12302, #16227, #5211, .T. ) ;
#25600 = CARTESIAN_POINT ( 'NONE',  ( -24.24144457387483698, -14.48500828217274439, 0.000000000000000000 ) ) ;
#25599 = CIRCLE ( 'NONE', #25531, 4.439999999480002124 ) ;
#25602 = VERTEX_POINT ( 'NONE', #26619 ) ;
#25603 = DIRECTION ( 'NONE',  ( -3.924189347185962345E-12, 0.4082287037029530552, 0.9128796883888952163 ) ) ;
#25604 = AXIS2_PLACEMENT_3D ( 'NONE', #23316, #18104, #11354 ) ;
#25605 = CARTESIAN_POINT ( 'NONE',  ( 8.000000000331638716, -14.95611408989132052, -40.37595097046627046 ) ) ;
#25606 = CARTESIAN_POINT ( 'NONE',  ( -10.99999999969999998, 20.99999999999999645, -58.51619611000000276 ) ) ;
#25607 = CARTESIAN_POINT ( 'NONE',  ( -3.455337460955915319, -1.015179960323179920, 230.7778176299147788 ) ) ;
#25608 =( BOUNDED_CURVE ( )  B_SPLINE_CURVE ( 5, ( #10972, #5776, #13480, #13643, #3727, #10819 ),
 .UNSPECIFIED., .F., .F. ) 
 B_SPLINE_CURVE_WITH_KNOTS ( ( 6, 6 ),
 ( 11.42265871740000094, 12.17014935140000098 ),
 .UNSPECIFIED. ) 
 CURVE ( )  GEOMETRIC_REPRESENTATION_ITEM ( )  RATIONAL_B_SPLINE_CURVE ( ( 0.3231753219119999909, 0.3307207062469999514, 0.3388331752689999754, 0.3475394025169999956, 0.3568692924569999980, 0.3668559804790000323 ) ) 
 REPRESENTATION_ITEM ( '' )  );
#25609 = DIRECTION ( 'NONE',  ( 0.9316362575375356503, 0.3633921898465274913, 0.000000000000000000 ) ) ;
#25610 = DIRECTION ( 'NONE',  ( 0.000000000000000000, 0.000000000000000000, 1.000000000000000000 ) ) ;
#25611 = CARTESIAN_POINT ( 'NONE',  ( -4.861312627829579291, -20.50181238075367318, -27.47976714836577017 ) ) ;
#25612 = ORIENTED_EDGE ( 'NONE', *, *, #16742, .F. ) ;
#25613 = CARTESIAN_POINT ( 'NONE',  ( 14.84775334008999970, -29.39779533080000107, -32.78913491209999620 ) ) ;
#25614 = CARTESIAN_POINT ( 'NONE',  ( 27.50000000000000000, -1.776356839399999804E-15, 136.3944487250000179 ) ) ;
#25615 = EDGE_CURVE ( 'NONE', #1750, #28717, #19002, .T. ) ;
#25616 = CARTESIAN_POINT ( 'NONE',  ( -10.69999999989999928, -2.500000000000002220, -2.399999999999999467 ) ) ;
#25617 = DIRECTION ( 'NONE',  ( -6.325958275728752229E-12, -0.3568421334038983650, 0.9341647027306021478 ) ) ;
#25618 = CARTESIAN_POINT ( 'NONE',  ( -24.09883371379999772, -15.21565466309999870, 225.0000014190000002 ) ) ;
#25619 = CARTESIAN_POINT ( 'NONE',  ( 19.80538173169999894, 19.50875421069999760, 226.9999998930000231 ) ) ;
#25620 = EDGE_CURVE ( 'NONE', #7336, #13982, #26468, .T. ) ;
#25621 = CARTESIAN_POINT ( 'NONE',  ( 23.24837000782807905, 15.24326850565740443, 4.713240265032504261 ) ) ;
#25622 = CARTESIAN_POINT ( 'NONE',  ( -17.91168065875913129, 11.26096619578952129, -1.400000000000001910 ) ) ;
#25623 = CARTESIAN_POINT ( 'NONE',  ( 5.477347162681518000, -0.4051096195737657335, -48.32442242802499521 ) ) ;
#25624 = AXIS2_PLACEMENT_3D ( 'NONE', #17073, #29029, #2148 ) ;
#25625 = AXIS2_PLACEMENT_3D ( 'NONE', #28575, #7170, #18811 ) ;
#25626 = EDGE_CURVE ( 'NONE', #19996, #28636, #3609, .T. ) ;
#25627 = CARTESIAN_POINT ( 'NONE',  ( 27.71261514784112379, 0.5042418800004117019, 0.5514269430000329208 ) ) ;
#25628 = CARTESIAN_POINT ( 'NONE',  ( -17.93324555120827668, 10.97998838178171432, -0.6999999999999784173 ) ) ;
#25629 = CARTESIAN_POINT ( 'NONE',  ( 2.484959595460734860, -2.695521301889526544, 230.7405105397797342 ) ) ;
#25630 = PRODUCT_RELATED_PRODUCT_CATEGORY ( 'part', '', ( #6042 ) ) ;
#25631 = CARTESIAN_POINT ( 'NONE',  ( -2.947640775130000104E-14, -27.50000000000000000, 115.0000000000000000 ) ) ;
#25632 = ORIENTED_EDGE ( 'NONE', *, *, #9967, .T. ) ;
#25633 = CLOSED_SHELL ( 'NONE', ( #9372, #21588, #25030, #29167, #12526, #8495, #4150, #14698, #23309, #9196, #6543, #24763, #2132, #17933, #19844, #12830, #7578, #9326, #24074, #5236, #28721, #21159, #9245, #28469 ) ) ;
#25634 = CARTESIAN_POINT ( 'NONE',  ( 5.672553144689285176, -0.9485505809898806540, -35.74517599850000948 ) ) ;
#25635 = ORIENTED_EDGE ( 'NONE', *, *, #10860, .F. ) ;
#25636 = CARTESIAN_POINT ( 'NONE',  ( -5.212126283948660621, -2.851000302232811201, -53.82982952342499061 ) ) ;
#25637 = VERTEX_POINT ( 'NONE', #515 ) ;
#25638 = CONTEXT_DEPENDENT_SHAPE_REPRESENTATION ( #4154, #882 ) ;
#25639 = ORIENTED_EDGE ( 'NONE', *, *, #23865, .F. ) ;
#25640 = EDGE_CURVE ( 'NONE', #18081, #17290, #24637, .T. ) ;
#25641 = VERTEX_POINT ( 'NONE', #7872 ) ;
#25642 = CARTESIAN_POINT ( 'NONE',  ( -8.699999999985950083, -116.8589940772574920, 11.34037319969351643 ) ) ;
#25643 = CARTESIAN_POINT ( 'NONE',  ( 20.30396079652883756, 20.00000000004620304, 1.000000000000000888 ) ) ;
#25644 = DIRECTION ( 'NONE',  ( -1.000000000000000000, 0.000000000000000000, 0.000000000000000000 ) ) ;
#25645 = EDGE_CURVE ( 'NONE', #9489, #10599, #4751, .T. ) ;
#25646 = CARTESIAN_POINT ( 'NONE',  ( 5.548090509119999680, -11.02205857200000061, 232.6627648150000027 ) ) ;
#25647 = DIRECTION ( 'NONE',  ( 0.000000000000000000, 0.000000000000000000, 1.000000000000000000 ) ) ;
#25648 = CARTESIAN_POINT ( 'NONE',  ( -16.70947337985631975, 12.10243747010558657, -4.336808689942017736E-16 ) ) ;
#25649 = CARTESIAN_POINT ( 'NONE',  ( -2.757905763689965095, 3.954155216896602987, -0.6901513540999957286 ) ) ;
#25650 = CARTESIAN_POINT ( 'NONE',  ( -14.09657507470000226, -28.30410041680000077, 229.2404163060000144 ) ) ;
#25651 = CARTESIAN_POINT ( 'NONE',  ( 26.80000000069999899, -3.281945028320000125E-15, 136.7828584130000138 ) ) ;
#25652 = EDGE_CURVE ( 'NONE', #17294, #2824, #15576, .T. ) ;
#25653 = CARTESIAN_POINT ( 'NONE',  ( 4.315341029122434335, -4.279276102762477940, -15.06112212870000455 ) ) ;
#25654 = CARTESIAN_POINT ( 'NONE',  ( -4.976668802704899086, 3.592974922927941073, -34.46696136359999940 ) ) ;
#25655 = CARTESIAN_POINT ( 'NONE',  ( 10.69999999930000101, -127.2537437101000108, -34.36317024011000143 ) ) ;
#25656 = CARTESIAN_POINT ( 'NONE',  ( -7.999999999949311658, -29.44934466747404755, -30.17621036722960426 ) ) ;
#25657 = CARTESIAN_POINT ( 'NONE',  ( -18.15338440918069907, 19.92139857694655802, 0.007026247000024854472 ) ) ;
#25658 = CARTESIAN_POINT ( 'NONE',  ( -23.17877535335809824, -15.80276672810151517, 8.000000000000007105 ) ) ;
#25659 = CARTESIAN_POINT ( 'NONE',  ( -3.188275555100174241, 1.478095767874147759, 227.6463701859477453 ) ) ;
#25660 = CARTESIAN_POINT ( 'NONE',  ( 28.49528339128749366, 0.5184828350247432383, 0.7595836940000044724 ) ) ;
#25661 = AXIS2_PLACEMENT_3D ( 'NONE', #11005, #13514, #27988 ) ;
#25662 = FACE_OUTER_BOUND ( 'NONE', #18182, .T. ) ;
#25663 = CARTESIAN_POINT ( 'NONE',  ( 9.799999999993435296, -14.12326182050966139, -36.34918934884738206 ) ) ;
#25664 = CARTESIAN_POINT ( 'NONE',  ( 0.000000000000000000, -1.776356839399999804E-15, 227.6412452697800006 ) ) ;
#25665 = EDGE_LOOP ( 'NONE', ( #23652, #12525, #1653, #1724 ) ) ;
#25666 = CARTESIAN_POINT ( 'NONE',  ( 27.50000000000000000, -3.367667472999999580E-15, 193.6055512739999926 ) ) ;
#25667 = CARTESIAN_POINT ( 'NONE',  ( 3.911140671018063397, 1.342814479487780543, -38.13410355316680977 ) ) ;
#25668 = CARTESIAN_POINT ( 'NONE',  ( 9.999999999962065900, -38.97546878332597942, -26.38794647299679497 ) ) ;
#25669 = ORIENTED_EDGE ( 'NONE', *, *, #815, .F. ) ;
#25670 = CARTESIAN_POINT ( 'NONE',  ( -9.999999999979998222, -127.2536115484999897, -34.36329565063000047 ) ) ;
#25671 = ORIENTED_EDGE ( 'NONE', *, *, #26012, .T. ) ;
#25672 = ORIENTED_EDGE ( 'NONE', *, *, #3563, .F. ) ;
#25673 = ORIENTED_EDGE ( 'NONE', *, *, #17557, .F. ) ;
#25674 = CARTESIAN_POINT ( 'NONE',  ( 18.97091807949999875, 21.26865672150000108, 229.2404163060000144 ) ) ;
#25675 = EDGE_CURVE ( 'NONE', #24581, #29336, #5520, .T. ) ;
#25676 = ORIENTED_EDGE ( 'NONE', *, *, #16171, .F. ) ;
#25677 = CARTESIAN_POINT ( 'NONE',  ( -24.71725143720000162, -14.18911829940000047, 226.0986578700000109 ) ) ;
#25678 = CARTESIAN_POINT ( 'NONE',  ( 24.36375418468539067, 14.78716628296302282, 3.904032100999987875 ) ) ;
#25679 = DIRECTION ( 'NONE',  ( 1.224606353819999829E-16, 1.000000000000000000, 0.000000000000000000 ) ) ;
#25680 = CYLINDRICAL_SURFACE ( 'NONE', #15953, 27.50000000000000000 ) ;
#25681 = EDGE_CURVE ( 'NONE', #11841, #125, #13063, .T. ) ;
#25682 = CARTESIAN_POINT ( 'NONE',  ( -0.4969045691571343237, -28.49594262166996828, 4.493528488000025689 ) ) ;
#25683 = EDGE_CURVE ( 'NONE', #25887, #27542, #4219, .T. ) ;
#25684 = CARTESIAN_POINT ( 'NONE',  ( 24.10235451439214316, -11.92514887769131526, -1.399999999999998579 ) ) ;
#25685 = CYLINDRICAL_SURFACE ( 'NONE', #22158, 2.299999999999999822 ) ;
#25686 = CARTESIAN_POINT ( 'NONE',  ( -12.00723796003150845, 26.18431201457259050, -59.34801937090718837 ) ) ;
#25687 = ORIENTED_EDGE ( 'NONE', *, *, #26178, .F. ) ;
#25688 = CARTESIAN_POINT ( 'NONE',  ( -2.886686092853935293, -3.810306705960904594, -4.666445369299999868 ) ) ;
#25689 = CARTESIAN_POINT ( 'NONE',  ( -5.902313038799129608, -1.548398769286710053, -25.04656121680000425 ) ) ;
#25690 = PLANE ( 'NONE',  #20889 ) ;
#25691 = CARTESIAN_POINT ( 'NONE',  ( -13.00000000000000000, 23.13259184047820582, -60.45875467758818189 ) ) ;
#25692 = FACE_OUTER_BOUND ( 'NONE', #6609, .T. ) ;
#25693 = DIRECTION ( 'NONE',  ( 2.764840495839172918E-12, 0.9128796883888953273, -0.4082287037029530552 ) ) ;
#25694 = CARTESIAN_POINT ( 'NONE',  ( -12.29999999970000069, -21.59999999962999695, -28.40000000001083791 ) ) ;
#25695 = VECTOR ( 'NONE', #9452, 1000.000000000000000 ) ;
#25696 = CARTESIAN_POINT ( 'NONE',  ( -17.93324555120827668, 10.97998838178171432, -1.000005633855494125E-09 ) ) ;
#25697 = CARTESIAN_POINT ( 'NONE',  ( 1.157672466183025994, -27.77645868488734138, 5.900907654000003610 ) ) ;
#25698 = DIRECTION ( 'NONE',  ( 0.000000000000000000, 0.000000000000000000, 1.000000000000000000 ) ) ;
#25699 = ORIENTED_EDGE ( 'NONE', *, *, #26599, .T. ) ;
#25700 = CARTESIAN_POINT ( 'NONE',  ( -4.361670840543652616, -2.217570095850531775, -61.61424626872500454 ) ) ;
#25701 = DIRECTION ( 'NONE',  ( 0.000000000000000000, 0.4794255386042043932, 0.8775825618903719816 ) ) ;
#25702 = ORIENTED_EDGE ( 'NONE', *, *, #8527, .T. ) ;
#25703 = ORIENTED_EDGE ( 'NONE', *, *, #16999, .F. ) ;
#25704 = CARTESIAN_POINT ( 'NONE',  ( 10.69999999999999929, -27.00000000000000000, -25.39999999999999858 ) ) ;
#25705 = CARTESIAN_POINT ( 'NONE',  ( 0.1051796283266584475, -6.084780997910130829, -33.41110030499999795 ) ) ;
#25706 = ORIENTED_EDGE ( 'NONE', *, *, #17463, .T. ) ;
#25707 = B_SPLINE_CURVE_WITH_KNOTS ( 'NONE', 3,
 ( #29057, #21518, #28905, #21676, #5301, #7501 ),
 .UNSPECIFIED., .F., .F.,
 ( 4, 2, 4 ),
 ( 0.000000000000000000, 0.5000000000000000000, 1.000000000000000000 ),
 .UNSPECIFIED. ) ;
#25708 = CARTESIAN_POINT ( 'NONE',  ( 22.36196472700000015, 17.71394650440000262, 223.9999999570000000 ) ) ;
#25709 = LINE ( 'NONE', #13900, #5740 ) ;
#25710 = EDGE_LOOP ( 'NONE', ( #2141, #15280, #27146, #10618 ) ) ;
#25711 = ADVANCED_FACE ( 'NONE', ( #29594 ), #9218, .F. ) ;
#25712 = ORIENTED_EDGE ( 'NONE', *, *, #17077, .T. ) ;
#25713 = EDGE_CURVE ( 'NONE', #29142, #3795, #14109, .T. ) ;
#25714 = VERTEX_POINT ( 'NONE', #11025 ) ;
#25715 = CARTESIAN_POINT ( 'NONE',  ( -17.79876841389999598, -8.472631907500000281, -0.7000000003999986564 ) ) ;
#25716 = ORIENTED_EDGE ( 'NONE', *, *, #19018, .T. ) ;
#25717 = CARTESIAN_POINT ( 'NONE',  ( 24.70074545475921823, -14.21822122957610368, 6.002806299999996043 ) ) ;
#25718 = CARTESIAN_POINT ( 'NONE',  ( 23.24663841809999809, -14.69162354060000020, 5.000000000000000000 ) ) ;
#25719 = CARTESIAN_POINT ( 'NONE',  ( -1.470080522021702363, 5.724986182348157371, -65.40876360972499981 ) ) ;
#25720 = CARTESIAN_POINT ( 'NONE',  ( 24.76888645009999834, -14.19515663950000040, 229.9751246520000052 ) ) ;
#25721 = CARTESIAN_POINT ( 'NONE',  ( -0.8784916636842051707, -26.78562594404069230, 224.3339239247088699 ) ) ;
#25722 = CARTESIAN_POINT ( 'NONE',  ( 8.000000000361213282, -29.94262568628330357, -29.10368077924198715 ) ) ;
#25723 = CARTESIAN_POINT ( 'NONE',  ( -17.49285076559437613, -24.40406112000763628, -24.12527371869715864 ) ) ;
#25724 = ORIENTED_EDGE ( 'NONE', *, *, #14355, .F. ) ;
#25725 = CARTESIAN_POINT ( 'NONE',  ( -19.46795263067491177, 18.54728466947916132, -1.399999999999998135 ) ) ;
#25726 = CARTESIAN_POINT ( 'NONE',  ( -4.101794773660127902, 5.071170285176791914, -13.00352819870000154 ) ) ;
#25727 = CARTESIAN_POINT ( 'NONE',  ( 9.993285220779439371, -25.61999708228226069, 115.0000000000000000 ) ) ;
#25728 = ORIENTED_EDGE ( 'NONE', *, *, #11241, .T. ) ;
#25729 = CARTESIAN_POINT ( 'NONE',  ( -10.69999999996535323, -29.70138143486801141, -27.04887742378237547 ) ) ;
#25730 = CYLINDRICAL_SURFACE ( 'NONE', #1215, 3.000000000000003997 ) ;
#25731 = CARTESIAN_POINT ( 'NONE',  ( 28.50000000000000000, 7.746889549609999817E-15, 229.0000000000000000 ) ) ;
#25732 = B_SPLINE_CURVE_WITH_KNOTS ( 'NONE', 3,
 ( #23532, #14082, #27929, #30610, #20855, #4168 ),
 .UNSPECIFIED., .F., .F.,
 ( 4, 2, 4 ),
 ( 0.000000000000000000, 0.5000000000000000000, 1.000000000000000000 ),
 .UNSPECIFIED. ) ;
#25733 = CARTESIAN_POINT ( 'NONE',  ( 25.85884820509708604, 9.361201669947201154, 0.000000000000000000 ) ) ;
#25734 = CARTESIAN_POINT ( 'NONE',  ( 11.48163258689999999, -24.28840541759999994, -1.419991652300001128 ) ) ;
#25735 = CARTESIAN_POINT ( 'NONE',  ( -5.325262776966551037, 2.643762325382846612, -56.79877225282499609 ) ) ;
#25736 = CARTESIAN_POINT ( 'NONE',  ( -9.999999999969999109, -24.87872937729999734, -30.52127062079999931 ) ) ;
#25737 = CARTESIAN_POINT ( 'NONE',  ( 10.69999999997582485, -123.0138898083720420, -31.69041458428544544 ) ) ;
#25738 = ORIENTED_EDGE ( 'NONE', *, *, #16254, .T. ) ;
#25739 = EDGE_CURVE ( 'NONE', #13739, #14446, #8645, .T. ) ;
#25740 = DIRECTION ( 'NONE',  ( 1.000000000000000000, 0.000000000000000000, 0.000000000000000000 ) ) ;
#25741 = CARTESIAN_POINT ( 'NONE',  ( -8.699999999985950083, -116.8589940772574920, 11.34037319969351643 ) ) ;
#25742 = CIRCLE ( 'NONE', #24220, 1.100000000390000787 ) ;
#25743 = CARTESIAN_POINT ( 'NONE',  ( 2.865660253176993688, -3.596091862522109661, -68.10000000002500542 ) ) ;
#25744 = PRODUCT_DEFINITION_SHAPE ( 'NONE', 'NONE',  #30228 ) ;
#25745 = EDGE_CURVE ( 'NONE', #12912, #17381, #29834, .T. ) ;
#25746 = CARTESIAN_POINT ( 'NONE',  ( -0.01646793526671820954, -3.529820002194270945, -0.6999999999999783062 ) ) ;
#25747 = CARTESIAN_POINT ( 'NONE',  ( -4.120143249015659315, -0.1148328759544282596, -44.10000000002499121 ) ) ;
#25748 = SURFACE_SIDE_STYLE ('',( #20705 ) ) ;
#25749 = ORIENTED_EDGE ( 'NONE', *, *, #30476, .T. ) ;
#25750 = DIRECTION ( 'NONE',  ( -0.9316362575375349842, 0.3633921898465292122, -0.000000000000000000 ) ) ;
#25751 = CARTESIAN_POINT ( 'NONE',  ( 5.807653394784360934, -2.603268055249425394, -67.75841551502499271 ) ) ;
#25752 = ORIENTED_EDGE ( 'NONE', *, *, #6012, .F. ) ;
#25753 = CARTESIAN_POINT ( 'NONE',  ( -26.58668732968209980, 4.592113237615420118, 0.000000000000000000 ) ) ;
#25754 = CARTESIAN_POINT ( 'NONE',  ( 1.111846212943386591, -3.388043077324369268, -88.52261276293990022 ) ) ;
#25755 = ORIENTED_EDGE ( 'NONE', *, *, #3020, .T. ) ;
#25756 = DIRECTION ( 'NONE',  ( 0.000000000000000000, 0.000000000000000000, 1.000000000000000000 ) ) ;
#25757 = AXIS2_PLACEMENT_3D ( 'NONE', #29622, #19883, #19726 ) ;
#25758 = CARTESIAN_POINT ( 'NONE',  ( 10.99999999979999998, 20.99999999999999645, -67.09999999999999432 ) ) ;
#25759 = CARTESIAN_POINT ( 'NONE',  ( -15.73094807277625584, 10.87373459869253445, -0.6999999999999784173 ) ) ;
#25760 = B_SPLINE_SURFACE_WITH_KNOTS ( 'NONE', 5, 1, ( 
 ( #12236, #16806 ),
 ( #19635, #19484 ),
 ( #2346, #24057 ),
 ( #5004, #2190 ),
 ( #16801, #29071 ),
 ( #28616, #11780 ) ),
 .UNSPECIFIED., .F., .F., .F.,
 ( 6, 6 ),
 ( 2, 2 ),
 ( 4.999999893150000041, 7.000000000150000012 ),
 ( -1.998401444329999950E-15, 0.6999999999459999289 ),
 .UNSPECIFIED. ) ;
#25761 = B_SPLINE_CURVE_WITH_KNOTS ( 'NONE', 3,
 ( #27184, #5469, #22160, #20110, #12703, #15223, #10049, #19645, #29387, #765, #26880, #27339, #7668, #17577, #5321, #14925, #24522, #24829, #10202, #10358, #19949, #12553, #29542, #8124, #3261, #17426 ),
 .UNSPECIFIED., .F., .F.,
 ( 4, 2, 2, 1, 1, 2, 2, 2, 2, 2, 1, 1, 2, 2, 4 ),
 ( 0.000000000000000000, 0.1249999999999994449, 0.1875000000000006661, 0.2187500000000019151, 0.2343750000000026090, 0.2421875000000029698, 0.2500000000000033307, 0.4999999999999833467, 0.6249999999999734657, 0.6874999999999695799, 0.7187499999999664713, 0.7343749999999659162, 0.7421874999999655831, 0.7499999999999653610, 1.000000000000000000 ),
 .UNSPECIFIED. ) ;
#25762 = CARTESIAN_POINT ( 'NONE',  ( -0.1501630637024684578, -28.50011693320769623, 4.099092748999999536 ) ) ;
#25763 = CARTESIAN_POINT ( 'NONE',  ( -12.48073050767821002, -22.00000000000000000, -26.63134324521094598 ) ) ;
#25764 = FACE_OUTER_BOUND ( 'NONE', #16734, .T. ) ;
#25765 = EDGE_CURVE ( 'NONE', #4970, #6914, #27538, .T. ) ;
#25766 = ORIENTED_EDGE ( 'NONE', *, *, #6167, .F. ) ;
#25767 = CARTESIAN_POINT ( 'NONE',  ( -0.6975711794063483850, -3.867593748343274740, -44.10000000002499121 ) ) ;
#25768 = CARTESIAN_POINT ( 'NONE',  ( 24.22190007760000086, -15.01852807150000046, 225.6806946080000102 ) ) ;
#25769 = DIRECTION ( 'NONE',  ( 0.000000000000000000, -1.000000000000000000, 0.000000000000000000 ) ) ;
#25770 = CARTESIAN_POINT ( 'NONE',  ( -2.990544846594861639, -1.820224383388544531, 230.8378734041664586 ) ) ;
#25771 = CARTESIAN_POINT ( 'NONE',  ( -8.000000000457589522, -24.26136093481186862, -29.62468611113247263 ) ) ;
#25772 = CARTESIAN_POINT ( 'NONE',  ( -1.115050571030000048, -28.47845913019999742, 225.2081166120000262 ) ) ;
#25773 = AXIS2_PLACEMENT_3D ( 'NONE', #20087, #1044, #8573 ) ;
#25774 = DIRECTION ( 'NONE',  ( 0.3633921898465292122, 0.9316362575375348731, -6.938893903907226800E-15 ) ) ;
#25775 = CARTESIAN_POINT ( 'NONE',  ( -16.80807069855958247, 9.890905752026485587, -1.400000000000002132 ) ) ;
#25776 = CARTESIAN_POINT ( 'NONE',  ( -4.320323480314920417, -1.509945384023513082, -50.40743646232499486 ) ) ;
#25777 = CARTESIAN_POINT ( 'NONE',  ( -23.48807013383927256, -14.30280389769410831, 5.913085275914951922 ) ) ;
#25778 = CARTESIAN_POINT ( 'NONE',  ( -16.04158851053540857, -9.763538383445707680, -0.6999999989999727834 ) ) ;
#25779 = CARTESIAN_POINT ( 'NONE',  ( 2.114469059363687009, -3.337632158144848482, 230.5777212759258248 ) ) ;
#25780 = AXIS2_PLACEMENT_3D ( 'NONE', #7454, #10286, #29308 ) ;
#25781 = EDGE_CURVE ( 'NONE', #28478, #2098, #970, .T. ) ;
#25782 = DIRECTION ( 'NONE',  ( -1.000000000000000000, -0.000000000000000000, -6.771000000000000128E-12 ) ) ;
#25783 = ORIENTED_EDGE ( 'NONE', *, *, #15941, .T. ) ;
#25784 = DIRECTION ( 'NONE',  ( 1.000000000000000000, -1.953112501701599149E-12, 2.703609717165946368E-12 ) ) ;
#25785 = VERTEX_POINT ( 'NONE', #5673 ) ;
#25786 = CARTESIAN_POINT ( 'NONE',  ( -4.541600168151700423, -0.1148504950298639971, -53.55673954922500002 ) ) ;
#25787 = ORIENTED_EDGE ( 'NONE', *, *, #8678, .F. ) ;
#25788 = PRODUCT_CONTEXT ( 'NONE', #2139, 'mechanical' ) ;
#25789 = EDGE_LOOP ( 'NONE', ( #23590, #27353, #17622, #8489 ) ) ;
#25790 = DIRECTION ( 'NONE',  ( 1.635844237846128888E-12, -0.6889064844488322903, 0.7248502298298253876 ) ) ;
#25791 = ORIENTED_EDGE ( 'NONE', *, *, #3028, .T. ) ;
#25792 = ADVANCED_FACE ( 'NONE', ( #30057 ), #8488, .F. ) ;
#25793 = CARTESIAN_POINT ( 'NONE',  ( 14.55660443456689812, -31.53611277141912694, -25.24542323765480845 ) ) ;
#25794 = DIRECTION ( 'NONE',  ( 3.924189347185962345E-12, -0.4082287037029530552, -0.9128796883888953273 ) ) ;
#25795 = CARTESIAN_POINT ( 'NONE',  ( -17.31926949172702024, -27.96829831963164636, -23.18554460379546711 ) ) ;
#25796 = EDGE_CURVE ( 'NONE', #18566, #18690, #19737, .T. ) ;
#25797 = CIRCLE ( 'NONE', #6688, 2.000000000010000889 ) ;
#25798 = CARTESIAN_POINT ( 'NONE',  ( -5.255844033138538762, 5.146895567855596987, -43.32728369093645426 ) ) ;
#25799 = FACE_OUTER_BOUND ( 'NONE', #8265, .T. ) ;
#25800 = CARTESIAN_POINT ( 'NONE',  ( -16.56504334151864910, 12.07643063650710857, -4.336808689942017243E-16 ) ) ;
#25801 = CARTESIAN_POINT ( 'NONE',  ( -4.274305095845718938, 2.229731738857087642, -0.4812643562999985303 ) ) ;
#25802 = CIRCLE ( 'NONE', #13216, 18.00000000000000000 ) ;
#25803 = CARTESIAN_POINT ( 'NONE',  ( -13.63290864800000080, -27.37311817530000013, 230.5592437530000041 ) ) ;
#25804 = ORIENTED_EDGE ( 'NONE', *, *, #20055, .T. ) ;
#25805 = CARTESIAN_POINT ( 'NONE',  ( 0.000000000000000000, 0.000000000000000000, 115.0000000000000000 ) ) ;
#25806 = EDGE_CURVE ( 'NONE', #13375, #21919, #28316, .T. ) ;
#25807 = CARTESIAN_POINT ( 'NONE',  ( -4.180754675048095947, 1.217138862148074763, -16.30443125759999745 ) ) ;
#25808 = CARTESIAN_POINT ( 'NONE',  ( -6.074876045044606876, 0.8789665559579967757, -34.25783976329999092 ) ) ;
#25809 = CARTESIAN_POINT ( 'NONE',  ( 24.10046253615778511, 13.85738024105139488, 4.039349569685102281 ) ) ;
#25810 = CARTESIAN_POINT ( 'NONE',  ( -19.49296039895628851, 19.58649212980878929, 0.4407160300000101394 ) ) ;
#25811 = CARTESIAN_POINT ( 'NONE',  ( 1.461759203915476313, -27.91510208544341509, 8.000000000000007105 ) ) ;
#25812 = CARTESIAN_POINT ( 'NONE',  ( -8.903108651239966420, -22.82508830966961000, 190.0000000000000000 ) ) ;
#25813 = CARTESIAN_POINT ( 'NONE',  ( 27.03594125075309762, 0.4919295335570642025, -0.6999999999999784173 ) ) ;
#25814 = CARTESIAN_POINT ( 'NONE',  ( -23.28322851814834493, -13.27226524233089933, 3.900000000000000799 ) ) ;
#25815 = CARTESIAN_POINT ( 'NONE',  ( -0.1258946531760308241, -17.01754440315029271, -109.8342699011357126 ) ) ;
#25816 = EDGE_CURVE ( 'NONE', #6569, #2099, #6244, .T. ) ;
#25817 = VECTOR ( 'NONE', #22819, 1000.000000000000000 ) ;
#25818 = CARTESIAN_POINT ( 'NONE',  ( -3.770605797612482490, -1.000149664079264422, -69.24235425649531805 ) ) ;
#25819 = ORIENTED_EDGE ( 'NONE', *, *, #7371, .T. ) ;
#25820 = AXIS2_PLACEMENT_3D ( 'NONE', #7804, #10488, #17698 ) ;
#25821 = CARTESIAN_POINT ( 'NONE',  ( 3.550686847520000117E-05, -28.50022181210000127, 223.9000014189999774 ) ) ;
#25822 = CARTESIAN_POINT ( 'NONE',  ( -10.35000000029999967, -25.00000000000000000, -2.400000000399998612 ) ) ;
#25823 = CARTESIAN_POINT ( 'NONE',  ( 0.9172539291170586084, -5.086450260305231730, -0.6999820721555671810 ) ) ;
#25824 = EDGE_LOOP ( 'NONE', ( #25342, #11022, #26916, #25513 ) ) ;
#25825 = CARTESIAN_POINT ( 'NONE',  ( -1.557622931652909104, -4.259165208650869339, -43.98640794712500224 ) ) ;
#25826 = ORIENTED_EDGE ( 'NONE', *, *, #4741, .F. ) ;
#25827 = EDGE_CURVE ( 'NONE', #23982, #8812, #23461, .T. ) ;
#25828 = EDGE_LOOP ( 'NONE', ( #4062, #22034, #19628, #3202 ) ) ;
#25829 = VERTEX_POINT ( 'NONE', #13533 ) ;
#25830 = CARTESIAN_POINT ( 'NONE',  ( -1.127665019380000189, -28.47796022459999676, 225.0000014190000002 ) ) ;
#25831 = VERTEX_POINT ( 'NONE', #1587 ) ;
#25832 = CARTESIAN_POINT ( 'NONE',  ( -25.22658730140000216, -13.26242337740000110, 225.0000014190000002 ) ) ;
#25833 = CARTESIAN_POINT ( 'NONE',  ( -4.861312627696712241, 5.146895567854025799, -43.32728369093569398 ) ) ;
#25834 = DIRECTION ( 'NONE',  ( 0.000000000000000000, 0.000000000000000000, -1.000000000000000000 ) ) ;
#25835 = CARTESIAN_POINT ( 'NONE',  ( 3.009918263491472512, 2.374761854523940396, -35.69999999999999574 ) ) ;
#25836 = CARTESIAN_POINT ( 'NONE',  ( 17.43495665832235630, -7.923569363432783952, -4.336808689942017243E-16 ) ) ;
#25837 = CARTESIAN_POINT ( 'NONE',  ( 11.69999999989999928, -24.11120071670000087, -1.399999999299995856 ) ) ;
#25838 = CARTESIAN_POINT ( 'NONE',  ( 2.541327885618866134, -2.598290983419757172, 227.7235171295553471 ) ) ;
#25839 = CIRCLE ( 'NONE', #16787, 2.000000000000000000 ) ;
#25840 = CARTESIAN_POINT ( 'NONE',  ( -18.31101975560000028, 19.88193351600000014, 229.9783743860000129 ) ) ;
#25841 = VECTOR ( 'NONE', #2480, 1000.000000000000000 ) ;
#25842 = ORIENTED_EDGE ( 'NONE', *, *, #9216, .T. ) ;
#25843 = CARTESIAN_POINT ( 'NONE',  ( -0.8661127261961210078, -4.701195862525644031, -4.462734013000006605 ) ) ;
#25844 = CARTESIAN_POINT ( 'NONE',  ( -2.496099253731141943, 5.577352528212363048, -22.13780126169999463 ) ) ;
#25845 = LINE ( 'NONE', #4282, #30928 ) ;
#25846 = AXIS2_PLACEMENT_3D ( 'NONE', #18387, #23594, #11618 ) ;
#25847 = CARTESIAN_POINT ( 'NONE',  ( 10.69999999930000101, -27.00000000000000000, -31.39999999999999858 ) ) ;
#25848 = CARTESIAN_POINT ( 'NONE',  ( 2.020725942159999899, 3.500000000000000000, 227.9588918784999976 ) ) ;
#25849 = FACE_OUTER_BOUND ( 'NONE', #17560, .T. ) ;
#25850 = CARTESIAN_POINT ( 'NONE',  ( -24.25909092270000045, -14.95913241679999928, 225.7602679599999931 ) ) ;
#25851 = CARTESIAN_POINT ( 'NONE',  ( 27.24857305730000334, 4.340180672490000177E-12, 229.9172022069999741 ) ) ;
#25852 = CARTESIAN_POINT ( 'NONE',  ( 0.5746121234326042604, -27.79431838510023312, 6.098651075000017130 ) ) ;
#25853 = CARTESIAN_POINT ( 'NONE',  ( -10.00000000016788526, -27.47344925843678709, -16.99201750748492756 ) ) ;
#25854 = ADVANCED_FACE ( 'NONE', ( #4560 ), #30688, .F. ) ;
#25855 = ORIENTED_EDGE ( 'NONE', *, *, #18113, .F. ) ;
#25856 = CARTESIAN_POINT ( 'NONE',  ( -1.143212971672622036, -4.711439499498762729, -61.94311227092499195 ) ) ;
#25857 = CARTESIAN_POINT ( 'NONE',  ( -18.48840241599999956, 20.72770724009999910, 229.2930776200000196 ) ) ;
#25858 = VERTEX_POINT ( 'NONE', #25503 ) ;
#25859 = EDGE_CURVE ( 'NONE', #16515, #18650, #7712, .T. ) ;
#25860 = CARTESIAN_POINT ( 'NONE',  ( 0.7646642646963620615, -28.49022165133369455, 3.920206710000012862 ) ) ;
#25861 = CARTESIAN_POINT ( 'NONE',  ( -5.864216825196034932, 1.669623860970033347, -31.30158078969999380 ) ) ;
#25862 = ORIENTED_EDGE ( 'NONE', *, *, #11896, .T. ) ;
#25863 = EDGE_CURVE ( 'NONE', #26900, #26548, #23321, .T. ) ;
#25864 = CARTESIAN_POINT ( 'NONE',  ( 27.23548387060000309, -1.776356839399999804E-15, 138.3395398250000028 ) ) ;
#25865 = CARTESIAN_POINT ( 'NONE',  ( -3.901237024542355769, -0.9768880954038594577, -68.10000000002501963 ) ) ;
#25866 = AXIS2_PLACEMENT_3D ( 'NONE', #30572, #20966, #11677 ) ;
#25867 = ORIENTED_EDGE ( 'NONE', *, *, #7156, .F. ) ;
#25868 = COLOUR_RGB ( '', 0.40784314, 0.44705882, 0.49803922) ;
#25869 = VERTEX_POINT ( 'NONE', #16203 ) ;
#25870 = VERTEX_POINT ( 'NONE', #3941 ) ;
#25871 = VECTOR ( 'NONE', #25769, 1000.000000000000000 ) ;
#25872 = B_SPLINE_CURVE_WITH_KNOTS ( 'NONE', 1,
 ( #24009, #10453 ),
 .UNSPECIFIED., .F., .F.,
 ( 2, 2 ),
 ( -2.557518061549999935E-06, 0.7000000000009999335 ),
 .UNSPECIFIED. ) ;
#25873 = AXIS2_PLACEMENT_3D ( 'NONE', #25256, #10934, #18323 ) ;
#25874 = ORIENTED_EDGE ( 'NONE', *, *, #16163, .T. ) ;
#25875 = CARTESIAN_POINT ( 'NONE',  ( -8.699999999632044734, -21.59934857482445381, -40.40126712747085236 ) ) ;
#25876 = CARTESIAN_POINT ( 'NONE',  ( 4.117846205589238195, 1.989599136607399954, -66.45315453652499116 ) ) ;
#25877 = CARTESIAN_POINT ( 'NONE',  ( 20.64716981400000151, -20.77933506639999806, 229.1414209110000115 ) ) ;
#25878 = CARTESIAN_POINT ( 'NONE',  ( -18.17095077428239236, 20.37181511265805156, -0.6577119969999878357 ) ) ;
#25879 = CARTESIAN_POINT ( 'NONE',  ( 8.000000000235820252, -29.73863906515999389, -27.17531388883937993 ) ) ;
#25880 = CARTESIAN_POINT ( 'NONE',  ( -23.64677485492346065, -12.61282739001573994, 5.633487048013353871 ) ) ;
#25881 = ORIENTED_EDGE ( 'NONE', *, *, #26593, .T. ) ;
#25882 = CARTESIAN_POINT ( 'NONE',  ( 10.32522729140000095, -24.73114799960000099, -1.399999999999998579 ) ) ;
#25883 = CARTESIAN_POINT ( 'NONE',  ( 3.082386449366550263, -3.056625787687238471, -15.06112212870000455 ) ) ;
#25884 = CARTESIAN_POINT ( 'NONE',  ( -3.552713678799999608E-15, 0.000000000000000000, 93.21714158839999698 ) ) ;
#25885 = VECTOR ( 'NONE', #24339, 1000.000000000000000 ) ;
#25886 = CARTESIAN_POINT ( 'NONE',  ( 11.98357239787091189, 2.900346313630838058, 232.6627636033630324 ) ) ;
#25887 = VERTEX_POINT ( 'NONE', #18716 ) ;
#25888 = CARTESIAN_POINT ( 'NONE',  ( 24.35861421954996331, 11.38494958298328008, -1.399999999999998579 ) ) ;
#25889 = CARTESIAN_POINT ( 'NONE',  ( -10.69999999999999929, -127.2537393281999982, -34.36317439833000265 ) ) ;
#25890 = AXIS2_PLACEMENT_3D ( 'NONE', #4985, #2784, #28598 ) ;
#25891 = CARTESIAN_POINT ( 'NONE',  ( -22.97554860800000043, 15.65134970540000126, 222.0000000000000000 ) ) ;
#25892 = CARTESIAN_POINT ( 'NONE',  ( 0.8959394325450000807, -28.48619164239999790, 225.6801530179999986 ) ) ;
#25893 = DIRECTION ( 'NONE',  ( 0.3633921898465291567, 0.9316362575375349842, 0.000000000000000000 ) ) ;
#25894 = CARTESIAN_POINT ( 'NONE',  ( 3.916181512753878824, -4.480608557854155904, -64.49605006312501132 ) ) ;
#25895 = CARTESIAN_POINT ( 'NONE',  ( 353541.3905939778197, 322735.7599763900507, -144366.1751435059414 ) ) ;
#25896 = CARTESIAN_POINT ( 'NONE',  ( 16.06409288198120677, 11.12626540299224942, -0.6999999999999784173 ) ) ;
#25897 = ORIENTED_EDGE ( 'NONE', *, *, #24992, .F. ) ;
#25898 = CARTESIAN_POINT ( 'NONE',  ( -10.00000000010862955, -28.84364015992474606, -30.79900052719611736 ) ) ;
#25899 = DIRECTION ( 'NONE',  ( -0.7071067811865475727, -0.7071067811865475727, 0.000000000000000000 ) ) ;
#25900 = CARTESIAN_POINT ( 'NONE',  ( 2.814735968722008153, -3.697461604360650522, -68.10000000002499121 ) ) ;
#25901 = EDGE_CURVE ( 'NONE', #20382, #12383, #23870, .T. ) ;
#25902 = TOROIDAL_SURFACE ( 'NONE', #22853, 18.16530045470000232, 1.699999999999999956 ) ;
#25903 = AXIS2_PLACEMENT_3D ( 'NONE', #17597, #788, #8145 ) ;
#25904 = CARTESIAN_POINT ( 'NONE',  ( 17.16657240421717390, -9.000000000001264766, -0.6999999999999784173 ) ) ;
#25905 = CARTESIAN_POINT ( 'NONE',  ( -4.125964278595938950, -0.08019631128595877678, -44.10000000002500542 ) ) ;
#25906 = ORIENTED_EDGE ( 'NONE', *, *, #496, .T. ) ;
#25907 = CARTESIAN_POINT ( 'NONE',  ( 1.906343942476213638, 12.18129127136987400, 232.6627637660202481 ) ) ;
#25908 = CARTESIAN_POINT ( 'NONE',  ( -4.150389416700805079, 1.923785201099232900, -66.17526299432499570 ) ) ;
#25909 = ORIENTED_EDGE ( 'NONE', *, *, #8216, .T. ) ;
#25910 = DIRECTION ( 'NONE',  ( 0.3633921898465272138, -0.9316362575375356503, -9.251858538542967489E-15 ) ) ;
#25911 = CARTESIAN_POINT ( 'NONE',  ( -27.24406355354269849, -0.4957164003159642007, 0.08279779300002232389 ) ) ;
#25912 = VERTEX_POINT ( 'NONE', #21404 ) ;
#25913 = CARTESIAN_POINT ( 'NONE',  ( -3.326860148959999819, -4.874695247160000022, 226.6412452697800006 ) ) ;
#25914 = CARTESIAN_POINT ( 'NONE',  ( -23.23277126416379801, -15.26692729116844482, 4.895813258999987205 ) ) ;
#25915 = DIRECTION ( 'NONE',  ( 2.764802276011834339E-12, 0.9128796883888953273, -0.4082287037029531107 ) ) ;
#25916 = CARTESIAN_POINT ( 'NONE',  ( 7.312007425309010600, -7.897185061697537201, -36.96526048002264986 ) ) ;
#25917 = FACE_OUTER_BOUND ( 'NONE', #1946, .T. ) ;
#25918 = CARTESIAN_POINT ( 'NONE',  ( -0.1113126277255015173, -0.6952657331094624915, -40.47787123679744070 ) ) ;
#25919 = AXIS2_PLACEMENT_3D ( 'NONE', #22643, #12572, #22035 ) ;
#25920 = CARTESIAN_POINT ( 'NONE',  ( -23.81866442513004856, -14.33570206453694240, 6.099998581000020792 ) ) ;
#25921 = EDGE_LOOP ( 'NONE', ( #28742, #5457, #8536, #29949 ) ) ;
#25922 = CARTESIAN_POINT ( 'NONE',  ( 10.69999999996162998, -27.38139074261332695, -25.40000000000000568 ) ) ;
#25923 = EDGE_CURVE ( 'NONE', #17734, #10804, #29476, .T. ) ;
#25924 = CARTESIAN_POINT ( 'NONE',  ( 17.83931934289999788, 20.00000000000000000, 230.7000122960000112 ) ) ;
#25925 = CARTESIAN_POINT ( 'NONE',  ( -27.79999999999999716, -2.355677988119999702E-11, 223.3999999999999773 ) ) ;
#25926 = LINE ( 'NONE', #4665, #27711 ) ;
#25927 = CARTESIAN_POINT ( 'NONE',  ( -0.8057362887179999600, -27.78873281830000153, 225.7596419580000315 ) ) ;
#25928 = CARTESIAN_POINT ( 'NONE',  ( -0.1455402981285491004, -27.49999999999999289, 226.1000000000000227 ) ) ;
#25929 = CARTESIAN_POINT ( 'NONE',  ( -4.499842235593497719, -29.81936866046843093, 0.000000000000000000 ) ) ;
#25930 = CARTESIAN_POINT ( 'NONE',  ( 3.317242526492594212, 4.404831280259204895, -53.82619010302499873 ) ) ;
#25931 = CARTESIAN_POINT ( 'NONE',  ( 19.80538173169999894, 19.50875421069999760, 226.9999998930000231 ) ) ;
#25932 = LINE ( 'NONE', #23110, #14832 ) ;
#25933 = CYLINDRICAL_SURFACE ( 'NONE', #3242, 1.099999999999999867 ) ;
#25934 = DIRECTION ( 'NONE',  ( 0.000000000000000000, 2.256505319260000033E-12, 1.000000000000000000 ) ) ;
#25935 = CARTESIAN_POINT ( 'NONE',  ( 4.198532171036193361, 1.238783022255082189, -36.03159726780002359 ) ) ;
#25936 = ORIENTED_EDGE ( 'NONE', *, *, #21955, .T. ) ;
#25937 = EDGE_CURVE ( 'NONE', #21389, #11492, #19787, .T. ) ;
#25938 = CARTESIAN_POINT ( 'NONE',  ( 2.097865490181839654, -3.779070126327678025, -55.98172062782500547 ) ) ;
#25939 = ORIENTED_EDGE ( 'NONE', *, *, #5968, .T. ) ;
#25940 = CONTEXT_DEPENDENT_SHAPE_REPRESENTATION ( #18006, #6952 ) ;
#25941 = ORIENTED_EDGE ( 'NONE', *, *, #25601, .T. ) ;
#25942 = DIRECTION ( 'NONE',  ( 0.4911057670060950398, -1.966019939440381643E-12, -0.8710999515631688839 ) ) ;
#25943 = B_SPLINE_CURVE_WITH_KNOTS ( 'NONE', 3,
 ( #22124, #19609, #14429, #584, #29189, #14587 ),
 .UNSPECIFIED., .F., .F.,
 ( 4, 2, 4 ),
 ( 0.000000000000000000, 0.5000000000000000000, 1.000000000000000000 ),
 .UNSPECIFIED. ) ;
#25944 = ORIENTED_EDGE ( 'NONE', *, *, #17109, .T. ) ;
#25945 = FACE_OUTER_BOUND ( 'NONE', #7444, .T. ) ;
#25946 = DIRECTION ( 'NONE',  ( 0.000000000000000000, 0.7113488923935522568, -0.7028390664230799167 ) ) ;
#25947 = PLANE ( 'NONE',  #18980 ) ;
#25948 = EDGE_CURVE ( 'NONE', #12574, #5207, #10243, .T. ) ;
#25949 = CARTESIAN_POINT ( 'NONE',  ( -5.260974094009999824, -10.78653348610000151, 231.9999991140000191 ) ) ;
#25950 = FACE_BOUND ( 'NONE', #1334, .T. ) ;
#25951 = FACE_OUTER_BOUND ( 'NONE', #9873, .T. ) ;
#25952 = CARTESIAN_POINT ( 'NONE',  ( 6.086077541567210147, 0.7980478301550381071, -5.026979598399996974 ) ) ;
#25953 = CARTESIAN_POINT ( 'NONE',  ( -23.65604620319999896, -20.91081238350000149, 229.4982322489999831 ) ) ;
#25954 = VERTEX_POINT ( 'NONE', #6913 ) ;
#25955 = CARTESIAN_POINT ( 'NONE',  ( -24.22223838309999877, -15.01863363600000056, 224.3191706570000292 ) ) ;
#25956 = EDGE_CURVE ( 'NONE', #27093, #23530, #22358, .T. ) ;
#25957 = CARTESIAN_POINT ( 'NONE',  ( 5.232234863148874204, 1.547035423556993639, -18.54190840230001314 ) ) ;
#25958 = CARTESIAN_POINT ( 'NONE',  ( -3.554763430470067043, 2.566410659217312151, -33.96696136360001361 ) ) ;
#25959 = B_SPLINE_CURVE_WITH_KNOTS ( 'NONE', 5,
 ( #19112, #4488, #2588, #6839, #26355, #14089, #9349, #21166, #14399, #16588, #11874, #7153 ),
 .UNSPECIFIED., .F., .F.,
 ( 6, 3, 3, 6 ),
 ( 3.339306057409999973, 4.810258470149999965, 6.613963845949999865, 6.678484290009999214 ),
 .UNSPECIFIED. ) ;
#25960 = CARTESIAN_POINT ( 'NONE',  ( 24.26024164798999649, 13.57543367310533000, 4.323353004038539282 ) ) ;
#25961 = CARTESIAN_POINT ( 'NONE',  ( -24.19505510210000310, -13.69211658319999891, 223.9201349309999785 ) ) ;
#25962 = CARTESIAN_POINT ( 'NONE',  ( -28.43007859798022707, -2.264358681363081605, 8.000000000000007105 ) ) ;
#25963 = CARTESIAN_POINT ( 'NONE',  ( 9.993285220779439371, -25.61999708228226069, 136.3944487260000074 ) ) ;
#25964 = CARTESIAN_POINT ( 'NONE',  ( 26.45504170235313879, 9.577025040725851923, -0.5592437529999827461 ) ) ;
#25965 = CARTESIAN_POINT ( 'NONE',  ( 9.738910687886868089, -24.96785170200598358, 86.78285841159998881 ) ) ;
#25966 = CARTESIAN_POINT ( 'NONE',  ( -17.49999999965344344, -27.00000000000000000, -28.40000000020000215 ) ) ;
#25967 = ADVANCED_FACE ( 'NONE', ( #30381 ), #8807, .F. ) ;
#25968 = CARTESIAN_POINT ( 'NONE',  ( 27.54391550559999757, -3.373045393719999713E-15, 187.0437466829999948 ) ) ;
#25969 = ORIENTED_EDGE ( 'NONE', *, *, #28555, .T. ) ;
#25970 = B_SPLINE_CURVE_WITH_KNOTS ( 'NONE', 3,
 ( #14589, #6752, #4243, #11014, #8957, #20762 ),
 .UNSPECIFIED., .F., .F.,
 ( 4, 2, 4 ),
 ( 0.000000000000000000, 0.5000000000000000000, 1.000000000000000000 ),
 .UNSPECIFIED. ) ;
#25971 = CARTESIAN_POINT ( 'NONE',  ( -11.39835558780000113, 19.99999999999999645, -0.7167260558000043691 ) ) ;
#25972 = SURFACE_SIDE_STYLE ('',( #4411 ) ) ;
#25973 =( NAMED_UNIT ( * ) PLANE_ANGLE_UNIT ( ) SI_UNIT ( $, .RADIAN. ) );
#25974 = LINE ( 'NONE', #15902, #27640 ) ;
#25975 = ORIENTED_EDGE ( 'NONE', *, *, #9384, .F. ) ;
#25976 = CARTESIAN_POINT ( 'NONE',  ( -5.162912894389027230, 3.035924517800103750, -44.84354844312500177 ) ) ;
#25977 = ORIENTED_EDGE ( 'NONE', *, *, #31035, .F. ) ;
#25978 = ORIENTED_EDGE ( 'NONE', *, *, #1001, .F. ) ;
#25979 = EDGE_CURVE ( 'NONE', #27585, #4187, #24381, .T. ) ;
#25980 = DIRECTION ( 'NONE',  ( 1.000000000000000000, 0.000000000000000000, 0.000000000000000000 ) ) ;
#25981 = EDGE_LOOP ( 'NONE', ( #10115, #22036, #12201, #14676 ) ) ;
#25982 = CARTESIAN_POINT ( 'NONE',  ( -9.999999999959999997, -29.06671945329999929, -26.22544931050000017 ) ) ;
#25983 = ORIENTED_EDGE ( 'NONE', *, *, #6842, .T. ) ;
#25984 = CARTESIAN_POINT ( 'NONE',  ( -24.80426825129999813, -14.03688870149999879, 226.0798679069999935 ) ) ;
#25985 = CARTESIAN_POINT ( 'NONE',  ( -24.60699806910000120, -12.93667933180000063, 225.0000014190000002 ) ) ;
#25986 = CARTESIAN_POINT ( 'NONE',  ( 3.759125770765979535, 0.1161620079115446708, -35.69999999999999574 ) ) ;
#25987 = CARTESIAN_POINT ( 'NONE',  ( 18.94011831790433931, 20.00034691316145086, -0.5314523398227246620 ) ) ;
#25988 = EDGE_CURVE ( 'NONE', #26221, #2944, #24219, .T. ) ;
#25989 = CARTESIAN_POINT ( 'NONE',  ( 3.843630909669756957, -2.553018000905745044, -0.6999999999999992895 ) ) ;
#25990 = DIRECTION ( 'NONE',  ( 0.000000000000000000, 0.000000000000000000, -1.000000000000000000 ) ) ;
#25991 = CARTESIAN_POINT ( 'NONE',  ( -20.30397143389999925, 20.00000785070000120, 229.1256643320000137 ) ) ;
#25992 = ORIENTED_EDGE ( 'NONE', *, *, #24532, .T. ) ;
#25993 = CARTESIAN_POINT ( 'NONE',  ( 2.246931792404676997, -6.149078805876593279, -6.860585232200004491 ) ) ;
#25994 = CARTESIAN_POINT ( 'NONE',  ( -0.6320852424383932577, 6.069672320066970883, -25.28903409330000684 ) ) ;
#25995 = CARTESIAN_POINT ( 'NONE',  ( 0.000000000000000000, 0.000000000000000000, 115.0000000000000000 ) ) ;
#25996 = FACE_BOUND ( 'NONE', #5072, .T. ) ;
#25997 = CARTESIAN_POINT ( 'NONE',  ( 1.290941959520814475, 3.499733189051936755, 227.7701677845689119 ) ) ;
#25998 = CARTESIAN_POINT ( 'NONE',  ( -3.372638840113360459, -21.47650793462416630, -30.34218218423842472 ) ) ;
#25999 = CARTESIAN_POINT ( 'NONE',  ( -24.02415253779999915, -13.98938335050000070, 226.0959707279999975 ) ) ;
#26000 = ADVANCED_FACE ( 'NONE', ( #2818 ), #29239, .F. ) ;
#26001 = VECTOR ( 'NONE', #10422, 1000.000000000000000 ) ;
#26002 = DIRECTION ( 'NONE',  ( 0.000000000000000000, -0.7113488923935499253, 0.7028390664230821372 ) ) ;
#26003 = DIRECTION ( 'NONE',  ( 1.000000000000000000, 0.000000000000000000, 0.000000000000000000 ) ) ;
#26004 = CARTESIAN_POINT ( 'NONE',  ( 10.00000000070000183, -43.95328087560000085, -27.24755286599999948 ) ) ;
#26005 = ORIENTED_EDGE ( 'NONE', *, *, #10616, .T. ) ;
#26006 = CARTESIAN_POINT ( 'NONE',  ( -0.8249440165340113928, 4.504533947698903695, -60.25324387862499975 ) ) ;
#26007 = CARTESIAN_POINT ( 'NONE',  ( -24.88589369081283920, 13.89120818323882922, 6.095967889000020179 ) ) ;
#26008 = EDGE_LOOP ( 'NONE', ( #2488, #23505, #17561, #8326, #29683 ) ) ;
#26009 = FACE_OUTER_BOUND ( 'NONE', #29278, .T. ) ;
#26010 = CARTESIAN_POINT ( 'NONE',  ( -4.976668802705447092, 3.592974922927108405, -34.46696136359999940 ) ) ;
#26011 = ORIENTED_EDGE ( 'NONE', *, *, #3929, .T. ) ;
#26012 = EDGE_CURVE ( 'NONE', #2408, #18020, #10316, .T. ) ;
#26013 = CARTESIAN_POINT ( 'NONE',  ( -10.99289321870000080, -24.65831413349999934, -1.692893218799999877 ) ) ;
#26014 = CARTESIAN_POINT ( 'NONE',  ( 12.77819780750000156, 21.69999999929999390, -56.09999999999999432 ) ) ;
#26015 = ORIENTED_EDGE ( 'NONE', *, *, #6012, .T. ) ;
#26016 = ORIENTED_EDGE ( 'NONE', *, *, #7747, .T. ) ;
#26017 = EDGE_LOOP ( 'NONE', ( #30179, #24658, #10914, #17027 ) ) ;
#26018 = B_SPLINE_CURVE_WITH_KNOTS ( 'NONE', 3,
 ( #2002, #9369, #11740, #1685 ),
 .UNSPECIFIED., .F., .F.,
 ( 4, 4 ),
 ( -0.1743933577400000046, 0.1743933577400000046 ),
 .UNSPECIFIED. ) ;
#26019 = ORIENTED_EDGE ( 'NONE', *, *, #17309, .T. ) ;
#26020 = DIRECTION ( 'NONE',  ( -1.000000000000000000, 5.063197467949062204E-16, -2.257212216284997029E-12 ) ) ;
#26021 = CIRCLE ( 'NONE', #5892, 2.000000000000000000 ) ;
#26022 = DIRECTION ( 'NONE',  ( 0.000000000000000000, 0.000000000000000000, 1.000000000000000000 ) ) ;
#26023 = CARTESIAN_POINT ( 'NONE',  ( -1.895255389310859684, 5.229048247678121264, -68.67099036452499661 ) ) ;
#26024 = FILL_AREA_STYLE_COLOUR ( '', #23493 ) ;
#26025 = VECTOR ( 'NONE', #12390, 1000.000000000000000 ) ;
#26026 = VECTOR ( 'NONE', #30626, 1000.000000000000000 ) ;
#26027 = CARTESIAN_POINT ( 'NONE',  ( 6.999999999949548801, -115.5267901941268178, 21.04701626962702576 ) ) ;
#26028 = EDGE_CURVE ( 'NONE', #10036, #25445, #27818, .T. ) ;
#26029 = CARTESIAN_POINT ( 'NONE',  ( 8.673459918069999830, -27.31266770540000266, 222.0000000000000000 ) ) ;
#26030 = CARTESIAN_POINT ( 'NONE',  ( 3.170293664407711098, -3.797356553874626783, -0.6999183984185574081 ) ) ;
#26031 = VERTEX_POINT ( 'NONE', #28631 ) ;
#26032 = CARTESIAN_POINT ( 'NONE',  ( 10.58956533789999988, -24.61949705740000027, -1.102843518299999381 ) ) ;
#26033 = EDGE_CURVE ( 'NONE', #1709, #8147, #22170, .T. ) ;
#26034 = CARTESIAN_POINT ( 'NONE',  ( 2.880392382415891017, 3.817472992077249661, -13.29046858840000311 ) ) ;
#26035 = CARTESIAN_POINT ( 'NONE',  ( 0.000000000000000000, 5.495185456771864096, -69.00660115587162124 ) ) ;
#26036 = CARTESIAN_POINT ( 'NONE',  ( -10.69999999969999926, -30.19999999925000012, -28.40000000000000213 ) ) ;
#26037 = EDGE_LOOP ( 'NONE', ( #10225, #20456, #29382, #16384, #10313, #23353 ) ) ;
#26038 = CARTESIAN_POINT ( 'NONE',  ( 1.638687372170417822, -21.81692582114680334, -30.17614928725064161 ) ) ;
#26039 = CARTESIAN_POINT ( 'NONE',  ( 1.186786632755666426, -28.47586096821117252, 4.099089508000003157 ) ) ;
#26040 = CARTESIAN_POINT ( 'NONE',  ( -23.81866442513186755, -14.33570206443695838, 3.899998581000013509 ) ) ;
#26041 = CONICAL_SURFACE ( 'NONE', #20499, 0.9999999999991012745, 0.7853981633970000820 ) ;
#26042 = CARTESIAN_POINT ( 'NONE',  ( 1.099998580829999906, -27.77839262550000043, 225.0000014190000002 ) ) ;
#26043 = ORIENTED_EDGE ( 'NONE', *, *, #26364, .F. ) ;
#26044 = CARTESIAN_POINT ( 'NONE',  ( -11.69999999989999928, -25.00000000000000000, -0.6999999999999992895 ) ) ;
#26045 = CARTESIAN_POINT ( 'NONE',  ( 1.094823181362614140, 5.872682718251108547, -63.42744533522500205 ) ) ;
#26046 = CARTESIAN_POINT ( 'NONE',  ( -10.60826873049999897, -25.00000000000000000, -1.605882353199999946 ) ) ;
#26047 = FACE_BOUND ( 'NONE', #21032, .T. ) ;
#26048 = ORIENTED_EDGE ( 'NONE', *, *, #19651, .F. ) ;
#26049 = CARTESIAN_POINT ( 'NONE',  ( -12.58977862431605388, -22.49200673191992550, -25.22918843513278375 ) ) ;
#26050 = CARTESIAN_POINT ( 'NONE',  ( 17.16657240420000008, 10.97998838177520931, -1.452769935612311825 ) ) ;
#26051 = AXIS2_PLACEMENT_3D ( 'NONE', #3837, #13423, #16253 ) ;
#26052 = CARTESIAN_POINT ( 'NONE',  ( 1.576770949147058731, -4.662922928932242250, -68.10000000002500542 ) ) ;
#26053 = CARTESIAN_POINT ( 'NONE',  ( 9.999999999948014917, -29.62149368169943742, -20.12419128126556700 ) ) ;
#26054 = DIRECTION ( 'NONE',  ( 1.000000000000000000, 0.000000000000000000, -2.257436476311583018E-12 ) ) ;
#26055 = CARTESIAN_POINT ( 'NONE',  ( 14.84775334008999970, -24.60220466919999893, -24.01086508770000094 ) ) ;
#26056 = VERTEX_POINT ( 'NONE', #7679 ) ;
#26057 = PLANE ( 'NONE',  #23012 ) ;
#26058 = CARTESIAN_POINT ( 'NONE',  ( 1.379247882464924579, -27.76613141686495823, 4.319830470999985295 ) ) ;
#26059 = ORIENTED_EDGE ( 'NONE', *, *, #18618, .F. ) ;
#26060 = DIRECTION ( 'NONE',  ( 0.4999999999969509945, -0.4151946956549595336, -0.7600087925169251024 ) ) ;
#26061 = VECTOR ( 'NONE', #16144, 1000.000000000000000 ) ;
#26062 = CARTESIAN_POINT ( 'NONE',  ( -27.58051882800086574, -7.764119750527245678, 0.5514269430000329208 ) ) ;
#26063 = EDGE_CURVE ( 'NONE', #4374, #26433, #21873, .T. ) ;
#26064 = ORIENTED_EDGE ( 'NONE', *, *, #9901, .F. ) ;
#26065 = FACE_OUTER_BOUND ( 'NONE', #30848, .T. ) ;
#26066 = TOROIDAL_SURFACE ( 'NONE', #12484, 24.50000000000000000, 3.200000000000000178 ) ;
#26067 = SURFACE_SIDE_STYLE ('',( #18970 ) ) ;
#26068 = CARTESIAN_POINT ( 'NONE',  ( 17.14656078602323319, -7.900182044548062166, -0.6999999989999727834 ) ) ;
#26069 = CARTESIAN_POINT ( 'NONE',  ( 11.20000000009999930, -27.00000000000000000, -34.17350269180000311 ) ) ;
#26070 = EDGE_CURVE ( 'NONE', #20395, #27980, #11819, .T. ) ;
#26071 = VECTOR ( 'NONE', #27440, 1000.000000000000114 ) ;
#26072 = CARTESIAN_POINT ( 'NONE',  ( 26.80000000069999899, -3.281945028320000125E-15, 42.88981852279999885 ) ) ;
#26073 = EDGE_CURVE ( 'NONE', #17864, #24435, #10060, .T. ) ;
#26074 = PLANE ( 'NONE',  #21073 ) ;
#26075 = EDGE_LOOP ( 'NONE', ( #20169, #2482, #11425, #17293 ) ) ;
#26076 = DIRECTION ( 'NONE',  ( -1.224606353819999829E-16, -1.000000000000000000, 0.000000000000000000 ) ) ;
#26077 = CARTESIAN_POINT ( 'NONE',  ( 24.25874038310000103, -14.95904359230000047, 225.7601370010000039 ) ) ;
#26078 = CARTESIAN_POINT ( 'NONE',  ( 19.68705805829999989, 19.53816415229999848, 229.3697640839999963 ) ) ;
#26079 = CARTESIAN_POINT ( 'NONE',  ( -27.79999999990000248, 4.328052761030000362, 226.2000000000000171 ) ) ;
#26080 = CARTESIAN_POINT ( 'NONE',  ( 8.999999999540001738, 19.99999999999999645, -43.75000000008299850 ) ) ;
#26081 = CARTESIAN_POINT ( 'NONE',  ( -0.2462327729630000017, -28.49941772390000239, 226.0797932899999978 ) ) ;
#26082 = CARTESIAN_POINT ( 'NONE',  ( -24.70448872506469229, 12.74983733322420321, 4.239730451999990102 ) ) ;
#26083 = LINE ( 'NONE', #18988, #71 ) ;
#26084 = CARTESIAN_POINT ( 'NONE',  ( 2.743362564037614248, -4.941860934411918649, -55.58172062782499268 ) ) ;
#26085 = AXIS2_PLACEMENT_3D ( 'NONE', #915, #15374, #24971 ) ;
#26086 = CARTESIAN_POINT ( 'NONE',  ( -7.999999999725509348, -29.60008687027021423, -26.86548392513261518 ) ) ;
#26087 = CARTESIAN_POINT ( 'NONE',  ( 17.43374459427612067, -7.923010675184074536, -0.6999999999999784173 ) ) ;
#26088 = CARTESIAN_POINT ( 'NONE',  ( 3.853987913886425698, -0.3246971213886250540, 230.6318310357701193 ) ) ;
#26089 = ADVANCED_BREP_SHAPE_REPRESENTATION ( '', ( #20809, #17722 ), #23366 ) ;
#26090 = EDGE_LOOP ( 'NONE', ( #6613, #12006, #17025, #16672 ) ) ;
#26091 = CARTESIAN_POINT ( 'NONE',  ( -23.81569860410000317, -13.75000000000000000, 223.8999999999999773 ) ) ;
#26092 = CARTESIAN_POINT ( 'NONE',  ( -24.22223838309999877, -15.01863363600000056, 224.3191706570000292 ) ) ;
#26093 = AXIS2_PLACEMENT_3D ( 'NONE', #23833, #2278, #11863 ) ;
#26094 = CARTESIAN_POINT ( 'NONE',  ( 2.528196872781957705, -4.554263998399506796, -56.38172062782499694 ) ) ;
#26095 = ORIENTED_EDGE ( 'NONE', *, *, #26028, .F. ) ;
#26096 = ADVANCED_FACE ( 'NONE', ( #2513 ), #26729, .T. ) ;
#26097 = ORIENTED_EDGE ( 'NONE', *, *, #18727, .F. ) ;
#26098 = CARTESIAN_POINT ( 'NONE',  ( -17.40850972538804697, -30.55410961813850790, -32.12153152511883292 ) ) ;
#26099 = ORIENTED_EDGE ( 'NONE', *, *, #24207, .F. ) ;
#26100 = CARTESIAN_POINT ( 'NONE',  ( 14.76126683900035985, -30.57407346967977446, -24.69027144666924301 ) ) ;
#26101 = DIRECTION ( 'NONE',  ( 0.000000000000000000, 0.000000000000000000, 1.000000000000000000 ) ) ;
#26102 = CARTESIAN_POINT ( 'NONE',  ( -25.38146355610767912, 12.59839636679889807, 3.799999999999998046 ) ) ;
#26103 = VERTEX_POINT ( 'NONE', #12564 ) ;
#26104 = CARTESIAN_POINT ( 'NONE',  ( -3.934873304249999482, -11.62798211380000168, 232.6627648150000027 ) ) ;
#26105 = CARTESIAN_POINT ( 'NONE',  ( -27.79539923781770128, -0.5057481688779147389, 8.000000000000007105 ) ) ;
#26106 = CARTESIAN_POINT ( 'NONE',  ( 8.700000000279958456, -18.28438020625039329, -36.42481760783426381 ) ) ;
#26107 = CARTESIAN_POINT ( 'NONE',  ( -2.150134890876696847, -3.785840986416655340, -6.185065142700006291 ) ) ;
#26108 = CARTESIAN_POINT ( 'NONE',  ( 20.27449537109999866, -20.40427436439999909, 230.6577119970000069 ) ) ;
#26109 = ORIENTED_EDGE ( 'NONE', *, *, #5724, .T. ) ;
#26110 = CARTESIAN_POINT ( 'NONE',  ( -24.48873108240000107, -14.58042505439999914, 223.9574921880000034 ) ) ;
#26111 = CARTESIAN_POINT ( 'NONE',  ( -4.180754675048084401, 1.217138862148065659, -16.80443125760001521 ) ) ;
#26112 = CARTESIAN_POINT ( 'NONE',  ( 25.43650006538670638, 11.58982781969230125, 8.000000000000007105 ) ) ;
#26113 = AXIS2_PLACEMENT_3D ( 'NONE', #9964, #26639, #29298 ) ;
#26114 = DIRECTION ( 'NONE',  ( 0.000000000000000000, 0.3420201433259318358, -0.9396926207858125046 ) ) ;
#26115 = CARTESIAN_POINT ( 'NONE',  ( 24.35342033856957045, 13.40728427522152444, 4.712140172059656962 ) ) ;
#26116 = CARTESIAN_POINT ( 'NONE',  ( -17.83930458849792089, 19.99999999999597478, -1.000005633855494125E-09 ) ) ;
#26117 = CARTESIAN_POINT ( 'NONE',  ( -15.73547908372051296, -8.877245731167342058, 0.000000000000000000 ) ) ;
#26118 = CARTESIAN_POINT ( 'NONE',  ( -19.49296039895628851, 19.58649212980878929, 0.4407160300000101394 ) ) ;
#26119 = B_SPLINE_CURVE_WITH_KNOTS ( 'NONE', 3,
 ( #2735, #29006, #7752, #17355, #14858, #7452, #24287, #10129, #24449, #26347 ),
 .UNSPECIFIED., .F., .F.,
 ( 4, 2, 2, 2, 4 ),
 ( 0.000000000000000000, 0.2500000000000000000, 0.5000000000000000000, 0.7500000000000000000, 1.000000000000000000 ),
 .UNSPECIFIED. ) ;
#26120 = DIRECTION ( 'NONE',  ( 0.000000000000000000, 1.000000000000000000, 0.000000000000000000 ) ) ;
#26121 = CARTESIAN_POINT ( 'NONE',  ( 17.16657240420000008, 11.00000000000000355, -0.8000000000000020428 ) ) ;
#26122 = CARTESIAN_POINT ( 'NONE',  ( -8.000000000002907896, -107.4273096626132116, 14.66297538107212262 ) ) ;
#26123 = EDGE_CURVE ( 'NONE', #28953, #5952, #210, .T. ) ;
#26124 = ADVANCED_FACE ( 'NONE', ( #24075 ), #19656, .F. ) ;
#26125 = CARTESIAN_POINT ( 'NONE',  ( 24.49999999589999788, -3.000285566359999846E-15, 40.00000000000000000 ) ) ;
#26126 = ORIENTED_EDGE ( 'NONE', *, *, #14101, .T. ) ;
#26127 = CARTESIAN_POINT ( 'NONE',  ( 0.000000000000000000, -1.776356839399999804E-15, 227.6412452697800006 ) ) ;
#26128 = DIRECTION ( 'NONE',  ( 0.3090169943750400994, -0.9510565162951234441, 0.000000000000000000 ) ) ;
#26129 = VERTEX_POINT ( 'NONE', #26891 ) ;
#26130 = CARTESIAN_POINT ( 'NONE',  ( -2.884696998040799709, 4.705809124755043982, -45.85531229042501167 ) ) ;
#26131 = ORIENTED_EDGE ( 'NONE', *, *, #23494, .T. ) ;
#26132 = EDGE_CURVE ( 'NONE', #16714, #13996, #14935, .T. ) ;
#26133 = VERTEX_POINT ( 'NONE', #19032 ) ;
#26134 = B_SPLINE_CURVE_WITH_KNOTS ( 'NONE', 1,
 ( #9093, #25643 ),
 .UNSPECIFIED., .F., .F.,
 ( 2, 2 ),
 ( -0.7000000000189999794, 2.331468351712828735E-15 ),
 .UNSPECIFIED. ) ;
#26135 = CIRCLE ( 'NONE', #20086, 3.200000004570001888 ) ;
#26136 = ORIENTED_EDGE ( 'NONE', *, *, #26242, .F. ) ;
#26137 = CARTESIAN_POINT ( 'NONE',  ( 7.312007425309012376, -6.582071621330287670, -34.26887834112514497 ) ) ;
#26138 = VERTEX_POINT ( 'NONE', #7381 ) ;
#26139 = DIRECTION ( 'NONE',  ( 1.000000000000000000, -1.224606353819999582E-16, 0.000000000000000000 ) ) ;
#26140 = CARTESIAN_POINT ( 'NONE',  ( 23.76534794177020871, 14.42397062701149935, 3.904032100999987875 ) ) ;
#26141 = DIRECTION ( 'NONE',  ( -1.000000000000000000, 0.000000000000000000, 0.000000000000000000 ) ) ;
#26142 = CARTESIAN_POINT ( 'NONE',  ( 0.2315610464403904389, 4.417977769816408440, -35.69999999999999574 ) ) ;
#26143 = CARTESIAN_POINT ( 'NONE',  ( 18.31933453193921579, 19.99999486414201755, -0.6702687248541838727 ) ) ;
#26144 = CARTESIAN_POINT ( 'NONE',  ( 14.58373518890417486, -21.99999999999999645, -26.18669965537439026 ) ) ;
#26145 = CARTESIAN_POINT ( 'NONE',  ( -23.13573312441312879, -13.52773475816182369, 6.100000000000007638 ) ) ;
#26146 = CARTESIAN_POINT ( 'NONE',  ( -20.28767293760000001, 20.00000794000000326, 229.2539848859999836 ) ) ;
#26147 = EDGE_CURVE ( 'NONE', #28386, #8364, #14442, .T. ) ;
#26148 = CARTESIAN_POINT ( 'NONE',  ( -3.010188847181571870, -5.300177381000955812, -7.285065142700005048 ) ) ;
#26149 = CARTESIAN_POINT ( 'NONE',  ( 2.450607853129164848, -3.579122932049590755, -27.13292313650000764 ) ) ;
#26150 = LINE ( 'NONE', #28798, #3783 ) ;
#26151 = DIRECTION ( 'NONE',  ( -0.000000000000000000, 0.000000000000000000, -1.000000000000000000 ) ) ;
#26152 = CARTESIAN_POINT ( 'NONE',  ( 24.98081130624543889, 13.71897605842228529, 5.104178997000024864 ) ) ;
#26153 = CARTESIAN_POINT ( 'NONE',  ( -5.437537900614403780E-11, -115.1185614904174059, 21.95989595798294758 ) ) ;
#26154 = CARTESIAN_POINT ( 'NONE',  ( 2.949882002856674124, 3.605460750137338799, -20.25622222230000347 ) ) ;
#26155 = CARTESIAN_POINT ( 'NONE',  ( 17.96875050214646308, 10.23368197051383532, -1.400000000000001910 ) ) ;
#26156 = CARTESIAN_POINT ( 'NONE',  ( 0.6090474298383116158, -27.79358669172298946, 6.095948809000023338 ) ) ;
#26157 = DIRECTION ( 'NONE',  ( 0.3633921898465291567, 0.9316362575375349842, 0.000000000000000000 ) ) ;
#26158 = VERTEX_POINT ( 'NONE', #15390 ) ;
#26159 = CIRCLE ( 'NONE', #28668, 27.92857142860000152 ) ;
#26160 = ORIENTED_EDGE ( 'NONE', *, *, #23887, .T. ) ;
#26161 = CARTESIAN_POINT ( 'NONE',  ( 9.499999999607904755, -15.94902145823426665, -35.53273252495232271 ) ) ;
#26162 = CARTESIAN_POINT ( 'NONE',  ( -2.705882613314523955, 5.963358562559473164, -31.72635571290000200 ) ) ;
#26163 = EDGE_LOOP ( 'NONE', ( #21138, #15624, #18053, #29959, #942 ) ) ;
#26164 = CARTESIAN_POINT ( 'NONE',  ( 23.53263993737497017, -14.22965940669009655, 5.959546603885336857 ) ) ;
#26165 = CARTESIAN_POINT ( 'NONE',  ( 23.98258507289250474, 15.39789216307533160, 4.239862992999999136 ) ) ;
#26166 = ORIENTED_EDGE ( 'NONE', *, *, #15143, .T. ) ;
#26167 = EDGE_LOOP ( 'NONE', ( #8367, #26473, #30108, #20124 ) ) ;
#26168 = EDGE_CURVE ( 'NONE', #20235, #25231, #28702, .T. ) ;
#26169 = ORIENTED_EDGE ( 'NONE', *, *, #10425, .F. ) ;
#26170 = ORIENTED_EDGE ( 'NONE', *, *, #7234, .F. ) ;
#26171 = DIRECTION ( 'NONE',  ( 1.000000000000000000, -1.843431230206220100E-12, 2.650498504954374861E-12 ) ) ;
#26172 = CARTESIAN_POINT ( 'NONE',  ( -11.49999999969999998, -27.00000000000000000, -28.40000000000541647 ) ) ;
#26173 = CARTESIAN_POINT ( 'NONE',  ( 0.3196029497759475535, 5.089975830446680227, -69.35875473022500159 ) ) ;
#26174 = VERTEX_POINT ( 'NONE', #22327 ) ;
#26175 = CARTESIAN_POINT ( 'NONE',  ( 27.71720220739999974, 1.975664076780000201E-11, 229.4485730569999760 ) ) ;
#26176 = CARTESIAN_POINT ( 'NONE',  ( 24.60666973299078109, -12.93650480179403139, 225.0734590689982610 ) ) ;
#26177 = CARTESIAN_POINT ( 'NONE',  ( 27.70209893939999901, -2.554094161149999653, 222.0000000000000000 ) ) ;
#26178 = EDGE_CURVE ( 'NONE', #1244, #10748, #3423, .T. ) ;
#26179 = CARTESIAN_POINT ( 'NONE',  ( 3.226399722048018948, -3.735024872883826674, -0.6998763472199169833 ) ) ;
#26180 = ORIENTED_EDGE ( 'NONE', *, *, #12872, .T. ) ;
#26181 = CARTESIAN_POINT ( 'NONE',  ( 10.40384844070000092, -24.69832375569999883, -1.291913789700005477 ) ) ;
#26182 = EDGE_CURVE ( 'NONE', #24853, #18124, #23083, .T. ) ;
#26183 = AXIS2_PLACEMENT_3D ( 'NONE', #1546, #16161, #18200 ) ;
#26184 = CARTESIAN_POINT ( 'NONE',  ( -4.363437395929419260, 0.1294788321584625090, -13.18304957890000573 ) ) ;
#26185 = CARTESIAN_POINT ( 'NONE',  ( -13.75032424529999986, -27.60893268180000248, 229.0000000050000040 ) ) ;
#26186 = EDGE_CURVE ( 'NONE', #553, #1959, #20859, .T. ) ;
#26187 = CARTESIAN_POINT ( 'NONE',  ( 1.100000000000000089, -27.47799119230000287, 5.000000000000000000 ) ) ;
#26188 = VERTEX_POINT ( 'NONE', #13174 ) ;
#26189 = LINE ( 'NONE', #13758, #18707 ) ;
#26190 = CARTESIAN_POINT ( 'NONE',  ( -24.09883371379999772, -15.21565466309999870, 225.0000014190000002 ) ) ;
#26191 = CARTESIAN_POINT ( 'NONE',  ( -24.50617912300000256, 13.34342669039999940, 222.0000000000000000 ) ) ;
#26192 = EDGE_CURVE ( 'NONE', #18763, #30472, #20446, .T. ) ;
#26193 = CARTESIAN_POINT ( 'NONE',  ( -10.82908725742657374, -27.76276047461854546, 143.2171415880000040 ) ) ;
#26194 = CARTESIAN_POINT ( 'NONE',  ( -5.941465883516308999, 0.03012783874251079297, -62.57122063482501062 ) ) ;
#26195 = CARTESIAN_POINT ( 'NONE',  ( -10.00000000024713209, -25.48914305888663634, -31.02135916506400193 ) ) ;
#26196 = CARTESIAN_POINT ( 'NONE',  ( 10.69999999997988382, -126.3403250530292183, -33.48783155437846659 ) ) ;
#26197 = ORIENTED_EDGE ( 'NONE', *, *, #5058, .F. ) ;
#26198 = DIRECTION ( 'NONE',  ( -1.000000000000000000, 0.000000000000000000, 0.000000000000000000 ) ) ;
#26199 = CARTESIAN_POINT ( 'NONE',  ( -7.999999999666060901, -18.44015901058016738, -35.17782714789814946 ) ) ;
#26200 = B_SPLINE_CURVE_WITH_KNOTS ( 'NONE', 3,
 ( #12190, #26670, #9997, #29028, #21802, #14720 ),
 .UNSPECIFIED., .F., .F.,
 ( 4, 2, 4 ),
 ( 0.000000000000000000, 0.5000000000000000000, 1.000000000000000000 ),
 .UNSPECIFIED. ) ;
#26201 = CARTESIAN_POINT ( 'NONE',  ( -10.46446609379999870, 21.70000000000000284, -54.63553390589999736 ) ) ;
#26202 = EDGE_CURVE ( 'NONE', #14673, #5141, #17816, .T. ) ;
#26203 = CARTESIAN_POINT ( 'NONE',  ( 9.999999999949999108, -30.49251257979999963, -21.04205368479999905 ) ) ;
#26204 = CYLINDRICAL_SURFACE ( 'NONE', #14759, 1.700000000000000178 ) ;
#26205 = CARTESIAN_POINT ( 'NONE',  ( -6.000000000000000000, -16.80434454291883029, -74.99461076894029077 ) ) ;
#26206 = MECHANICAL_DESIGN_GEOMETRIC_PRESENTATION_REPRESENTATION (  '', ( #30719 ), #9095 ) ;
#26207 = ORIENTED_EDGE ( 'NONE', *, *, #15135, .F. ) ;
#26208 = CARTESIAN_POINT ( 'NONE',  ( -12.18129127137019907, 1.906343942474053366, 232.6627637660202197 ) ) ;
#26209 = CARTESIAN_POINT ( 'NONE',  ( 4.441146713720570460, -1.990734395216660069, -67.67841551502500863 ) ) ;
#26210 = VERTEX_POINT ( 'NONE', #29709 ) ;
#26211 = EDGE_CURVE ( 'NONE', #12999, #23914, #18046, .T. ) ;
#26212 = CARTESIAN_POINT ( 'NONE',  ( -26.79556473285982321, -0.4875557887250224209, 0.000000000000000000 ) ) ;
#26213 = CARTESIAN_POINT ( 'NONE',  ( -1.219854050253890598, 4.750520449216602437, -66.20876360982499875 ) ) ;
#26214 = ORIENTED_EDGE ( 'NONE', *, *, #11762, .T. ) ;
#26215 = LINE ( 'NONE', #4819, #24092 ) ;
#26216 = CARTESIAN_POINT ( 'NONE',  ( -24.36375418918093061, -14.78716628874576244, 3.904032100999987875 ) ) ;
#26217 = CARTESIAN_POINT ( 'NONE',  ( 24.25874038310000103, -14.95904359230000047, 224.2398658380000143 ) ) ;
#26218 = CARTESIAN_POINT ( 'NONE',  ( 8.700000000286459922, -13.45891141627732779, -35.92950628563520610 ) ) ;
#26219 = DIRECTION ( 'NONE',  ( 0.6343890248118320141, 0.7730139489027949562, 0.000000000000000000 ) ) ;
#26220 = DIRECTION ( 'NONE',  ( -2.764840495839172918E-12, -0.9128796883888953273, 0.4082287037029531107 ) ) ;
#26221 = VERTEX_POINT ( 'NONE', #25306 ) ;
#26222 = DIRECTION ( 'NONE',  ( 2.764840495839172918E-12, 0.9128796883888953273, -0.4082287037029530552 ) ) ;
#26223 = CARTESIAN_POINT ( 'NONE',  ( 24.11883219139999923, -15.18335225210000061, 225.3105549429999996 ) ) ;
#26224 = CARTESIAN_POINT ( 'NONE',  ( 20.28774895549999968, 20.00000871369999800, 229.2541281029999993 ) ) ;
#26225 = CARTESIAN_POINT ( 'NONE',  ( -15.73293181562159404, -9.017240966205054775, 0.000000000000000000 ) ) ;
#26226 = VECTOR ( 'NONE', #7182, 1000.000000000000000 ) ;
#26227 = CARTESIAN_POINT ( 'NONE',  ( 8.700000000229927366, -28.07050130669910715, -25.59757157921452020 ) ) ;
#26228 = CARTESIAN_POINT ( 'NONE',  ( -1.419173379759999885E-06, -27.80022181310000207, 226.1000014189999945 ) ) ;
#26229 = CARTESIAN_POINT ( 'NONE',  ( 8.999999999770000869, 20.70710678120000381, -44.39289321881399530 ) ) ;
#26230 = VECTOR ( 'NONE', #19004, 1000.000000000000000 ) ;
#26231 = CYLINDRICAL_SURFACE ( 'NONE', #14779, 2.500000000000001776 ) ;
#26232 = AXIS2_PLACEMENT_3D ( 'NONE', #3674, #27438, #6035 ) ;
#26233 = CARTESIAN_POINT ( 'NONE',  ( 23.50667118420000179, -14.84174322970000048, 225.0000014190000002 ) ) ;
#26234 = CARTESIAN_POINT ( 'NONE',  ( 4.885731121091885676, 11.07235364852818549, 232.0000002394077967 ) ) ;
#26235 = CARTESIAN_POINT ( 'NONE',  ( -16.77890539070889275, -7.900403655799213887, 0.000000000000000000 ) ) ;
#26236 = CARTESIAN_POINT ( 'NONE',  ( 24.96253706050071131, 13.75225324050492581, 5.310538874999992665 ) ) ;
#26237 = EDGE_CURVE ( 'NONE', #21919, #8607, #1392, .T. ) ;
#26238 = ORIENTED_EDGE ( 'NONE', *, *, #15780, .T. ) ;
#26239 = CARTESIAN_POINT ( 'NONE',  ( 10.32522729140000095, -24.73114799960000099, -1.399999999999998579 ) ) ;
#26240 = EDGE_CURVE ( 'NONE', #28488, #25231, #20903, .T. ) ;
#26241 = EDGE_LOOP ( 'NONE', ( #344, #25185 ) ) ;
#26242 = EDGE_CURVE ( 'NONE', #15285, #17294, #15864, .T. ) ;
#26243 = CARTESIAN_POINT ( 'NONE',  ( 8.350000000651883525, -22.83323352209971091, -39.84673050092360569 ) ) ;
#26244 = VECTOR ( 'NONE', #17256, 1000.000000000000114 ) ;
#26245 = EDGE_CURVE ( 'NONE', #11243, #22220, #28442, .T. ) ;
#26246 = TOROIDAL_SURFACE ( 'NONE', #16685, 24.50000000000000000, 4.000000000000000000 ) ;
#26247 = CARTESIAN_POINT ( 'NONE',  ( -0.05052225346893063351, 4.317558364482401601, -57.31818518972499987 ) ) ;
#26248 = VERTEX_POINT ( 'NONE', #30658 ) ;
#26249 = VERTEX_POINT ( 'NONE', #4212 ) ;
#26250 = CARTESIAN_POINT ( 'NONE',  ( 8.700000000229927366, -28.07050130669910715, -25.59757157921452020 ) ) ;
#26251 = ORIENTED_EDGE ( 'NONE', *, *, #20172, .F. ) ;
#26252 = CARTESIAN_POINT ( 'NONE',  ( 1.484924240490000047, 1.484924240490000047, 227.6412452697800006 ) ) ;
#26253 = CARTESIAN_POINT ( 'NONE',  ( 4.638687372223566641, -10.37384054538513567, -34.08841197926504663 ) ) ;
#26254 = CARTESIAN_POINT ( 'NONE',  ( -2.753981004559999946, -11.98181634260000017, 232.6627648150000027 ) ) ;
#26255 = CARTESIAN_POINT ( 'NONE',  ( -27.52676963214412353, -0.5008603480660359653, 0.2686740700000300741 ) ) ;
#26256 = APPLICATION_CONTEXT ( 'automotive_design' ) ;
#26257 = CARTESIAN_POINT ( 'NONE',  ( 8.700000000277853474, -18.40140086067256320, -36.11849812464715370 ) ) ;
#26258 = CARTESIAN_POINT ( 'NONE',  ( -2.723504195107721237, -4.795398582787750108, -5.685065142700003626 ) ) ;
#26259 = CARTESIAN_POINT ( 'NONE',  ( -22.69220507780000062, -20.05882317629999889, 230.6577119970000069 ) ) ;
#26260 = ORIENTED_EDGE ( 'NONE', *, *, #12614, .F. ) ;
#26261 = CARTESIAN_POINT ( 'NONE',  ( 8.000000000291789704, -9.149979919790938609, -35.02638174844400965 ) ) ;
#26262 = CARTESIAN_POINT ( 'NONE',  ( 2.949882002856674124, 3.605460750137338799, -20.25622222230000347 ) ) ;
#26263 = CARTESIAN_POINT ( 'NONE',  ( -1.828693153457167320, 3.499999999999999112, 230.5790337530978888 ) ) ;
#26264 = CARTESIAN_POINT ( 'NONE',  ( 349323.8516742420034, -54523.81728454602126, -353320.2493477302487 ) ) ;
#26265 = AXIS2_PLACEMENT_3D ( 'NONE', #15007, #21940, #10131 ) ;
#26266 = CARTESIAN_POINT ( 'NONE',  ( -12.09628639100000136, -1.465387503939999947, 230.6412452697800006 ) ) ;
#26267 = CARTESIAN_POINT ( 'NONE',  ( -15.93069263124182555, -8.365606382343615977, 0.000000000000000000 ) ) ;
#26268 = CARTESIAN_POINT ( 'NONE',  ( -4.884981308350000102E-15, -2.100000000000000089, 227.6412452697800006 ) ) ;
#26269 = CARTESIAN_POINT ( 'NONE',  ( -17.79876841389999598, -8.472631907500000281, -0.7999999992999995424 ) ) ;
#26270 = CARTESIAN_POINT ( 'NONE',  ( 11.08346179031908640, -28.41490585489483678, 93.60555127549999099 ) ) ;
#26271 = CARTESIAN_POINT ( 'NONE',  ( -24.47278419579111386, -14.60601539740217092, 6.095965388000001539 ) ) ;
#26272 = CARTESIAN_POINT ( 'NONE',  ( 8.999999999770000869, 21.70000000070000112, -44.94917764161499463 ) ) ;
#26273 = ORIENTED_EDGE ( 'NONE', *, *, #12266, .T. ) ;
#26274 = CARTESIAN_POINT ( 'NONE',  ( 8.700000000248314436, -24.01191590399745479, -28.87649232339336081 ) ) ;
#26275 = DIRECTION ( 'NONE',  ( -0.000000000000000000, -0.000000000000000000, -1.000000000000000000 ) ) ;
#26276 = EDGE_CURVE ( 'NONE', #5374, #27866, #30502, .T. ) ;
#26277 = DIRECTION ( 'NONE',  ( 0.000000000000000000, 0.000000000000000000, -1.000000000000000000 ) ) ;
#26278 = ORIENTED_EDGE ( 'NONE', *, *, #3349, .T. ) ;
#26279 = CARTESIAN_POINT ( 'NONE',  ( -21.30888436558564791, -16.34772642260388409, 186.7828584121667177 ) ) ;
#26280 = CARTESIAN_POINT ( 'NONE',  ( -3.362912017748242999, 4.936852587875802278, -48.53391720692499689 ) ) ;
#26281 = ORIENTED_EDGE ( 'NONE', *, *, #7883, .T. ) ;
#26282 = ORIENTED_EDGE ( 'NONE', *, *, #12379, .T. ) ;
#26283 = DIRECTION ( 'NONE',  ( 1.000000000000000000, 0.000000000000000000, 0.000000000000000000 ) ) ;
#26284 = ORIENTED_EDGE ( 'NONE', *, *, #9259, .F. ) ;
#26285 = CARTESIAN_POINT ( 'NONE',  ( -0.03443693864410000277, -27.80022362959999782, 223.9000014189999774 ) ) ;
#26286 = EDGE_LOOP ( 'NONE', ( #7688, #17810, #9676, #13781, #4852, #19360, #6920, #12649 ) ) ;
#26287 = AXIS2_PLACEMENT_3D ( 'NONE', #17320, #26766, #7867 ) ;
#26288 = CARTESIAN_POINT ( 'NONE',  ( 4.276011752548591005, -51.11187400310260642, -27.80500476121942199 ) ) ;
#26289 = CARTESIAN_POINT ( 'NONE',  ( -6.393889225687406253, -8.665023291132417427, -36.59076075278051832 ) ) ;
#26290 = DIRECTION ( 'NONE',  ( -1.000000000000000000, 0.000000000000000000, 3.489272357540000343E-15 ) ) ;
#26291 = CARTESIAN_POINT ( 'NONE',  ( 0.5114632729423386204, 4.239061013832984948, -35.69999999999999574 ) ) ;
#26292 = CARTESIAN_POINT ( 'NONE',  ( 18.62215279828695458, 19.99998923236033832, -0.6161023301325340151 ) ) ;
#26293 = CARTESIAN_POINT ( 'NONE',  ( -24.09407738750993033, 13.86899051154378881, 6.002806299999996043 ) ) ;
#26294 = LINE ( 'NONE', #16684, #12110 ) ;
#26295 = CARTESIAN_POINT ( 'NONE',  ( -19.80526744929999694, 19.50877353739999975, 229.0739196179999908 ) ) ;
#26296 = EDGE_CURVE ( 'NONE', #12935, #15367, #18947, .T. ) ;
#26297 = ORIENTED_EDGE ( 'NONE', *, *, #1841, .F. ) ;
#26298 = CARTESIAN_POINT ( 'NONE',  ( 0.1708583496781539146, 4.358252033550397364, -8.437690181099997133 ) ) ;
#26299 = CARTESIAN_POINT ( 'NONE',  ( 5.307277461537168506, -2.951504967840870464, -26.33037294500000058 ) ) ;
#26300 = FACE_OUTER_BOUND ( 'NONE', #3154, .T. ) ;
#26301 = CARTESIAN_POINT ( 'NONE',  ( 23.73992238019999945, -12.43607998449999918, 225.0000000000000000 ) ) ;
#26302 = VECTOR ( 'NONE', #19089, 1000.000000000000000 ) ;
#26303 = CARTESIAN_POINT ( 'NONE',  ( -27.79999999999999716, -2.360778239559999931E-11, 229.0000000000000000 ) ) ;
#26304 = CARTESIAN_POINT ( 'NONE',  ( 13.00000000000000178, 24.78814172431745533, -59.85618379852729731 ) ) ;
#26305 = CARTESIAN_POINT ( 'NONE',  ( 2.618538529469180531, 3.470429992801026042, -14.22796858840000311 ) ) ;
#26307 = ADVANCED_FACE ( 'NONE', ( #23584, #20580 ), #8928, .F. ) ;
#26306 = VECTOR ( 'NONE', #19571, 1000.000000000000114 ) ;
#26308 = PRODUCT_DEFINITION_SHAPE ( 'NONE', 'NONE',  #31134 ) ;
#26309 = B_SPLINE_CURVE_WITH_KNOTS ( 'NONE', 5,
 ( #65, #14382, #14688, #23980, #12008, #21615, #19246, #24276, #28833, #7290, #16879, #834, #22544, #5845, #24901 ),
 .UNSPECIFIED., .F., .F.,
 ( 6, 3, 3, 3, 6 ),
 ( 0.000000000000000000, 0.2999999999989615973, 0.5999999999979230836, 0.7999999999996538769, 1.000000000000000000 ),
 .UNSPECIFIED. ) ;
#26310 = COLOUR_RGB ( '', 0.08235294, 0.09019608, 0.10196078) ;
#26311 = DIRECTION ( 'NONE',  ( 1.000000000000000000, -1.224606353820000075E-16, 0.000000000000000000 ) ) ;
#26312 = CARTESIAN_POINT ( 'NONE',  ( 24.41841038956698640, 14.69667349781389376, 6.099998581000020792 ) ) ;
#26313 = CARTESIAN_POINT ( 'NONE',  ( -1.091910126141098170, -3.499798787989274462, 230.7405105397821785 ) ) ;
#26314 = ORIENTED_EDGE ( 'NONE', *, *, #28875, .F. ) ;
#26315 = AXIS2_PLACEMENT_3D ( 'NONE', #12738, #26753, #648 ) ;
#26316 = CARTESIAN_POINT ( 'NONE',  ( -1.243449787579999883E-14, 0.000000000000000000, -0.6999999999999992895 ) ) ;
#26317 = CARTESIAN_POINT ( 'NONE',  ( -6.085238278930475531, -0.01014600953121863602, -28.16856466009999593 ) ) ;
#26318 = ORIENTED_EDGE ( 'NONE', *, *, #5246, .T. ) ;
#26319 = CARTESIAN_POINT ( 'NONE',  ( -7.999999999669004325, -18.23122067930106027, -34.51216076568240965 ) ) ;
#26320 = CARTESIAN_POINT ( 'NONE',  ( 23.81776757409229361, 15.65134803726813217, 4.895813257000003915 ) ) ;
#26321 = ORIENTED_EDGE ( 'NONE', *, *, #30400, .T. ) ;
#26322 = EDGE_LOOP ( 'NONE', ( #27295, #25066, #3065, #28779 ) ) ;
#26323 = ORIENTED_EDGE ( 'NONE', *, *, #17090, .F. ) ;
#26324 =( NAMED_UNIT ( * ) SI_UNIT ( $, .STERADIAN. ) SOLID_ANGLE_UNIT ( ) );
#26325 = ORIENTED_EDGE ( 'NONE', *, *, #19938, .F. ) ;
#26326 = CARTESIAN_POINT ( 'NONE',  ( -17.49999999969999820, -26.21905350739292473, -31.32349012542221089 ) ) ;
#26327 = ADVANCED_FACE ( 'NONE', ( #8606 ), #23262, .F. ) ;
#26328 = FACE_OUTER_BOUND ( 'NONE', #24293, .T. ) ;
#26330 = FACE_BOUND ( 'NONE', #19971, .T. ) ;
#26329 = AXIS2_PLACEMENT_3D ( 'NONE', #27388, #24882, #5982 ) ;
#26331 = AXIS2_PLACEMENT_3D ( 'NONE', #3649, #23178, #15311 ) ;
#26332 = EDGE_LOOP ( 'NONE', ( #25033, #761, #593, #6500, #13414 ) ) ;
#26333 = LINE ( 'NONE', #62, #26488 ) ;
#26334 = VECTOR ( 'NONE', #2935, 1000.000000000000114 ) ;
#26335 = LINE ( 'NONE', #26482, #10521 ) ;
#26336 = CARTESIAN_POINT ( 'NONE',  ( 10.45000000009999930, -30.05766787309999799, -27.53807693043399851 ) ) ;
#26337 = CARTESIAN_POINT ( 'NONE',  ( 3.538401481699890994, -3.323650355412237190, -0.6997877701626019631 ) ) ;
#26338 = VERTEX_POINT ( 'NONE', #4060 ) ;
#26339 = CARTESIAN_POINT ( 'NONE',  ( -19.44855986669129777, 20.00001404973996699, -0.2987059375404466643 ) ) ;
#26340 = B_SPLINE_SURFACE_WITH_KNOTS ( 'NONE', 5, 1, ( 
 ( #19874, #3480 ),
 ( #26788, #22229 ),
 ( #26950, #29455 ),
 ( #8045, #10117 ),
 ( #987, #17345 ),
 ( #14993, #12932 ),
 ( #3173, #10721 ),
 ( #24437, #27253 ),
 ( #2872, #7741 ) ),
 .UNSPECIFIED., .F., .F., .F.,
 ( 6, 3, 6 ),
 ( 2, 2 ),
 ( 0.000000000000000000, 55.31395511720000258, 94.75474465359999954 ),
 ( -3.500000000000000000, 3.500000000000000000 ),
 .UNSPECIFIED. ) ;
#26341 = CARTESIAN_POINT ( 'NONE',  ( 4.543782907447139863, 1.343478130985185537, -16.60440840229999893 ) ) ;
#26342 = CARTESIAN_POINT ( 'NONE',  ( 10.69999999999999929, -130.0000000000000000, -22.39999999999999858 ) ) ;
#26343 = DIRECTION ( 'NONE',  ( -0.3090169943750401549, -0.9510565162951233331, 0.000000000000000000 ) ) ;
#26344 = ORIENTED_EDGE ( 'NONE', *, *, #27977, .F. ) ;
#26345 = CARTESIAN_POINT ( 'NONE',  ( 1.776356839399999804E-15, -5.329070518200000398E-15, 228.3912452697800006 ) ) ;
#26346 = CARTESIAN_POINT ( 'NONE',  ( 0.7459188900473354700, -27.79046661982714639, 3.920206710000012862 ) ) ;
#26347 = CARTESIAN_POINT ( 'NONE',  ( -24.83827471527357744, 12.48687850854618198, 4.999998581000003384 ) ) ;
#26348 = ADVANCED_FACE ( 'NONE', ( #1701 ), #20739, .F. ) ;
#26349 = CARTESIAN_POINT ( 'NONE',  ( -8.699999999715885224, -26.99999999997790923, -28.40000000002690683 ) ) ;
#26350 = DIRECTION ( 'NONE',  ( -0.9880370573969197157, 0.1542166437529879364, 0.000000000000000000 ) ) ;
#26351 = CARTESIAN_POINT ( 'NONE',  ( 26.80000000000000071, 3.197442310919999608E-14, 230.0000000000000000 ) ) ;
#26352 = CARTESIAN_POINT ( 'NONE',  ( -16.30907199849999856, 8.426333778950001019, 230.6999999999999886 ) ) ;
#26353 = B_SPLINE_CURVE_WITH_KNOTS ( 'NONE', 3,
 ( #24642, #27000, #3539, #3076, #13135, #888 ),
 .UNSPECIFIED., .F., .F.,
 ( 4, 2, 4 ),
 ( 0.000000000000000000, 0.5000000000000000000, 1.000000000000000000 ),
 .UNSPECIFIED. ) ;
#26354 = ORIENTED_EDGE ( 'NONE', *, *, #13862, .T. ) ;
#26355 = CARTESIAN_POINT ( 'NONE',  ( -10.69999999999999929, -24.24512542849999974, -29.64315313870000068 ) ) ;
#26356 = DIRECTION ( 'NONE',  ( 0.000000000000000000, 0.9396926207858126157, 0.3420201433259318913 ) ) ;
#26357 = AXIS2_PLACEMENT_3D ( 'NONE', #5672, #17774, #27232 ) ;
#26358 = VECTOR ( 'NONE', #79, 1000.000000000000000 ) ;
#26359 = VECTOR ( 'NONE', #14766, 1000.000000000000114 ) ;
#26360 = CARTESIAN_POINT ( 'NONE',  ( 1.409024965274377150, -4.735590434768029766, -68.10000000002503384 ) ) ;
#26361 = DIRECTION ( 'NONE',  ( -1.000000000000000000, 0.000000000000000000, 0.000000000000000000 ) ) ;
#26362 = EDGE_CURVE ( 'NONE', #24890, #25397, #10693, .T. ) ;
#26363 = ORIENTED_EDGE ( 'NONE', *, *, #22789, .T. ) ;
#26364 = EDGE_CURVE ( 'NONE', #14172, #25001, #23112, .T. ) ;
#26365 = CARTESIAN_POINT ( 'NONE',  ( 25.89948290199999903, 7.563190779290000165, 230.6999999999999886 ) ) ;
#26366 = ORIENTED_EDGE ( 'NONE', *, *, #16214, .F. ) ;
#26367 = CARTESIAN_POINT ( 'NONE',  ( 24.41841038956698640, 14.69667349781389376, 6.099998581000020792 ) ) ;
#26368 = CARTESIAN_POINT ( 'NONE',  ( -1.084269253894827534, -5.810518403417324507, -67.90745670422499813 ) ) ;
#26369 = ORIENTED_EDGE ( 'NONE', *, *, #26063, .F. ) ;
#26370 = CARTESIAN_POINT ( 'NONE',  ( 3.430850994441077439, -5.010772104901466406, -27.73292313649999841 ) ) ;
#26371 = DIRECTION ( 'NONE',  ( -1.000000000000000000, -2.587524353642439916E-24, -2.257144471329210308E-12 ) ) ;
#26372 = EDGE_CURVE ( 'NONE', #26433, #21744, #8796, .T. ) ;
#26373 = CARTESIAN_POINT ( 'NONE',  ( 4.508719565894415915, 1.847421675581904843, -60.89141554682500157 ) ) ;
#26375 = DIRECTION ( 'NONE',  ( 1.000000000000000000, 0.000000000000000000, 0.000000000000000000 ) ) ;
#26374 = VECTOR ( 'NONE', #17165, 1000.000000000000114 ) ;
#26376 = AXIS2_PLACEMENT_3D ( 'NONE', #8210, #27271, #22562 ) ;
#26377 = CARTESIAN_POINT ( 'NONE',  ( 1.071601127087828287, -27.47917021045937958, 224.7132485889944746 ) ) ;
#26378 = DIRECTION ( 'NONE',  ( -1.000000000000000000, 0.000000000000000000, 0.000000000000000000 ) ) ;
#26379 = AXIS2_PLACEMENT_3D ( 'NONE', #4288, #1929, #30247 ) ;
#26380 = UNCERTAINTY_MEASURE_WITH_UNIT (LENGTH_MEASURE( 1.000000000000000082E-05 ), #93, 'distance_accuracy_value', 'NONE');
#26381 = CARTESIAN_POINT ( 'NONE',  ( -7.999999999684150431, -16.34187081459762680, -33.05013248324110720 ) ) ;
#26382 = EDGE_CURVE ( 'NONE', #22250, #21103, #20066, .T. ) ;
#26383 = DIRECTION ( 'NONE',  ( 0.000000000000000000, 0.000000000000000000, -1.000000000000000000 ) ) ;
#26384 = ORIENTED_EDGE ( 'NONE', *, *, #27405, .T. ) ;
#26385 = CARTESIAN_POINT ( 'NONE',  ( 22.36170820408901960, 17.71391973664089292, 6.000000000000005329 ) ) ;
#26386 = CARTESIAN_POINT ( 'NONE',  ( 3.269803491262430306, -2.171870132384594587, -35.34814375549996157 ) ) ;
#26387 = FACE_OUTER_BOUND ( 'NONE', #3365, .T. ) ;
#26388 = CARTESIAN_POINT ( 'NONE',  ( -22.83911268609999823, 16.42879705509999866, 224.8000000000000114 ) ) ;
#26389 = CARTESIAN_POINT ( 'NONE',  ( -10.69999999999999929, 19.99999999999999645, -22.39999999999999858 ) ) ;
#26390 = CARTESIAN_POINT ( 'NONE',  ( -1.346291201779999946, -3.434453875705480108, -72.25672407562892374 ) ) ;
#26391 = DIRECTION ( 'NONE',  ( 5.962915006522622422E-16, 0.4383711467890810676, 0.8987940462991651502 ) ) ;
#26392 = CARTESIAN_POINT ( 'NONE',  ( -24.44014312407112399, 13.24968496200000523, 3.920132093000017193 ) ) ;
#26393 = DIRECTION ( 'NONE',  ( 1.000000000000000000, -0.000000000000000000, -2.257150022439999944E-12 ) ) ;
#26394 = EDGE_CURVE ( 'NONE', #19664, #528, #6874, .T. ) ;
#26395 = CARTESIAN_POINT ( 'NONE',  ( -6.585786437629999490, -16.41511111490214603, -74.85294138696069410 ) ) ;
#26396 = CARTESIAN_POINT ( 'NONE',  ( -27.53132593009999951, -1.221706759790000127E-11, 229.7313259299999686 ) ) ;
#26397 = CARTESIAN_POINT ( 'NONE',  ( -8.699999999683917906, -16.84112679184576677, -33.19732076807623145 ) ) ;
#26398 = ORIENTED_EDGE ( 'NONE', *, *, #13481, .F. ) ;
#26399 = AXIS2_PLACEMENT_3D ( 'NONE', #19548, #21917, #22214 ) ;
#26400 = CARTESIAN_POINT ( 'NONE',  ( 9.999999999969999109, -24.00000000000000000, -28.40000000000000213 ) ) ;
#26401 = ORIENTED_EDGE ( 'NONE', *, *, #19186, .T. ) ;
#26402 = CARTESIAN_POINT ( 'NONE',  ( 25.17364887440000132, -13.36205984479999920, 225.5069763079999916 ) ) ;
#26403 = CARTESIAN_POINT ( 'NONE',  ( 4.003591150705128499, -2.204345408526048988, -58.70843849682500348 ) ) ;
#26404 = ORIENTED_EDGE ( 'NONE', *, *, #10942, .F. ) ;
#26405 = ORIENTED_EDGE ( 'NONE', *, *, #24992, .T. ) ;
#26406 = DIRECTION ( 'NONE',  ( -1.000000000000000000, 0.000000000000000000, 0.000000000000000000 ) ) ;
#26407 = ORIENTED_EDGE ( 'NONE', *, *, #27163, .F. ) ;
#26408 = VECTOR ( 'NONE', #16387, 1000.000000000000114 ) ;
#26409 = AXIS2_PLACEMENT_3D ( 'NONE', #19042, #21570, #11653 ) ;
#26410 = CARTESIAN_POINT ( 'NONE',  ( -23.83006840756495137, 14.31758445875128594, 4.492876031000014869 ) ) ;
#26411 = CARTESIAN_POINT ( 'NONE',  ( 9.097977789939999838, 19.99999999999999645, -43.40000000045500173 ) ) ;
#26412 = CARTESIAN_POINT ( 'NONE',  ( 16.58866331865612409, 11.94697101960596974, -1.400000000000001688 ) ) ;
#26413 = CARTESIAN_POINT ( 'NONE',  ( 14.25032083441342934, -27.35421241409322946, 8.000000000000007105 ) ) ;
#26414 = ADVANCED_FACE ( 'NONE', ( #26547 ), #28600, .T. ) ;
#26415 = DIRECTION ( 'NONE',  ( -5.551115123130000150E-16, -1.000000000000000000, 0.000000000000000000 ) ) ;
#26416 = CARTESIAN_POINT ( 'NONE',  ( 4.116710911288352648, -1.508563155650267884, -5.836105321700007842 ) ) ;
#26417 = CARTESIAN_POINT ( 'NONE',  ( 27.29823224869999976, -7.151321944500000249, 230.6577119970000069 ) ) ;
#26418 = ORIENTED_EDGE ( 'NONE', *, *, #14486, .F. ) ;
#26419 = DIRECTION ( 'NONE',  ( 0.000000000000000000, 0.000000000000000000, 1.000000000000000000 ) ) ;
#26420 = EDGE_CURVE ( 'NONE', #7280, #4633, #7307, .T. ) ;
#26421 = CARTESIAN_POINT ( 'NONE',  ( 0.5830502407437251344, -4.723335260236232180, -19.30804674910000784 ) ) ;
#26422 = CARTESIAN_POINT ( 'NONE',  ( -0.8233448747507865484, -27.78811367915593777, 225.7327679764803179 ) ) ;
#26423 = B_SPLINE_CURVE_WITH_KNOTS ( 'NONE', 3,
 ( #30233, #6625, #20795, #18263, #28183, #11510, #1294, #1454, #13230, #30405 ),
 .UNSPECIFIED., .F., .F.,
 ( 4, 2, 2, 2, 4 ),
 ( 0.000000000000000000, 0.2500000000000000555, 0.5000000000000000000, 0.7499999999999998890, 1.000000000000000000 ),
 .UNSPECIFIED. ) ;
#26424 = CARTESIAN_POINT ( 'NONE',  ( -3.040504021322313122, -1.733590290792417887, 0.000000000000000000 ) ) ;
#26425 = ADVANCED_FACE ( 'NONE', ( #14440 ), #11259, .F. ) ;
#26426 = CARTESIAN_POINT ( 'NONE',  ( 25.46368747440213198, -12.80129684534102807, 4.999998581000003384 ) ) ;
#26427 = CARTESIAN_POINT ( 'NONE',  ( -15.74934601578848614, -8.774721957951193474, 0.000000000000000000 ) ) ;
#26428 = CARTESIAN_POINT ( 'NONE',  ( 3.498556269673057884, -2.323812390827893815, -42.60875473022500159 ) ) ;
#26429 = CARTESIAN_POINT ( 'NONE',  ( -7.999999999945165641, -111.9817663798748981, 5.760339591700875950 ) ) ;
#26430 = LINE ( 'NONE', #12249, #6217 ) ;
#26431 = CARTESIAN_POINT ( 'NONE',  ( -24.32472894358752313, 13.45989150749028873, 6.099998581000020792 ) ) ;
#26432 = CARTESIAN_POINT ( 'NONE',  ( 10.00000000000000000, 4.552933401020911042, -69.34955285734142194 ) ) ;
#26433 = VERTEX_POINT ( 'NONE', #9555 ) ;
#26434 = CARTESIAN_POINT ( 'NONE',  ( -3.052438874386664835, 3.509528713898347974, -28.58728588869999143 ) ) ;
#26435 = CARTESIAN_POINT ( 'NONE',  ( -7.999999999654498595, -13.74237167848310115, -36.71272273345665837 ) ) ;
#26436 = ORIENTED_EDGE ( 'NONE', *, *, #13585, .F. ) ;
#26437 = CARTESIAN_POINT ( 'NONE',  ( 9.999999999969999109, -24.87872937930000106, -30.52127062269999769 ) ) ;
#26438 = CARTESIAN_POINT ( 'NONE',  ( 3.650437977654107602, 3.794428519304413605, -49.44426496242500235 ) ) ;
#26439 = ORIENTED_EDGE ( 'NONE', *, *, #9712, .F. ) ;
#26440 = ORIENTED_EDGE ( 'NONE', *, *, #24218, .T. ) ;
#26441 =( NAMED_UNIT ( * ) PLANE_ANGLE_UNIT ( ) SI_UNIT ( $, .RADIAN. ) );
#26442 = VERTEX_POINT ( 'NONE', #7352 ) ;
#26443 = CARTESIAN_POINT ( 'NONE',  ( -0.06887222117169999880, -27.80017212539999960, 223.9013489249999793 ) ) ;
#26444 = ORIENTED_EDGE ( 'NONE', *, *, #27509, .T. ) ;
#26445 = CARTESIAN_POINT ( 'NONE',  ( 17.43374459646987873, 12.07698932438915840, -0.6999999999999784173 ) ) ;
#26446 = CARTESIAN_POINT ( 'NONE',  ( 3.552713678799999608E-15, -3.552713678799999608E-15, 186.7828584120000244 ) ) ;
#26447 = CARTESIAN_POINT ( 'NONE',  ( 22.62517538432032183, 16.36045799713948057, 8.000000000000007105 ) ) ;
#26448 = CARTESIAN_POINT ( 'NONE',  ( 0.4968125066838017245, 4.681645040665504354, -35.70000000000000284 ) ) ;
#26449 = CARTESIAN_POINT ( 'NONE',  ( 18.22359483181848105, 19.99999695154517809, -0.6804351800466643674 ) ) ;
#26450 = CARTESIAN_POINT ( 'NONE',  ( -17.62526668104891314, 11.76353838341477953, -0.6999999999999784173 ) ) ;
#26451 = CARTESIAN_POINT ( 'NONE',  ( -6.292028302495006109, -7.397523702828756598, -33.87115578656446502 ) ) ;
#26452 = DIRECTION ( 'NONE',  ( -0.6343890248118320141, -0.7730139489027949562, 0.000000000000000000 ) ) ;
#26453 = VERTEX_POINT ( 'NONE', #21988 ) ;
#26454 = ADVANCED_FACE ( 'NONE', ( #7648 ), #21366, .F. ) ;
#26455 = CARTESIAN_POINT ( 'NONE',  ( -5.530047734074942767, 3.478668956039820959, -11.04547590279999980 ) ) ;
#26456 = CARTESIAN_POINT ( 'NONE',  ( 3.104103280670445830, -4.533555713950848443, -26.13292313650000409 ) ) ;
#26457 = CARTESIAN_POINT ( 'NONE',  ( -0.7509949761406778945, -3.448174246630094864, 0.000000000000000000 ) ) ;
#26458 = EDGE_CURVE ( 'NONE', #7727, #12643, #21812, .T. ) ;
#26459 = LINE ( 'NONE', #24102, #14706 ) ;
#26460 = CARTESIAN_POINT ( 'NONE',  ( 19.29866511436280874, 19.63492491799039996, 0.3046098590000212436 ) ) ;
#26461 = CARTESIAN_POINT ( 'NONE',  ( -23.56630063319272139, -14.17280417015954619, 225.9948832298492221 ) ) ;
#26462 = CARTESIAN_POINT ( 'NONE',  ( -4.448701673712585070, 0.6187532242676665462, -19.25159460730001371 ) ) ;
#26463 = CARTESIAN_POINT ( 'NONE',  ( -17.49999999969999820, -27.00000000000000000, -28.40000000020000215 ) ) ;
#26464 = CARTESIAN_POINT ( 'NONE',  ( -24.86822223968379575, -13.92223202017373573, 4.319317663000004970 ) ) ;
#26465 = CARTESIAN_POINT ( 'NONE',  ( 10.45000000009999930, -26.99999999999950617, -28.39999999990030588 ) ) ;
#26466 = EDGE_LOOP ( 'NONE', ( #19554, #5671, #3725, #7356 ) ) ;
#26467 = DIRECTION ( 'NONE',  ( 0.000000000000000000, 0.000000000000000000, 1.000000000000000000 ) ) ;
#26468 = LINE ( 'NONE', #12301, #20338 ) ;
#26469 = ORIENTED_EDGE ( 'NONE', *, *, #23556, .T. ) ;
#26470 = CARTESIAN_POINT ( 'NONE',  ( 23.36339467984016594, -14.50559736741132433, 5.674968348874030788 ) ) ;
#26471 = CYLINDRICAL_SURFACE ( 'NONE', #21838, 10.00000000000000533 ) ;
#26472 = VERTEX_POINT ( 'NONE', #26400 ) ;
#26473 = ORIENTED_EDGE ( 'NONE', *, *, #14909, .T. ) ;
#26474 = ORIENTED_EDGE ( 'NONE', *, *, #1230, .T. ) ;
#26475 =( LENGTH_UNIT ( ) NAMED_UNIT ( * ) SI_UNIT ( .MILLI., .METRE. ) );
#26476 = ORIENTED_EDGE ( 'NONE', *, *, #21008, .F. ) ;
#26477 = CARTESIAN_POINT ( 'NONE',  ( -17.49999999969999820, -30.00000000000000000, -28.79765167477413357 ) ) ;
#26478 = CARTESIAN_POINT ( 'NONE',  ( 13.00000000000000000, 24.54213077165692525, -59.94572446259928711 ) ) ;
#26479 = CARTESIAN_POINT ( 'NONE',  ( 16.50668551558484509, 10.10821397331193339, -0.6999999999999784173 ) ) ;
#26480 = ADVANCED_FACE ( 'NONE', ( #19619 ), #12193, .F. ) ;
#26481 = ORIENTED_EDGE ( 'NONE', *, *, #22930, .T. ) ;
#26482 = CARTESIAN_POINT ( 'NONE',  ( 12.80098767942999771, -26.99999999940830264, -34.17350269213999781 ) ) ;
#26483 = CARTESIAN_POINT ( 'NONE',  ( 3.378474373710000034, 11.51459555979999827, 232.0000000000000000 ) ) ;
#26484 = CARTESIAN_POINT ( 'NONE',  ( 10.69999999999999929, -29.30501631380000305, -26.47986985000000004 ) ) ;
#26485 = CARTESIAN_POINT ( 'NONE',  ( 2.715726573628606477, -4.227879611059382370, -0.6999936726990061420 ) ) ;
#26486 = VERTEX_POINT ( 'NONE', #19154 ) ;
#26487 = CARTESIAN_POINT ( 'NONE',  ( -18.42955812989342945, 20.00001476357908814, -0.6532716553696857886 ) ) ;
#26488 = VECTOR ( 'NONE', #7288, 999.9999999999998863 ) ;
#26489 = CARTESIAN_POINT ( 'NONE',  ( 4.130711734062736618, 1.221343755424965316, -17.54190840230000248 ) ) ;
#26490 = CARTESIAN_POINT ( 'NONE',  ( -7.861312627893095595, -5.944809905196246191, -34.57969164752912405 ) ) ;
#26491 = PLANE ( 'NONE',  #18033 ) ;
#26492 = CIRCLE ( 'NONE', #16938, 2.100000000000000089 ) ;
#26493 = ORIENTED_EDGE ( 'NONE', *, *, #18288, .F. ) ;
#26494 = CARTESIAN_POINT ( 'NONE',  ( -12.41036288881528016, -28.33197836327668639, -33.40447669382125895 ) ) ;
#26495 = CARTESIAN_POINT ( 'NONE',  ( 10.99999999979999998, 21.69999999919999212, -70.09999999999999432 ) ) ;
#26496 = CARTESIAN_POINT ( 'NONE',  ( 23.20948082139999968, -13.40000000000000036, 6.099999999630000502 ) ) ;
#26497 = LINE ( 'NONE', #12022, #19507 ) ;
#26498 = PLANE ( 'NONE',  #9683 ) ;
#26499 = PLANE ( 'NONE',  #2694 ) ;
#26500 = CARTESIAN_POINT ( 'NONE',  ( -8.999999999710000864, 20.70710678120000381, -44.39289321881399530 ) ) ;
#26501 = ORIENTED_EDGE ( 'NONE', *, *, #26724, .F. ) ;
#26502 = CARTESIAN_POINT ( 'NONE',  ( -12.31403527401453424, -24.10534946231254239, -24.29772457544500597 ) ) ;
#26503 = B_SPLINE_CURVE_WITH_KNOTS ( 'NONE', 3,
 ( #1656, #18324, #23380, #6369 ),
 .UNSPECIFIED., .F., .F.,
 ( 4, 4 ),
 ( 0.000000000000000000, 1.000000000000000000 ),
 .UNSPECIFIED. ) ;
#26504 = CARTESIAN_POINT ( 'NONE',  ( 0.7004501677642104296, -4.947957971645007724, -68.10000000002501963 ) ) ;
#26505 = FACE_OUTER_BOUND ( 'NONE', #26695, .T. ) ;
#26506 = ORIENTED_EDGE ( 'NONE', *, *, #21907, .F. ) ;
#26507 = EDGE_CURVE ( 'NONE', #26188, #1312, #25707, .T. ) ;
#26508 = VECTOR ( 'NONE', #29413, 1000.000000000000000 ) ;
#26509 = FACE_OUTER_BOUND ( 'NONE', #7429, .T. ) ;
#26510 = SURFACE_STYLE_FILL_AREA ( #16746 ) ;
#26511 = AXIS2_PLACEMENT_3D ( 'NONE', #9409, #5148, #21693 ) ;
#26512 = EDGE_LOOP ( 'NONE', ( #19039, #9285, #7803, #19565 ) ) ;
#26513 = CARTESIAN_POINT ( 'NONE',  ( 2.775954778257573530, 3.272756372082325171, -39.07539910822363538 ) ) ;
#26514 = CARTESIAN_POINT ( 'NONE',  ( 0.2632024292269652954, 4.191744801550177257, -70.10875473022500159 ) ) ;
#26515 = ORIENTED_EDGE ( 'NONE', *, *, #25615, .F. ) ;
#26516 = CARTESIAN_POINT ( 'NONE',  ( -4.215937884789293655, -1.105999120962562809, -25.04656121680000425 ) ) ;
#26517 = EDGE_CURVE ( 'NONE', #21618, #23628, #9707, .T. ) ;
#26518 = CYLINDRICAL_SURFACE ( 'NONE', #4881, 20.00000000000000711 ) ;
#26519 = B_SPLINE_CURVE_WITH_KNOTS ( 'NONE', 5,
 ( #10190, #19791, #11280, #18023, #15845, #30154 ),
 .UNSPECIFIED., .F., .F.,
 ( 6, 6 ),
 ( 0.000000000000000000, 18.58426834389999982 ),
 .UNSPECIFIED. ) ;
#26520 = CARTESIAN_POINT ( 'NONE',  ( -3.221934060409652023, 3.671197199744479001, -53.98587006832499924 ) ) ;
#26521 = DIRECTION ( 'NONE',  ( -3.924189347185962345E-12, 0.4082287037029530552, 0.9128796883888952163 ) ) ;
#26522 = CARTESIAN_POINT ( 'NONE',  ( -23.76534794678204321, -14.42397063190348483, 3.904032100999987875 ) ) ;
#26523 = CARTESIAN_POINT ( 'NONE',  ( 24.22190007760000086, -15.01852807150000046, 224.3193082299999901 ) ) ;
#26524 = CARTESIAN_POINT ( 'NONE',  ( -22.90527192528401201, 16.36193184990112570, 1.000000000000000888 ) ) ;
#26525 = DIRECTION ( 'NONE',  ( -0.6211122697021861372, 0.3379638270947744605, -0.7071067811871500908 ) ) ;
#26526 = AXIS2_PLACEMENT_3D ( 'NONE', #8380, #6657, #23197 ) ;
#26527 = CARTESIAN_POINT ( 'NONE',  ( -17.39542721469608821, -22.00021333527590883, -29.71046973867640872 ) ) ;
#26528 = VERTEX_POINT ( 'NONE', #19311 ) ;
#26529 = CARTESIAN_POINT ( 'NONE',  ( 20.50699588867001211, 18.79637368904402095, 4.000000000000003553 ) ) ;
#26530 = ADVANCED_FACE ( 'NONE', ( #18995 ), #17097, .T. ) ;
#26531 = FACE_OUTER_BOUND ( 'NONE', #21042, .T. ) ;
#26532 = CARTESIAN_POINT ( 'NONE',  ( -23.98258507372315051, -15.39789217239198571, 5.760134161999996394 ) ) ;
#26533 = CIRCLE ( 'NONE', #19503, 4.000000000000000888 ) ;
#26534 = CARTESIAN_POINT ( 'NONE',  ( 7.636659491170000535, 9.305401069080000198, 229.6412452697800006 ) ) ;
#26535 = DIRECTION ( 'NONE',  ( 1.000000000000000000, 0.000000000000000000, 0.000000000000000000 ) ) ;
#26536 = LINE ( 'NONE', #21818, #24585 ) ;
#26537 = FACE_OUTER_BOUND ( 'NONE', #20062, .T. ) ;
#26538 = CIRCLE ( 'NONE', #4436, 2.299999999979998933 ) ;
#26539 = CARTESIAN_POINT ( 'NONE',  ( -0.9003584917538117738, -26.78512143702961268, 225.6334870514607189 ) ) ;
#26540 = FACE_BOUND ( 'NONE', #2625, .T. ) ;
#26541 = CARTESIAN_POINT ( 'NONE',  ( 23.52223098035388205, -14.81718486479981323, 225.2893105631158051 ) ) ;
#26542 = DIRECTION ( 'NONE',  ( -1.000000000000000000, 0.000000000000000000, 0.000000000000000000 ) ) ;
#26543 = CARTESIAN_POINT ( 'NONE',  ( -27.50000000000000000, 0.000000000000000000, 143.6055512749999821 ) ) ;
#26544 = DIRECTION ( 'NONE',  ( 0.7198537139083028835, -0.6941258031311204890, 0.000000000000000000 ) ) ;
#26545 = ORIENTED_EDGE ( 'NONE', *, *, #30762, .F. ) ;
#26546 = VECTOR ( 'NONE', #11316, 1000.000000000000000 ) ;
#26547 = FACE_OUTER_BOUND ( 'NONE', #29130, .T. ) ;
#26548 = VERTEX_POINT ( 'NONE', #2786 ) ;
#26549 = CARTESIAN_POINT ( 'NONE',  ( 24.09856112909999837, -15.21545593799999985, 225.0000014190000002 ) ) ;
#26550 = EDGE_CURVE ( 'NONE', #3906, #26249, #4679, .T. ) ;
#26551 = CARTESIAN_POINT ( 'NONE',  ( -0.05052225346893526176, 4.317558364482406930, -57.71818518972499845 ) ) ;
#26552 = ORIENTED_EDGE ( 'NONE', *, *, #20592, .F. ) ;
#26553 = ADVANCED_FACE ( 'NONE', ( #23735 ), #7428, .T. ) ;
#26554 = ITEM_DEFINED_TRANSFORMATION ( 'NONE', 'NONE', #9829,  #17722 ) ;
#26555 = VERTEX_POINT ( 'NONE', #1199 ) ;
#26557 = DIRECTION ( 'NONE',  ( 1.000000000000000000, 0.000000000000000000, 0.000000000000000000 ) ) ;
#26556 = AXIS2_PLACEMENT_3D ( 'NONE', #22807, #4082, #25488 ) ;
#26558 = ORIENTED_EDGE ( 'NONE', *, *, #15468, .T. ) ;
#26559 = CARTESIAN_POINT ( 'NONE',  ( 2.033405199262924956, 0.5436710260910023740, 226.6412452697799438 ) ) ;
#26560 = DIRECTION ( 'NONE',  ( 0.000000000000000000, 0.9396926207858125046, 0.3420201433259318358 ) ) ;
#26561 = CARTESIAN_POINT ( 'NONE',  ( 9.665310091690001215, 19.99999999999999645, -43.14889995884200147 ) ) ;
#26562 = CARTESIAN_POINT ( 'NONE',  ( 12.10980759760000147, 2.370578709670000173, 232.6627648150000027 ) ) ;
#26563 = FACE_OUTER_BOUND ( 'NONE', #665, .T. ) ;
#26564 = CARTESIAN_POINT ( 'NONE',  ( -2.564224011386423641, 5.541743391105337757, -7.131725184300004017 ) ) ;
#26565 = CARTESIAN_POINT ( 'NONE',  ( 28.35924375230000294, -7.429275285240000137, 229.7625741969999922 ) ) ;
#26566 = ORIENTED_EDGE ( 'NONE', *, *, #14593, .T. ) ;
#26567 = CARTESIAN_POINT ( 'NONE',  ( -2.118729980851755901, -4.637508198188047714, -44.10000000002499121 ) ) ;
#26568 = EDGE_CURVE ( 'NONE', #10260, #23969, #21792, .T. ) ;
#26569 = VECTOR ( 'NONE', #26378, 1000.000000000000000 ) ;
#26570 = CARTESIAN_POINT ( 'NONE',  ( 6.096654317658788180, 0.1519075334363156893, -20.67661200060000226 ) ) ;
#26571 = CARTESIAN_POINT ( 'NONE',  ( -0.5500250885004874801, -27.79512802401430704, 225.9640385793438497 ) ) ;
#26572 = PLANE ( 'NONE',  #28082 ) ;
#26573 = EDGE_CURVE ( 'NONE', #16174, #20501, #15199, .T. ) ;
#26574 = CARTESIAN_POINT ( 'NONE',  ( -3.389121577140000063, -11.55088360979999962, 230.6412452697800006 ) ) ;
#26575 = CARTESIAN_POINT ( 'NONE',  ( 21.81274943930000276, 17.27884304029999640, 223.9999999570000000 ) ) ;
#26576 = CARTESIAN_POINT ( 'NONE',  ( -19.06860189597471944, 19.69237645765742073, 0.2003674019999956979 ) ) ;
#26577 = EDGE_CURVE ( 'NONE', #528, #16211, #27314, .T. ) ;
#26578 = CARTESIAN_POINT ( 'NONE',  ( -7.999999999965972108, -115.9769488450772741, 9.394897729457213131 ) ) ;
#26579 = CARTESIAN_POINT ( 'NONE',  ( 0.8178280466645336810, -26.78758467633450735, 224.2627730065052560 ) ) ;
#26580 = DIRECTION ( 'NONE',  ( 1.000000000000000000, 0.000000000000000000, 0.000000000000000000 ) ) ;
#26581 = CIRCLE ( 'NONE', #13000, 27.69999999999999929 ) ;
#26582 = CARTESIAN_POINT ( 'NONE',  ( -24.60726957497166367, 14.37955347300500364, 5.901399683999997592 ) ) ;
#26583 = CARTESIAN_POINT ( 'NONE',  ( 2.895630725101784542, -26.64812433595226437, 20.04809298185875832 ) ) ;
#26584 = VERTEX_POINT ( 'NONE', #5753 ) ;
#26585 = CARTESIAN_POINT ( 'NONE',  ( 4.634019325638262465, 0.4639887426745106791, -29.63116556699998938 ) ) ;
#26586 = EDGE_CURVE ( 'NONE', #15092, #6979, #5787, .T. ) ;
#26587 = ORIENTED_EDGE ( 'NONE', *, *, #4438, .T. ) ;
#26588 = CARTESIAN_POINT ( 'NONE',  ( 23.88846875300728456, -13.62395840476969688, 3.900000000370010156 ) ) ;
#26589 = CARTESIAN_POINT ( 'NONE',  ( -1.909971040720825908, -5.612411004515823088, -46.99520033292500187 ) ) ;
#26590 = VERTEX_POINT ( 'NONE', #24496 ) ;
#26591 = ORIENTED_EDGE ( 'NONE', *, *, #25640, .T. ) ;
#26592 = VECTOR ( 'NONE', #13477, 1000.000000000000000 ) ;
#26593 = EDGE_CURVE ( 'NONE', #6267, #30881, #29517, .T. ) ;
#26594 = ORIENTED_EDGE ( 'NONE', *, *, #20399, .T. ) ;
#26595 = CARTESIAN_POINT ( 'NONE',  ( -7.999999999730326827, -27.47149743197635630, -25.42634137633946878 ) ) ;
#26596 = ORIENTED_EDGE ( 'NONE', *, *, #10220, .T. ) ;
#26597 = CARTESIAN_POINT ( 'NONE',  ( -24.49999999470000134, 3.000285566209999917E-15, 39.99999999930000172 ) ) ;
#26598 = CARTESIAN_POINT ( 'NONE',  ( -0.1113126276967127126, 5.146895567835117369, -43.32728369092647824 ) ) ;
#26599 = EDGE_CURVE ( 'NONE', #1366, #12957, #22137, .T. ) ;
#26600 = CARTESIAN_POINT ( 'NONE',  ( 27.07818553041514065, 6.807801137122736712, 8.000000000000007105 ) ) ;
#26601 = CARTESIAN_POINT ( 'NONE',  ( 0.5561711591857212422, 4.217760595753933472, -35.69999999999999574 ) ) ;
#26602 = AXIS2_PLACEMENT_3D ( 'NONE', #26336, #7442, #7742 ) ;
#26603 = CARTESIAN_POINT ( 'NONE',  ( 17.92796488783011455, 19.99992859427167957, -0.6995494494441671929 ) ) ;
#26604 = CARTESIAN_POINT ( 'NONE',  ( -23.83006840756313238, 14.31758445865130369, 5.507121130000014020 ) ) ;
#26605 = CYLINDRICAL_SURFACE ( 'NONE', #5063, 1.099999999999999867 ) ;
#26606 = FACE_OUTER_BOUND ( 'NONE', #3508, .T. ) ;
#26607 = CARTESIAN_POINT ( 'NONE',  ( 0.3624384587677549341, -4.645391411234346180, -9.893384211800000827 ) ) ;
#26608 = CARTESIAN_POINT ( 'NONE',  ( -6.085238278930475531, -0.01014600953121863602, -27.56856466010000517 ) ) ;
#26609 = DIRECTION ( 'NONE',  ( -0.000000000000000000, 1.000000000000000000, -2.257145581549999994E-12 ) ) ;
#26610 = CARTESIAN_POINT ( 'NONE',  ( 24.37165445055180157, -14.77472140295711434, 4.999998581000003384 ) ) ;
#26611 = DIRECTION ( 'NONE',  ( -0.000000000000000000, -0.000000000000000000, -1.000000000000000000 ) ) ;
#26612 = CARTESIAN_POINT ( 'NONE',  ( 4.941595660341814522, -27.05346828916501423, 20.49141012103500259 ) ) ;
#26613 = CARTESIAN_POINT ( 'NONE',  ( -3.099128499470596321, -3.102542665468454253, -9.813991631000003935 ) ) ;
#26614 = CARTESIAN_POINT ( 'NONE',  ( 16.05747815621842989, 10.97464310281671018, -1.400000000000001910 ) ) ;
#26615 = DIRECTION ( 'NONE',  ( -0.000000000000000000, 1.000000000000000000, -2.258510841069999963E-12 ) ) ;
#26616 = CARTESIAN_POINT ( 'NONE',  ( 0.000000000000000000, 0.000000000000000000, 92.06031501460000754 ) ) ;
#26617 = ORIENTED_EDGE ( 'NONE', *, *, #28930, .F. ) ;
#26618 = CARTESIAN_POINT ( 'NONE',  ( 10.00000000070000183, -30.00000000000000000, -28.40000000000000213 ) ) ;
#26619 = CARTESIAN_POINT ( 'NONE',  ( -1.346291201189999898, -3.434453875705480108, -72.25672407562892374 ) ) ;
#26620 = VECTOR ( 'NONE', #10381, 1000.000000000000114 ) ;
#26621 = ORIENTED_EDGE ( 'NONE', *, *, #24267, .F. ) ;
#26622 = B_SPLINE_SURFACE_WITH_KNOTS ( 'NONE', 5, 1, ( 
 ( #30879, #16236 ),
 ( #1931, #9149 ),
 ( #28196, #16085 ),
 ( #4590, #21126 ),
 ( #13724, #21275 ),
 ( #11676, #19069 ),
 ( #14046, #6955 ),
 ( #14363, #25697 ),
 ( #4128, #30418 ),
 ( #8837, #1779 ),
 ( #4444, #23650 ),
 ( #16548, #26156 ),
 ( #18752, #25852 ),
 ( #2086, #9310 ),
 ( #18599, #11369 ) ),
 .UNSPECIFIED., .F., .F., .F.,
 ( 6, 3, 3, 3, 6 ),
 ( 2, 2 ),
 ( 0.000000000000000000, 0.5239015560140000138, 1.047803112029999983, 1.571704668039999975, 1.746338520049999898 ),
 ( -0.7000000000009999335, 2.556813327499999719E-06 ),
 .UNSPECIFIED. ) ;
#26623 = CARTESIAN_POINT ( 'NONE',  ( 23.47117976014261131, -14.33053685730250493, 5.880491002250007426 ) ) ;
#26624 = CARTESIAN_POINT ( 'NONE',  ( -16.66884554159437926, 9.902812559993083852, -0.6999999999999783062 ) ) ;
#26625 = ADVANCED_FACE ( 'NONE', ( #12679 ), #15505, .T. ) ;
#26626 = ORIENTED_EDGE ( 'NONE', *, *, #13520, .F. ) ;
#26627 = ORIENTED_EDGE ( 'NONE', *, *, #10470, .F. ) ;
#26628 = ORIENTED_EDGE ( 'NONE', *, *, #6321, .T. ) ;
#26629 = EDGE_CURVE ( 'NONE', #11773, #11717, #6218, .T. ) ;
#26630 = ORIENTED_EDGE ( 'NONE', *, *, #13270, .T. ) ;
#26631 = CARTESIAN_POINT ( 'NONE',  ( 8.699999999949548979, -115.5267901941283810, 21.04701626963504069 ) ) ;
#26632 = ADVANCED_FACE ( 'NONE', ( #10336 ), #744, .F. ) ;
#26633 = EDGE_CURVE ( 'NONE', #22666, #20223, #22679, .T. ) ;
#26634 = LINE ( 'NONE', #6977, #22511 ) ;
#26635 = FACE_OUTER_BOUND ( 'NONE', #6879, .T. ) ;
#26636 = ORIENTED_EDGE ( 'NONE', *, *, #8459, .F. ) ;
#26637 = FACE_OUTER_BOUND ( 'NONE', #18754, .T. ) ;
#26638 = FACE_OUTER_BOUND ( 'NONE', #15783, .T. ) ;
#26639 = DIRECTION ( 'NONE',  ( 0.000000000000000000, 0.000000000000000000, 1.000000000000000000 ) ) ;
#26640 = DIRECTION ( 'NONE',  ( 0.000000000000000000, 0.3420201433259318358, -0.9396926207858125046 ) ) ;
#26641 = ORIENTED_EDGE ( 'NONE', *, *, #6549, .T. ) ;
#26642 = FACE_OUTER_BOUND ( 'NONE', #25789, .T. ) ;
#26643 = CIRCLE ( 'NONE', #30074, 3.200000004570001888 ) ;
#26644 = CARTESIAN_POINT ( 'NONE',  ( -5.853056545089267537, 1.703994407032248581, -15.70443125760000136 ) ) ;
#26645 = LINE ( 'NONE', #74, #26873 ) ;
#26646 = CARTESIAN_POINT ( 'NONE',  ( 0.2195862974910302301, -27.49906791309039633, 6.087643466945557691 ) ) ;
#26647 = DIRECTION ( 'NONE',  ( 1.224606353819999829E-16, 1.000000000000000000, 0.000000000000000000 ) ) ;
#26648 = DIRECTION ( 'NONE',  ( 0.000000000000000000, 0.000000000000000000, 1.000000000000000000 ) ) ;
#26649 = CARTESIAN_POINT ( 'NONE',  ( 26.93395387809999875, -3.298349105250000085E-15, 92.24324102360000666 ) ) ;
#26650 = CARTESIAN_POINT ( 'NONE',  ( 8.000000000839454728, -14.48034092994288180, -33.45092210021663703 ) ) ;
#26651 = B_SPLINE_CURVE_WITH_KNOTS ( 'NONE', 3,
 ( #25572, #13605, #23211, #1654, #18477, #23531, #25888, #6992, #4166, #30608, #23683, #11710, #30753, #11560 ),
 .UNSPECIFIED., .F., .F.,
 ( 4, 2, 2, 2, 2, 2, 4 ),
 ( 0.000000000000000000, 0.1250000000000001388, 0.2500000000000002776, 0.5000000000000002220, 0.7500000000000001110, 0.8750000000000001110, 1.000000000000000000 ),
 .UNSPECIFIED. ) ;
#26652 = CARTESIAN_POINT ( 'NONE',  ( -27.23548387180000319, 3.335274659879999868E-15, 88.33953982590000464 ) ) ;
#26653 = CARTESIAN_POINT ( 'NONE',  ( -11.30445666259999982, -24.42656469639999983, -1.476955128299997533 ) ) ;
#26654 = CARTESIAN_POINT ( 'NONE',  ( 0.000000000000000000, 0.000000000000000000, 231.1412452697749984 ) ) ;
#26655 = ORIENTED_EDGE ( 'NONE', *, *, #4423, .F. ) ;
#26656 = CARTESIAN_POINT ( 'NONE',  ( 5.363076718300177959, -2.525690298526013677, -52.29872167392500160 ) ) ;
#26657 = CARTESIAN_POINT ( 'NONE',  ( 16.40303402075260308, 10.20816091466531716, 0.000000000000000000 ) ) ;
#26658 = CARTESIAN_POINT ( 'NONE',  ( 2.471021819916508822, -4.092477270420384450, -68.10000000002504805 ) ) ;
#26659 = CARTESIAN_POINT ( 'NONE',  ( -7.075849446371014650, 5.588469936758675871, -40.20484807950032291 ) ) ;
#26660 = ORIENTED_EDGE ( 'NONE', *, *, #10289, .T. ) ;
#26661 = DIRECTION ( 'NONE',  ( -1.000000000000000000, 0.000000000000000000, 0.000000000000000000 ) ) ;
#26662 = VERTEX_POINT ( 'NONE', #3083 ) ;
#26663 = CARTESIAN_POINT ( 'NONE',  ( -17.93324555128263142, -9.020011618190519442, -0.6999999989999727834 ) ) ;
#26664 = CARTESIAN_POINT ( 'NONE',  ( 1.257215589593047023, -4.341675124665348662, -68.10367649352500052 ) ) ;
#26665 = EDGE_LOOP ( 'NONE', ( #12160, #8839, #2933, #23035 ) ) ;
#26666 = CARTESIAN_POINT ( 'NONE',  ( -3.579388909039125988, -3.189794392837340009, -25.77851932450001016 ) ) ;
#26667 = CARTESIAN_POINT ( 'NONE',  ( -6.000000000000000000, -16.12030425626696939, -76.87399601051191667 ) ) ;
#26668 = AXIS2_PLACEMENT_3D ( 'NONE', #7800, #12520, #12988 ) ;
#26669 = CARTESIAN_POINT ( 'NONE',  ( -2.948077164825084306, -3.495793300896363753, -59.17407541852499975 ) ) ;
#26670 = CARTESIAN_POINT ( 'NONE',  ( 8.700000000237631426, -25.41583080867745892, -25.82211739995418753 ) ) ;
#26671 = B_SPLINE_CURVE_WITH_KNOTS ( 'NONE', 3,
 ( #13132, #24946, #10939, #23217 ),
 .UNSPECIFIED., .F., .F.,
 ( 4, 4 ),
 ( 0.000000000000000000, 1.000000000000000000 ),
 .UNSPECIFIED. ) ;
#26672 =( NAMED_UNIT ( * ) PLANE_ANGLE_UNIT ( ) SI_UNIT ( $, .RADIAN. ) );
#26673 = CARTESIAN_POINT ( 'NONE',  ( -4.383426400183576099, -19.28336513850018008, -28.07404357586100829 ) ) ;
#26674 = PRODUCT_DEFINITION_CONTEXT ( 'detailed design', #16418, 'design' ) ;
#26675 = CARTESIAN_POINT ( 'NONE',  ( 8.700000000284820345, -13.66682223737197610, -36.55330428411850363 ) ) ;
#26676 = LINE ( 'NONE', #10004, #19544 ) ;
#26677 = ORIENTED_EDGE ( 'NONE', *, *, #10344, .F. ) ;
#26678 = CARTESIAN_POINT ( 'NONE',  ( 13.11056599509670129, -23.44705117439652042, 36.78285841135431156 ) ) ;
#26679 = EDGE_CURVE ( 'NONE', #23153, #18290, #6570, .T. ) ;
#26680 = CARTESIAN_POINT ( 'NONE',  ( 23.31771987772114940, -13.21065015143701693, 223.9123094306712005 ) ) ;
#26681 = CARTESIAN_POINT ( 'NONE',  ( -24.06750537087731701, -15.26514226597108781, 5.901296963999991263 ) ) ;
#26682 = CARTESIAN_POINT ( 'NONE',  ( 3.043095095529606997, -3.198806979771088077, -95.69213427732501032 ) ) ;
#26683 = CARTESIAN_POINT ( 'NONE',  ( 9.999999999963074870, -25.13744799596687685, -26.04099479820597196 ) ) ;
#26684 = CARTESIAN_POINT ( 'NONE',  ( 10.69999999999999929, -127.2537437101000108, -34.36317024011000143 ) ) ;
#26685 = CARTESIAN_POINT ( 'NONE',  ( -9.897162125297922941, -25.37356426550855204, 141.6604601749999972 ) ) ;
#26686 = CARTESIAN_POINT ( 'NONE',  ( -19.71199437610940919, -20.57358076904808897, -0.6999999999999784173 ) ) ;
#26687 = CARTESIAN_POINT ( 'NONE',  ( -8.999999999970000886, 21.35000000040000145, -60.10000000000000142 ) ) ;
#26688 = CARTESIAN_POINT ( 'NONE',  ( 14.60916111670818474, -28.04296597385482315, 8.000000000000007105 ) ) ;
#26689 = CARTESIAN_POINT ( 'NONE',  ( 23.58655966524121794, -14.71450914371738605, 225.5583129603366785 ) ) ;
#26690 = EDGE_CURVE ( 'NONE', #6097, #8184, #13936, .T. ) ;
#26691 = B_SPLINE_CURVE_WITH_KNOTS ( 'NONE', 5,
 ( #14179, #18732, #16377, #28179, #1761, #1910, #11505, #13709, #16680, #14028, #16531, #4110, #23314, #28333, #11659 ),
 .UNSPECIFIED., .F., .F.,
 ( 6, 3, 3, 3, 6 ),
 ( 0.000000000000000000, 0.1000000000011452422, 0.3999999999988547161, 0.7000000000005726086, 1.000000000000000000 ),
 .UNSPECIFIED. ) ;
#26692 = DIRECTION ( 'NONE',  ( 0.3633921898465273803, -0.9316362575375355393, 0.000000000000000000 ) ) ;
#26693 = LINE ( 'NONE', #5130, #25885 ) ;
#26694 = CYLINDRICAL_SURFACE ( 'NONE', #17308, 10.00000000000001421 ) ;
#26695 = EDGE_LOOP ( 'NONE', ( #6026, #21, #21605, #13212 ) ) ;
#26696 = DIRECTION ( 'NONE',  ( 0.000000000000000000, -0.5000000000001900702, -0.8660254037843290176 ) ) ;
#26697 = FACE_OUTER_BOUND ( 'NONE', #13378, .T. ) ;
#26698 = CARTESIAN_POINT ( 'NONE',  ( 4.332295931058598448, 4.388630459628991787, -57.70805965152499795 ) ) ;
#26699 = ORIENTED_EDGE ( 'NONE', *, *, #20250, .T. ) ;
#26700 = CONTEXT_DEPENDENT_SHAPE_REPRESENTATION ( #30902, #23799 ) ;
#26701 = ORIENTED_EDGE ( 'NONE', *, *, #29880, .F. ) ;
#26702 = DIRECTION ( 'NONE',  ( 0.3633921898465291567, 0.9316362575375349842, 0.000000000000000000 ) ) ;
#26703 = EDGE_LOOP ( 'NONE', ( #5986, #15906, #25180, #1282, #4917, #1751, #20623, #489, #13629, #4774 ) ) ;
#26704 = EDGE_CURVE ( 'NONE', #29499, #18081, #20868, .T. ) ;
#26705 = ORIENTED_EDGE ( 'NONE', *, *, #25901, .F. ) ;
#26706 = LINE ( 'NONE', #14755, #24732 ) ;
#26707 = CARTESIAN_POINT ( 'NONE',  ( -24.43008698341936835, 14.67811372381255630, 4.492876031000014869 ) ) ;
#26708 = CARTESIAN_POINT ( 'NONE',  ( -27.87609112763809449, 3.928995115440388375, 6.600000000000022737 ) ) ;
#26709 = B_SPLINE_SURFACE_WITH_KNOTS ( 'NONE', 5, 5, ( 
 ( #23281, #23448, #4080, #11626, #7057, #21540, #30979, #4545, #13995 ),
 ( #16188, #30675, #11932, #9253, #18861, #4698, #23913, #21224, #15800 ),
 ( #16648, #1878, #26259, #28761, #28618, #30522, #25953, #30825, #9101 ),
 ( #28150, #18701, #23602, #25803, #13836, #4236, #28459, #25650, #20920 ),
 ( #2038, #21078, #11476, #28301, #6894, #6745, #16345, #16496, #2193 ),
 ( #4390, #1723, #26108, #14148, #23753, #11782, #21387, #9411, #19015 ),
 ( #14307, #2348, #13676, #9576, #19174, #7215, #11322, #8949, #18549 ),
 ( #6590, #22005, #26417, #2953, #10043, #26565, #27027, #306, #12238 ),
 ( #7821, #26875, #21855, #4859, #29381, #12086, #15070, #14460, #12547 ) ),
 .UNSPECIFIED., .F., .F., .F.,
 ( 6, 3, 6 ),
 ( 6, 3, 6 ),
 ( 0.000000000000000000, 54.03331039209999886, 92.56095350929999199 ),
 ( 8.011061266649999624, 9.405960541640000727, 10.80085981660000094 ),
 .UNSPECIFIED. ) ;
#26710 = AXIS2_PLACEMENT_3D ( 'NONE', #25174, #3301, #12906 ) ;
#26711 = CARTESIAN_POINT ( 'NONE',  ( -11.69999999949999925, 19.99999999999999645, -1.049999999899998926 ) ) ;
#26712 = CARTESIAN_POINT ( 'NONE',  ( 27.54391550599999761, -3.373045393770000084E-15, 87.04374668499998791 ) ) ;
#26713 = CARTESIAN_POINT ( 'NONE',  ( 0.4590887144193210312, -5.884162454197269909, -8.393384211800002603 ) ) ;
#26714 = DIRECTION ( 'NONE',  ( -3.924189347185962345E-12, 0.4082287037029530552, 0.9128796883888952163 ) ) ;
#26715 = ORIENTED_EDGE ( 'NONE', *, *, #1388, .T. ) ;
#26716 = CARTESIAN_POINT ( 'NONE',  ( 2.541294302003115568, -4.027761424469836093, -44.10000000002499121 ) ) ;
#26717 = CARTESIAN_POINT ( 'NONE',  ( -24.47278419579111386, -14.60601539740217092, 3.904031772999999816 ) ) ;
#26718 = CARTESIAN_POINT ( 'NONE',  ( -2.449727287106972184, -3.823908298404834483, -19.64294088819999828 ) ) ;
#26719 = CARTESIAN_POINT ( 'NONE',  ( 22.97559295454826511, 15.65128684788800939, 8.000000000000007105 ) ) ;
#26720 = CARTESIAN_POINT ( 'NONE',  ( 1.100000000000000089, -17.25771824079999917, 225.0000000000000000 ) ) ;
#26721 = CARTESIAN_POINT ( 'NONE',  ( -4.792542393989999816, 11.13937006400000129, 230.6412452697800006 ) ) ;
#26722 = DIRECTION ( 'NONE',  ( -1.000000000000000000, 0.000000000000000000, -2.257436476311583018E-12 ) ) ;
#26723 = CARTESIAN_POINT ( 'NONE',  ( -19.80535357387461204, 19.50875577042408793, 0.9260390330000090042 ) ) ;
#26724 = EDGE_CURVE ( 'NONE', #9370, #18431, #20273, .T. ) ;
#26725 = CARTESIAN_POINT ( 'NONE',  ( -7.999999999953479879, -114.0541489762801461, 7.119646953328183869 ) ) ;
#26726 = CARTESIAN_POINT ( 'NONE',  ( 0.000000000000000000, 0.000000000000000000, 230.8412452699534470 ) ) ;
#26727 = DIRECTION ( 'NONE',  ( -1.000000000000000000, 0.000000000000000000, -6.771000000000000128E-12 ) ) ;
#26728 = CARTESIAN_POINT ( 'NONE',  ( -24.52721838146529620, 14.51532614515499020, 5.760265123000013254 ) ) ;
#26729 = CYLINDRICAL_SURFACE ( 'NONE', #14270, 3.500000000000000444 ) ;
#26730 = AXIS2_PLACEMENT_3D ( 'NONE', #27482, #2160, #14117 ) ;
#26731 = ORIENTED_EDGE ( 'NONE', *, *, #5484, .T. ) ;
#26732 = CARTESIAN_POINT ( 'NONE',  ( -5.984522419796141079, -1.167122196978044535, -31.09652066320001040 ) ) ;
#26733 = ORIENTED_EDGE ( 'NONE', *, *, #29051, .F. ) ;
#26734 = EDGE_CURVE ( 'NONE', #21489, #19996, #18800, .T. ) ;
#26735 = CARTESIAN_POINT ( 'NONE',  ( 24.50348397774211051, -13.13223627713423092, 3.957489296000010981 ) ) ;
#26736 = CARTESIAN_POINT ( 'NONE',  ( -5.221537131022022216, 0.5214849208526588509, -48.37737393802499497 ) ) ;
#26737 = VERTEX_POINT ( 'NONE', #15660 ) ;
#26738 = ORIENTED_EDGE ( 'NONE', *, *, #22969, .T. ) ;
#26739 = EDGE_CURVE ( 'NONE', #16404, #4771, #27822, .T. ) ;
#26740 = B_SPLINE_CURVE_WITH_KNOTS ( 'NONE', 5,
 ( #11778, #30672, #16645, #18698, #26255, #10683, #29878, #27668, #22802 ),
 .UNSPECIFIED., .F., .F.,
 ( 6, 3, 6 ),
 ( 8.011061266649999624, 8.831591450809998634, 9.652121634960000307 ),
 .UNSPECIFIED. ) ;
#26741 = APPLICATION_PROTOCOL_DEFINITION ( 'draft international standard', 'automotive_design', 1998, #544 ) ;
#26742 = B_SPLINE_CURVE_WITH_KNOTS ( 'NONE', 5,
 ( #180, #2229, #2534, #24095, #21582, #16846, #12121, #26451, #4429, #18899, #29, #2072 ),
 .UNSPECIFIED., .F., .F.,
 ( 6, 3, 3, 6 ),
 ( 0.000000000000000000, 2.408321940520000037, 4.816680738749999691, 4.935551033660000364 ),
 .UNSPECIFIED. ) ;
#26743 = ORIENTED_EDGE ( 'NONE', *, *, #17377, .T. ) ;
#26744 = CARTESIAN_POINT ( 'NONE',  ( -0.2462327729630000017, -28.49941772390000239, 223.9202095490000204 ) ) ;
#26745 = ORIENTED_EDGE ( 'NONE', *, *, #633, .F. ) ;
#26746 = DIRECTION ( 'NONE',  ( 1.224606353819999829E-16, 1.000000000000000000, 0.000000000000000000 ) ) ;
#26747 = CARTESIAN_POINT ( 'NONE',  ( 2.992535305844774118, 1.816776806827645085, 227.6446713698604185 ) ) ;
#26748 = FACE_OUTER_BOUND ( 'NONE', #22869, .T. ) ;
#26749 = CARTESIAN_POINT ( 'NONE',  ( 0.5919590525021038996, 4.200897578713889580, -35.69999999999999574 ) ) ;
#26750 = EDGE_CURVE ( 'NONE', #22118, #9001, #18152, .T. ) ;
#26751 = LINE ( 'NONE', #7852, #7047 ) ;
#26752 = CARTESIAN_POINT ( 'NONE',  ( -23.77307140041805411, 14.41181874028064591, 5.104215870000011535 ) ) ;
#26753 = DIRECTION ( 'NONE',  ( 0.000000000000000000, 0.000000000000000000, 1.000000000000000000 ) ) ;
#26754 = VECTOR ( 'NONE', #17315, 1000.000000000000000 ) ;
#26755 = DIRECTION ( 'NONE',  ( 0.000000000000000000, -0.9396926207858125046, -0.3420201433259318358 ) ) ;
#26756 = VERTEX_POINT ( 'NONE', #6686 ) ;
#26757 = CARTESIAN_POINT ( 'NONE',  ( -1.831588579526983063, 3.958388136463033558, -8.231725184300008991 ) ) ;
#26758 = CARTESIAN_POINT ( 'NONE',  ( 2.450607853129171954, -3.579122932049592976, -26.63292313650000764 ) ) ;
#26759 = CARTESIAN_POINT ( 'NONE',  ( 2.787054272977523173, -3.222358495660834876, -70.05117212551519401 ) ) ;
#26760 = ADVANCED_FACE ( 'NONE', ( #16288 ), #8733, .F. ) ;
#26761 = LINE ( 'NONE', #9776, #26754 ) ;
#26762 = CARTESIAN_POINT ( 'NONE',  ( 24.86822223037987456, 13.92223202030449691, 5.680679506000013923 ) ) ;
#26763 = SURFACE_STYLE_FILL_AREA ( #7412 ) ;
#26764 = CARTESIAN_POINT ( 'NONE',  ( 1.656896971990419853, -20.50178133589399110, -27.47978228995554417 ) ) ;
#26765 = CARTESIAN_POINT ( 'NONE',  ( -4.484282906631567478, 1.269983465873030015, -7.310827254900003069 ) ) ;
#26766 = DIRECTION ( 'NONE',  ( -5.551115123047629543E-18, 6.252214723449840749E-31, -1.000000000000000000 ) ) ;
#26767 = CARTESIAN_POINT ( 'NONE',  ( -24.75645986059852177, -14.12045945554185522, 4.098702617000016701 ) ) ;
#26768 = EDGE_LOOP ( 'NONE', ( #4116, #5151, #26596, #16888, #1920 ) ) ;
#26769 = EDGE_CURVE ( 'NONE', #4259, #10529, #23809, .T. ) ;
#26770 = CARTESIAN_POINT ( 'NONE',  ( -16.83342759579999637, 11.00000000000000355, -0.8000000000000020428 ) ) ;
#26771 = CARTESIAN_POINT ( 'NONE',  ( -12.42716818975153892, -32.00000000000000711, -29.85990057496828953 ) ) ;
#26772 = ORIENTED_EDGE ( 'NONE', *, *, #9018, .F. ) ;
#26773 = CARTESIAN_POINT ( 'NONE',  ( -7.999999999699952014, -24.42167197178301308, -29.98317312624888231 ) ) ;
#26774 = DIRECTION ( 'NONE',  ( -0.8660254037843290176, 0.5000000000001899592, 0.000000000000000000 ) ) ;
#26776 = EDGE_LOOP ( 'NONE', ( #2857, #4801, #127, #5524 ) ) ;
#26775 = VECTOR ( 'NONE', #13683, 1000.000000000000000 ) ;
#26777 = CARTESIAN_POINT ( 'NONE',  ( -4.647753910737981720, 0.7988342186384705945, -44.10000000002498410 ) ) ;
#26778 = EDGE_LOOP ( 'NONE', ( #5081, #10482, #160, #24479 ) ) ;
#26779 = B_SPLINE_SURFACE_WITH_KNOTS ( 'NONE', 5, 1, ( 
 ( #29357, #10174 ),
 ( #12844, #29820 ),
 ( #12677, #29515 ),
 ( #8408, #7802 ),
 ( #15356, #17399 ),
 ( #27005, #19775 ),
 ( #24954, #19927 ),
 ( #20082, #5443 ),
 ( #13139, #17694 ),
 ( #27312, #10789 ),
 ( #7950, #3386 ),
 ( #5751, #12990 ),
 ( #22287, #15053 ),
 ( #8257, #15196 ),
 ( #24647, #22602 ) ),
 .UNSPECIFIED., .F., .F., .F.,
 ( 6, 3, 3, 3, 6 ),
 ( 2, 2 ),
 ( 0.000000000000000000, 0.5239017170190000128, 1.047803434039999981, 1.571705151059999972, 1.746339056730000117 ),
 ( -0.7000000000009999335, 2.556331278550000249E-06 ),
 .UNSPECIFIED. ) ;
#26780 = ORIENTED_EDGE ( 'NONE', *, *, #26192, .T. ) ;
#26781 = FILL_AREA_STYLE ('',( #29137 ) ) ;
#26782 = ORIENTED_EDGE ( 'NONE', *, *, #13819, .F. ) ;
#26783 = CARTESIAN_POINT ( 'NONE',  ( -17.49999999932747130, -30.00000000000000000, -28.40000000020000215 ) ) ;
#26784 = CARTESIAN_POINT ( 'NONE',  ( 8.700000000248671483, -25.22378963206060831, -30.84934466687800025 ) ) ;
#26785 = DIRECTION ( 'NONE',  ( 1.667044707805962905E-12, -0.4082287037029530552, -0.9128796883888953273 ) ) ;
#26786 = ORIENTED_EDGE ( 'NONE', *, *, #3309, .T. ) ;
#26787 = CARTESIAN_POINT ( 'NONE',  ( -24.83272648880584654, 12.49791454310039640, 5.208434320000010942 ) ) ;
#26788 = CARTESIAN_POINT ( 'NONE',  ( -28.68577476999353237, 9.950727454195712696, 1.000000000000000888 ) ) ;
#26789 = CARTESIAN_POINT ( 'NONE',  ( -13.39900052755271886, 20.99999999990061994, -68.94364015901247456 ) ) ;
#26790 = CARTESIAN_POINT ( 'NONE',  ( 10.69999999994264428, -27.47147066701633022, -16.98898364808261618 ) ) ;
#26791 = VERTEX_POINT ( 'NONE', #30140 ) ;
#26792 = TOROIDAL_SURFACE ( 'NONE', #30326, 24.50000000000000000, 4.000000000000000000 ) ;
#26793 = LINE ( 'NONE', #22084, #7416 ) ;
#26794 = CARTESIAN_POINT ( 'NONE',  ( 2.992916622598570608, -2.824380467281231599, -17.53565261000000319 ) ) ;
#26795 = CARTESIAN_POINT ( 'NONE',  ( -27.79999999970000246, -10.21376199200000201, 229.0000000000000000 ) ) ;
#26796 = EDGE_CURVE ( 'NONE', #12383, #11948, #21817, .T. ) ;
#26797 = CARTESIAN_POINT ( 'NONE',  ( -27.50000000000000000, 0.000000000000000000, 143.6055512749999821 ) ) ;
#26798 = AXIS2_PLACEMENT_3D ( 'NONE', #29704, #12873, #3419 ) ;
#26799 = DIRECTION ( 'NONE',  ( 0.000000000000000000, -2.256504834499999987E-12, -1.000000000000000000 ) ) ;
#26800 = CARTESIAN_POINT ( 'NONE',  ( 0.5184513693225187847, -28.49550581263314086, 3.899998581000013509 ) ) ;
#26801 = LINE ( 'NONE', #5245, #30375 ) ;
#26802 = EDGE_CURVE ( 'NONE', #28608, #16174, #23073, .T. ) ;
#26803 = CARTESIAN_POINT ( 'NONE',  ( 17.16657240420000008, 10.97998838177520931, -1.452769935612311825 ) ) ;
#26804 = EDGE_CURVE ( 'NONE', #5832, #14789, #19284, .T. ) ;
#26805 = FACE_OUTER_BOUND ( 'NONE', #30063, .T. ) ;
#26806 = CARTESIAN_POINT ( 'NONE',  ( 27.24857305720000156, 4.601362004630000335, 229.9172022069999741 ) ) ;
#26807 = CARTESIAN_POINT ( 'NONE',  ( -3.184804871879999943, 18.07879523729999960, 230.6999999999999886 ) ) ;
#26808 = ORIENTED_EDGE ( 'NONE', *, *, #11030, .T. ) ;
#26809 = CARTESIAN_POINT ( 'NONE',  ( -4.292339292658051697, -2.347882601813513492, -52.59982952342499374 ) ) ;
#26810 = DIRECTION ( 'NONE',  ( 1.386461269282634800E-13, 1.000000000000000000, 0.000000000000000000 ) ) ;
#26811 = CARTESIAN_POINT ( 'NONE',  ( -26.40151772468378510, 8.923123374263472130, 0.08279779700001710374 ) ) ;
#26812 = CARTESIAN_POINT ( 'NONE',  ( -4.059731841906703664, -0.4201311362673507133, -68.10000000002501963 ) ) ;
#26813 = AXIS2_PLACEMENT_3D ( 'NONE', #18529, #13815, #6568 ) ;
#26814 = ORIENTED_EDGE ( 'NONE', *, *, #24532, .F. ) ;
#26815 = TOROIDAL_SURFACE ( 'NONE', #21297, 12.03781779390000040, 6.000000000000000000 ) ;
#26816 = CARTESIAN_POINT ( 'NONE',  ( 1.532951308181600414, -0.6901018627532701233, -97.93793859254537892 ) ) ;
#26817 = AXIS2_PLACEMENT_3D ( 'NONE', #13304, #22914, #4178 ) ;
#26818 = EDGE_LOOP ( 'NONE', ( #29538, #10110, #12850, #7582 ) ) ;
#26819 = DIRECTION ( 'NONE',  ( 1.000000000000000000, 0.000000000000000000, 0.000000000000000000 ) ) ;
#26820 = DIRECTION ( 'NONE',  ( 1.000000000000000000, 0.000000000000000000, 0.000000000000000000 ) ) ;
#26821 = ORIENTED_EDGE ( 'NONE', *, *, #29581, .F. ) ;
#26822 = CARTESIAN_POINT ( 'NONE',  ( -0.5718866478877175918, 5.491608289559616551, -26.88903409329999761 ) ) ;
#26823 = CARTESIAN_POINT ( 'NONE',  ( 8.000000000000000000, -15.18061163548115466, -76.53197586718597734 ) ) ;
#26824 = CARTESIAN_POINT ( 'NONE',  ( 2.097865490181829884, -3.779070126327673140, -55.58172062782499268 ) ) ;
#26825 = CARTESIAN_POINT ( 'NONE',  ( 8.000000000749292184, -24.01208138067712028, -28.87597782833235627 ) ) ;
#26826 = CARTESIAN_POINT ( 'NONE',  ( -3.982632971385688947, -19.71206033698065596, -27.86495495700036784 ) ) ;
#26827 = B_SPLINE_CURVE_WITH_KNOTS ( 'NONE', 5,
 ( #15910, #11503, #3955, #16375, #9129, #8661 ),
 .UNSPECIFIED., .F., .F.,
 ( 6, 6 ),
 ( 76.96280491019999204, 81.23072221990000230 ),
 .UNSPECIFIED. ) ;
#26828 = CARTESIAN_POINT ( 'NONE',  ( 8.700000000296723712, -12.54225101349288529, -39.16323275742981025 ) ) ;
#26829 = AXIS2_PLACEMENT_3D ( 'NONE', #15043, #1304, #27721 ) ;
#26830 = CARTESIAN_POINT ( 'NONE',  ( -17.45884911674703588, -22.00029789592859686, -29.17883862680921681 ) ) ;
#26831 = VERTEX_POINT ( 'NONE', #2134 ) ;
#26832 = CARTESIAN_POINT ( 'NONE',  ( 14.71164558017381019, -31.99968858407690320, -26.83887133594891239 ) ) ;
#26833 = CARTESIAN_POINT ( 'NONE',  ( 11.69999999989999928, -24.11120071670000087, -1.399999999299995856 ) ) ;
#26834 = AXIS2_PLACEMENT_3D ( 'NONE', #23254, #6409, #21199 ) ;
#26835 = AXIS2_PLACEMENT_3D ( 'NONE', #30885, #9315, #16552 ) ;
#26836 = CARTESIAN_POINT ( 'NONE',  ( -11.18209233740000208, 4.537649734730000439, 231.9999989789999972 ) ) ;
#26837 = CARTESIAN_POINT ( 'NONE',  ( 2.015353881180397710, -1.035356480594303852, -97.67120874164949385 ) ) ;
#26838 = CARTESIAN_POINT ( 'NONE',  ( -23.96357375497718678, -14.09276578719063266, 3.927141029190090560 ) ) ;
#26839 = AXIS2_PLACEMENT_3D ( 'NONE', #27927, #6368, #15965 ) ;
#26840 = CARTESIAN_POINT ( 'NONE',  ( -11.69999999989999928, -24.11120071630000083, -1.399999999999998579 ) ) ;
#26841 = CARTESIAN_POINT ( 'NONE',  ( 3.048238659810818429, -2.820297993983834406, -0.6999999999999991784 ) ) ;
#26842 = CARTESIAN_POINT ( 'NONE',  ( 23.94939220324485518, -20.40613828787117967, 0.2374258030000131470 ) ) ;
#26844 = ADVANCED_FACE ( 'NONE', ( #24301, #26509 ), #4640, .F. ) ;
#26843 = CARTESIAN_POINT ( 'NONE',  ( -1.033595436889999888E-13, -27.50000000069999828, 3.899999999999999911 ) ) ;
#26845 = CARTESIAN_POINT ( 'NONE',  ( 0.000000000000000000, 0.000000000000000000, 229.6412452697800006 ) ) ;
#26846 = DIRECTION ( 'NONE',  ( -1.000000000000000000, 0.000000000000000000, 0.000000000000000000 ) ) ;
#26847 = B_SPLINE_CURVE_WITH_KNOTS ( 'NONE', 5,
 ( #22459, #909, #17567, #15518, #15212, #27174, #12692, #13154, #29688, #10647, #30153, #22927, #22761, #6238, #8114 ),
 .UNSPECIFIED., .F., .F.,
 ( 6, 3, 3, 3, 6 ),
 ( 0.000000000000000000, 0.1000000000000000472, 0.3999999999942737139, 0.6999999999994274136, 1.000000000000000000 ),
 .UNSPECIFIED. ) ;
#26849 = CYLINDRICAL_SURFACE ( 'NONE', #3717, 20.00000000000000355 ) ;
#26848 = APPLICATION_CONTEXT ( 'automotive_design' ) ;
#26850 = CARTESIAN_POINT ( 'NONE',  ( 0.000000000000000000, 0.000000000000000000, 143.6055512739999926 ) ) ;
#26851 = ORIENTED_EDGE ( 'NONE', *, *, #30416, .T. ) ;
#26852 = CARTESIAN_POINT ( 'NONE',  ( -17.47315945020447359, -25.05913013249180565, -23.74705904876886109 ) ) ;
#26853 = CARTESIAN_POINT ( 'NONE',  ( 19.80526555972147307, 19.50877392102524155, 2.600000000000019185 ) ) ;
#26854 =( LENGTH_UNIT ( ) NAMED_UNIT ( * ) SI_UNIT ( .MILLI., .METRE. ) );
#26855 = CARTESIAN_POINT ( 'NONE',  ( 25.22036945370000183, -13.27344566769999901, 225.2083619149999834 ) ) ;
#26856 = B_SPLINE_CURVE_WITH_KNOTS ( 'NONE', 5,
 ( #7577, #23300, #25667, #20618, #20777, #27856, #22828, #27692, #4097, #13696, #15580, #6607, #25349, #15901, #1746 ),
 .UNSPECIFIED., .F., .F.,
 ( 6, 3, 3, 3, 6 ),
 ( 7.679355244459999952, 8.437083003899999767, 11.24945694400000029, 14.06183523920000056, 15.35825106630000114 ),
 .UNSPECIFIED. ) ;
#26857 = AXIS2_PLACEMENT_3D ( 'NONE', #10902, #29630, #849 ) ;
#26858 = CARTESIAN_POINT ( 'NONE',  ( -5.035266659556940638, -1.323295706752037670, -57.25102360502499721 ) ) ;
#26859 = CIRCLE ( 'NONE', #9263, 4.175165894169885483 ) ;
#26860 = ORIENTED_EDGE ( 'NONE', *, *, #14527, .T. ) ;
#26861 = VECTOR ( 'NONE', #30091, 1000.000000000000000 ) ;
#26862 = ITEM_DEFINED_TRANSFORMATION ( 'NONE', 'NONE', #10815,  #17722 ) ;
#26863 = CIRCLE ( 'NONE', #10221, 3.000000000000001332 ) ;
#26864 = ORIENTED_EDGE ( 'NONE', *, *, #10530, .F. ) ;
#26865 = CARTESIAN_POINT ( 'NONE',  ( 8.700000000235451836, -26.13547327700162271, -25.50030203292368114 ) ) ;
#26866 = VERTEX_POINT ( 'NONE', #2592 ) ;
#26867 = EDGE_CURVE ( 'NONE', #11998, #6070, #2014, .T. ) ;
#26868 = CARTESIAN_POINT ( 'NONE',  ( -24.09407738750993033, 13.86899051154378881, 3.997190861000005313 ) ) ;
#26869 = CARTESIAN_POINT ( 'NONE',  ( -25.21256988278790701, -13.28918881462575285, 224.7093197384999428 ) ) ;
#26870 = CARTESIAN_POINT ( 'NONE',  ( 17.42753860032010849, 12.07825306288010658, -1.400000000000001910 ) ) ;
#26871 = CARTESIAN_POINT ( 'NONE',  ( 8.700000000274457079, -18.36552062635309213, -34.81248186671538036 ) ) ;
#26872 = CARTESIAN_POINT ( 'NONE',  ( 4.689100480956518879, -0.8300439969826994835, -7.833982634700003445 ) ) ;
#26873 = VECTOR ( 'NONE', #5239, 1000.000000000000000 ) ;
#26874 =( GEOMETRIC_REPRESENTATION_CONTEXT ( 3 ) GLOBAL_UNCERTAINTY_ASSIGNED_CONTEXT ( ( #14418 ) ) GLOBAL_UNIT_ASSIGNED_CONTEXT ( ( #17974, #27587, #13265 ) ) REPRESENTATION_CONTEXT ( 'NONE', 'WORKASPACE' ) );
#26875 = CARTESIAN_POINT ( 'NONE',  ( 27.04041630560000087, -5.329070518199999767E-14, 230.6999999999999886 ) ) ;
#26876 = EDGE_LOOP ( 'NONE', ( #6788, #28254, #7999, #19693 ) ) ;
#26877 = CARTESIAN_POINT ( 'NONE',  ( 0.4822354468651134929, -3.969360884996547156, -44.10000000002497700 ) ) ;
#26878 = CARTESIAN_POINT ( 'NONE',  ( 24.97472003062369694, 13.73006752330286595, 4.791638082000004850 ) ) ;
#26879 = CARTESIAN_POINT ( 'NONE',  ( 0.5300456733980246637, -4.293941145674104121, -18.37054674910000429 ) ) ;
#26880 = CARTESIAN_POINT ( 'NONE',  ( -12.41081696005857715, -25.67136812075533925, -33.40618142470727747 ) ) ;
#26881 = FACE_OUTER_BOUND ( 'NONE', #14448, .T. ) ;
#26882 = VECTOR ( 'NONE', #775, 1000.000000000000000 ) ;
#26883 = CARTESIAN_POINT ( 'NONE',  ( 0.000000000000000000, 0.000000000000000000, 229.1412452697749984 ) ) ;
#26884 = AXIS2_PLACEMENT_3D ( 'NONE', #14708, #16591, #21787 ) ;
#26885 = CARTESIAN_POINT ( 'NONE',  ( 0.8233563490081640124, -27.78802870620434007, 224.2672522965996791 ) ) ;
#26886 = CARTESIAN_POINT ( 'NONE',  ( -5.162912894389027230, 3.035924517800103750, -44.36354844312499779 ) ) ;
#26887 = CARTESIAN_POINT ( 'NONE',  ( -7.999999999961045383, -115.3392401410248738, 8.473717002696254497 ) ) ;
#26888 = CARTESIAN_POINT ( 'NONE',  ( -27.23548387060000309, 7.105427357599999217E-15, 141.6604601749999972 ) ) ;
#26889 = CARTESIAN_POINT ( 'NONE',  ( -10.69999999999813589, -27.37998968024088953, -25.40000000000000213 ) ) ;
#26890 = CARTESIAN_POINT ( 'NONE',  ( -26.81201737230000148, 9.375055877159999440, 229.0000000000000000 ) ) ;
#26891 = CARTESIAN_POINT ( 'NONE',  ( 9.000000000000000000, 21.70000000000000284, -51.10000000017000588 ) ) ;
#26893 = ORIENTED_EDGE ( 'NONE', *, *, #29617, .F. ) ;
#26892 = VECTOR ( 'NONE', #13390, 1000.000000000000000 ) ;
#26894 = CARTESIAN_POINT ( 'NONE',  ( -2.308365619037855421, -4.044857084274065429, -30.67642233980000199 ) ) ;
#26895 = CIRCLE ( 'NONE', #16852, 3.199999983039998774 ) ;
#26896 =( GEOMETRIC_REPRESENTATION_CONTEXT ( 3 ) GLOBAL_UNCERTAINTY_ASSIGNED_CONTEXT ( ( #26987 ) ) GLOBAL_UNIT_ASSIGNED_CONTEXT ( ( #18418, #20467, #13863 ) ) REPRESENTATION_CONTEXT ( 'NONE', 'WORKASPACE' ) );
#26897 = ORIENTED_EDGE ( 'NONE', *, *, #14555, .F. ) ;
#26898 = CARTESIAN_POINT ( 'NONE',  ( -10.00000000020261659, -34.37899275726326920, -24.26894200080224095 ) ) ;
#26899 = CARTESIAN_POINT ( 'NONE',  ( -4.848570193085772750, 0.4842359979205512754, -48.02737393802500065 ) ) ;
#26900 = VERTEX_POINT ( 'NONE', #23698 ) ;
#26901 = ORIENTED_EDGE ( 'NONE', *, *, #9395, .T. ) ;
#26902 = ADVANCED_FACE ( 'NONE', ( #19428 ), #26204, .T. ) ;
#26903 = APPLICATION_PROTOCOL_DEFINITION ( 'draft international standard', 'automotive_design', 1998, #29463 ) ;
#26904 = ORIENTED_EDGE ( 'NONE', *, *, #14650, .F. ) ;
#26905 = DIRECTION ( 'NONE',  ( 0.000000000000000000, 0.000000000000000000, 1.000000000000000000 ) ) ;
#26906 = ORIENTED_EDGE ( 'NONE', *, *, #13583, .F. ) ;
#26907 = CARTESIAN_POINT ( 'NONE',  ( 8.000000000846746673, -13.86721103371404418, -37.00141305325693963 ) ) ;
#26908 = CARTESIAN_POINT ( 'NONE',  ( -9.993285220779425160, -25.61999708228226069, 115.0000000000000000 ) ) ;
#26909 = EDGE_CURVE ( 'NONE', #29211, #5951, #5203, .T. ) ;
#26910 = CARTESIAN_POINT ( 'NONE',  ( 23.80322556508107112, 14.59355840047072661, 8.000000000000007105 ) ) ;
#26911 = FACE_OUTER_BOUND ( 'NONE', #31063, .T. ) ;
#26912 = DIRECTION ( 'NONE',  ( 0.000000000000000000, 0.000000000000000000, -1.000000000000000000 ) ) ;
#26913 = CARTESIAN_POINT ( 'NONE',  ( -23.79228473957821777, 14.38012949749760416, 5.310643621000004977 ) ) ;
#26914 = CARTESIAN_POINT ( 'NONE',  ( 2.816286225276055433, -4.345042730952153320, 0.8340606117000020081 ) ) ;
#26915 = CARTESIAN_POINT ( 'NONE',  ( -23.52253596342320918, -14.81732487615617089, 224.7105397188568645 ) ) ;
#26916 = ORIENTED_EDGE ( 'NONE', *, *, #6593, .F. ) ;
#26917 = CARTESIAN_POINT ( 'NONE',  ( 4.584724779240096915, 3.684399570836669024, -9.354586408000001185 ) ) ;
#26918 = CARTESIAN_POINT ( 'NONE',  ( 6.487627055914963137, 0.6495842397260740420, -29.63116556699998938 ) ) ;
#26919 = CARTESIAN_POINT ( 'NONE',  ( 3.629192601380414551, -1.807102915225842432, -69.53606122035726855 ) ) ;
#26920 = PRODUCT_DEFINITION_FORMATION_WITH_SPECIFIED_SOURCE ( 'ANY', '', #25418, .NOT_KNOWN. ) ;
#26921 = CARTESIAN_POINT ( 'NONE',  ( 24.14205449336675713, -13.78537897189897343, 6.042507811999997536 ) ) ;
#26922 = EDGE_CURVE ( 'NONE', #7809, #25385, #5100, .T. ) ;
#26923 = CARTESIAN_POINT ( 'NONE',  ( 19.80526555982327608, 19.50877392092707296, 0.9260799790000162623 ) ) ;
#26924 = FILL_AREA_STYLE_COLOUR ( '', #5102 ) ;
#26925 = CARTESIAN_POINT ( 'NONE',  ( 1.638687372170419598, -20.50181238077955470, -27.47976714835314738 ) ) ;
#26926 = CARTESIAN_POINT ( 'NONE',  ( -8.699999999726605537, -29.57832802798597527, -26.81682687338189197 ) ) ;
#26927 = EDGE_CURVE ( 'NONE', #1750, #22335, #23425, .T. ) ;
#26928 = B_SPLINE_CURVE_WITH_KNOTS ( 'NONE', 3,
 ( #22517, #24875, #29897, #8638, #23141, #15723, #8323, #3304, #22818, #3937, #30377, #11019 ),
 .UNSPECIFIED., .F., .F.,
 ( 4, 2, 2, 2, 2, 4 ),
 ( 0.000000000000000000, 0.2499999999999976685, 0.3749999999999970579, 0.4999999999999964473, 0.7499999999999982236, 1.000000000000000000 ),
 .UNSPECIFIED. ) ;
#26929 = CARTESIAN_POINT ( 'NONE',  ( 10.69999999999999929, -43.95328087560000085, -27.24755286599999948 ) ) ;
#26930 = CARTESIAN_POINT ( 'NONE',  ( -24.98081131316241255, -13.71897606304888662, 4.999998581000003384 ) ) ;
#26931 = CARTESIAN_POINT ( 'NONE',  ( -1.291648043245374966, -3.499742528933395658, 230.7036791710427508 ) ) ;
#26932 = ORIENTED_EDGE ( 'NONE', *, *, #11187, .F. ) ;
#26933 = PRODUCT_DEFINITION ( 'UNKNOWN', '', #9328, #263 ) ;
#26934 = CARTESIAN_POINT ( 'NONE',  ( 8.000000000488469709, -24.55065533249607412, -26.62378963273996391 ) ) ;
#26935 = CARTESIAN_POINT ( 'NONE',  ( -1.861312627829580402, -20.50181238076562096, -27.47976714835994727 ) ) ;
#26936 = ORIENTED_EDGE ( 'NONE', *, *, #16820, .T. ) ;
#26937 = DIRECTION ( 'NONE',  ( 0.000000000000000000, -2.257145581549999994E-12, -1.000000000000000000 ) ) ;
#26938 = CARTESIAN_POINT ( 'NONE',  ( -8.699999999691694796, -25.92947359974585098, -31.20249410827203107 ) ) ;
#26939 = ORIENTED_EDGE ( 'NONE', *, *, #23388, .F. ) ;
#26940 = CARTESIAN_POINT ( 'NONE',  ( -4.328334940905476991, -2.689252967667119520, -44.10000000002499121 ) ) ;
#26941 = ORIENTED_EDGE ( 'NONE', *, *, #28269, .F. ) ;
#26942 = EDGE_LOOP ( 'NONE', ( #21713, #1157, #21372, #21348, #2674 ) ) ;
#26943 = ORIENTED_EDGE ( 'NONE', *, *, #9375, .F. ) ;
#26944 = CARTESIAN_POINT ( 'NONE',  ( 28.35924375240000117, 4.788916714149999088, 229.7625741969999922 ) ) ;
#26945 = EDGE_CURVE ( 'NONE', #27983, #24427, #13236, .T. ) ;
#26946 = DIRECTION ( 'NONE',  ( 0.000000000000000000, 1.000000000000000000, 0.000000000000000000 ) ) ;
#26947 = CARTESIAN_POINT ( 'NONE',  ( -8.000000000050450311, -115.5267901941129907, 21.04701626955636939 ) ) ;
#26948 = ORIENTED_EDGE ( 'NONE', *, *, #5279, .F. ) ;
#26949 = DIRECTION ( 'NONE',  ( 1.000000000000000000, 0.000000000000000000, 0.000000000000000000 ) ) ;
#26950 = CARTESIAN_POINT ( 'NONE',  ( -24.06826084723317649, 20.50742046750733039, 1.000000000000000888 ) ) ;
#26951 = CARTESIAN_POINT ( 'NONE',  ( -17.41896590622109287, -31.99977565255875689, -27.25864250883248374 ) ) ;
#26952 = ADVANCED_FACE ( 'NONE', ( #21327 ), #2696, .F. ) ;
#26953 = LINE ( 'NONE', #31096, #15430 ) ;
#26954 = CARTESIAN_POINT ( 'NONE',  ( -4.047971700351067348, -2.476765951022760870, -20.97049200639999356 ) ) ;
#26955 = CARTESIAN_POINT ( 'NONE',  ( -17.91041691994261242, -8.732827808381141921, -0.6999999999999784173 ) ) ;
#26956 = CARTESIAN_POINT ( 'NONE',  ( 10.69999999999999929, -24.92624922430000467, -26.23177045490000125 ) ) ;
#26957 = CARTESIAN_POINT ( 'NONE',  ( -12.40426553250898500, -28.36724026820617794, -33.38411139160245256 ) ) ;
#26958 = EDGE_CURVE ( 'NONE', #23024, #22582, #21300, .T. ) ;
#26959 = CARTESIAN_POINT ( 'NONE',  ( 28.23994777610000284, 4.869985548859999902, 222.0000000000000000 ) ) ;
#26960 = CARTESIAN_POINT ( 'NONE',  ( 10.34999999979999963, 19.99999999999999645, -2.400000000399998612 ) ) ;
#26961 = CARTESIAN_POINT ( 'NONE',  ( 26.80000000069999899, -3.281945028320000125E-15, 192.8898184869999852 ) ) ;
#26962 = EDGE_CURVE ( 'NONE', #29126, #19505, #3899, .T. ) ;
#26963 = CARTESIAN_POINT ( 'NONE',  ( 17.93345776099999966, 20.10553696510000066, 230.0000000000000000 ) ) ;
#26964 = CARTESIAN_POINT ( 'NONE',  ( -2.595987296770100095, -16.63200279373747392, -109.8342699011499946 ) ) ;
#26965 = ORIENTED_EDGE ( 'NONE', *, *, #19134, .F. ) ;
#26966 = CARTESIAN_POINT ( 'NONE',  ( 3.630871288588910506, -4.685987307826644965, -52.02430438132500257 ) ) ;
#26967 = CARTESIAN_POINT ( 'NONE',  ( -8.699999999675917195, -17.42919676355489855, -33.49161196806937824 ) ) ;
#26968 = B_SPLINE_CURVE_WITH_KNOTS ( 'NONE', 3,
 ( #22383, #15441, #3321, #17936, #980, #27094 ),
 .UNSPECIFIED., .F., .F.,
 ( 4, 2, 4 ),
 ( 0.000000000000000000, 0.5000000000000000000, 1.000000000000000000 ),
 .UNSPECIFIED. ) ;
#26969 = CARTESIAN_POINT ( 'NONE',  ( -26.85558069653561120, 9.076679569434611849, 0.5514269540000116265 ) ) ;
#26970 = CARTESIAN_POINT ( 'NONE',  ( -4.660805219281239253, 0.7680161694985663257, -68.10000000002503384 ) ) ;
#26971 = EDGE_LOOP ( 'NONE', ( #17189, #26515, #2522, #28208, #21413, #18251, #1286, #3392, #30852, #7483, #31116, #2026, #24686, #7470, #4916, #11809, #26814 ) ) ;
#26972 = CARTESIAN_POINT ( 'NONE',  ( -3.646602756718712701, -1.367734702628457866, -96.46963879144223597 ) ) ;
#26973 = EDGE_LOOP ( 'NONE', ( #6461, #30392, #18155, #2329 ) ) ;
#26974 = CARTESIAN_POINT ( 'NONE',  ( -249983.7073439999076, -207625.5457919999608, -380034.9891179999686 ) ) ;
#26975 = ADVANCED_FACE ( 'NONE', ( #29642 ), #19162, .T. ) ;
#26976 = CARTESIAN_POINT ( 'NONE',  ( 23.47637528925218575, 14.89020703997133488, 5.901296968999991677 ) ) ;
#26977 = VERTEX_POINT ( 'NONE', #25715 ) ;
#26978 = CARTESIAN_POINT ( 'NONE',  ( 2.450607853129164848, -3.579122932049590755, -27.13292313650000764 ) ) ;
#26979 = CARTESIAN_POINT ( 'NONE',  ( -10.14902473063359167, -26.01926976387843027, 192.0603150150000147 ) ) ;
#26980 = ADVANCED_FACE ( 'NONE', ( #28637 ), #18137, .F. ) ;
#26981 = CARTESIAN_POINT ( 'NONE',  ( -21.46610162199371885, 17.08729007858795157, -0.6999999999999784173 ) ) ;
#26982 = DIRECTION ( 'NONE',  ( 0.000000000000000000, 0.000000000000000000, -1.000000000000000000 ) ) ;
#26983 = SURFACE_SIDE_STYLE ('',( #20059 ) ) ;
#26984 = ADVANCED_FACE ( 'NONE', ( #3990 ), #8730, .T. ) ;
#26985 = CARTESIAN_POINT ( 'NONE',  ( 23.20948082139999968, -13.40000000000000036, 226.0999999999999943 ) ) ;
#26986 = VERTEX_POINT ( 'NONE', #8376 ) ;
#26987 = UNCERTAINTY_MEASURE_WITH_UNIT (LENGTH_MEASURE( 1.000000000000000082E-05 ), #18418, 'distance_accuracy_value', 'NONE');
#26988 = CARTESIAN_POINT ( 'NONE',  ( 24.70074545465923421, -14.21822122957792445, 3.997190862000010725 ) ) ;
#26989 = CARTESIAN_POINT ( 'NONE',  ( 7.908773014210000341, 16.35323874420000223, 230.6999999999999886 ) ) ;
#26990 = EDGE_LOOP ( 'NONE', ( #15512, #16587, #26705, #28368 ) ) ;
#26991 = CARTESIAN_POINT ( 'NONE',  ( 14.67158610510948513, -31.99958078956481700, -30.24423881306254813 ) ) ;
#26992 = CARTESIAN_POINT ( 'NONE',  ( 10.99999999979999998, 20.99999999999999645, -58.51619795479999908 ) ) ;
#26993 = CARTESIAN_POINT ( 'NONE',  ( -23.87963657974803056, -15.55698410987797331, 5.506989586000016423 ) ) ;
#26994 = FACE_OUTER_BOUND ( 'NONE', #24999, .T. ) ;
#26995 = CARTESIAN_POINT ( 'NONE',  ( 24.02382125689999981, -13.98923529139999999, 223.9040349389999847 ) ) ;
#26996 = CARTESIAN_POINT ( 'NONE',  ( -1.841797396446221091, -26.73663745407121795, 210.0000000000000284 ) ) ;
#26997 = CARTESIAN_POINT ( 'NONE',  ( 1.770085743148440027, -3.528255691684338391, -0.6999999999999995115 ) ) ;
#26998 = CARTESIAN_POINT ( 'NONE',  ( -4.778179638654715511, -31.66384348256136150, 0.5017677510000262409 ) ) ;
#26999 = CARTESIAN_POINT ( 'NONE',  ( 0.6812178525677142771, -27.49175526060846408, 4.123857012729932769 ) ) ;
#27000 = CARTESIAN_POINT ( 'NONE',  ( -10.69999999997381401, -28.84292916499192927, -30.79962415685015742 ) ) ;
#27001 = CARTESIAN_POINT ( 'NONE',  ( 24.41841038956698640, 14.69667349781389376, 6.099998581000020792 ) ) ;
#27002 = VECTOR ( 'NONE', #10347, 1000.000000000000000 ) ;
#27003 = AXIS2_PLACEMENT_3D ( 'NONE', #5922, #607, #12545 ) ;
#27004 = CARTESIAN_POINT ( 'NONE',  ( -5.159343048259773745, -26.29982486972314604, 20.68509006311345644 ) ) ;
#27005 = CARTESIAN_POINT ( 'NONE',  ( -0.3775595308337927891, -28.49777658967324356, 5.680150179000031940 ) ) ;
#27006 = ORIENTED_EDGE ( 'NONE', *, *, #9107, .T. ) ;
#27007 = CARTESIAN_POINT ( 'NONE',  ( 11.30445670279999959, -24.42656466549999905, -1.476955110899999646 ) ) ;
#27008 = FILL_AREA_STYLE ('',( #27462 ) ) ;
#27009 = CARTESIAN_POINT ( 'NONE',  ( 24.09271802119999961, -13.87022289859999979, 226.1000014189999945 ) ) ;
#27010 = EDGE_CURVE ( 'NONE', #18572, #15181, #12751, .T. ) ;
#27011 = CARTESIAN_POINT ( 'NONE',  ( -4.069925668896384963, 4.914984763948436530, -63.47933298482501385 ) ) ;
#27012 = ORIENTED_EDGE ( 'NONE', *, *, #24678, .F. ) ;
#27013 = VERTEX_POINT ( 'NONE', #18458 ) ;
#27014 = EDGE_CURVE ( 'NONE', #22831, #11286, #13742, .T. ) ;
#27015 = CARTESIAN_POINT ( 'NONE',  ( 13.81022701813574116, -26.50938575128768804, 0.000000000000000000 ) ) ;
#27016 = ADVANCED_FACE ( 'NONE', ( #11385 ), #6713, .T. ) ;
#27017 = ORIENTED_EDGE ( 'NONE', *, *, #27674, .T. ) ;
#27018 = VERTEX_POINT ( 'NONE', #27586 ) ;
#27019 = DIRECTION ( 'NONE',  ( -0.000000000000000000, 1.000000000000000000, -2.257145581549999994E-12 ) ) ;
#27020 = CARTESIAN_POINT ( 'NONE',  ( -24.32472894358752313, 13.45989150749028873, 3.899998581000013509 ) ) ;
#27021 = CARTESIAN_POINT ( 'NONE',  ( -20.19076655603533155, -17.71015691556361205, 143.2171415880000040 ) ) ;
#27022 = AXIS2_PLACEMENT_3D ( 'NONE', #22572, #15628, #10303 ) ;
#27023 = B_SPLINE_CURVE_WITH_KNOTS ( 'NONE', 5,
 ( #13834, #6588, #23446, #3765, #13993, #30673 ),
 .UNSPECIFIED., .F., .F.,
 ( 6, 6 ),
 ( -2.300779653509999800, 0.000000000000000000 ),
 .UNSPECIFIED. ) ;
#27024 = CARTESIAN_POINT ( 'NONE',  ( 9.479780402439999420, -7.539304615940000787, 231.9999991140000191 ) ) ;
#27025 = FACE_OUTER_BOUND ( 'NONE', #4880, .T. ) ;
#27026 = CARTESIAN_POINT ( 'NONE',  ( -3.950034095761360664, 2.484763540022561834, -9.945475902800005485 ) ) ;
#27027 = CARTESIAN_POINT ( 'NONE',  ( 28.45771199700000054, -7.455071025909999705, 229.4982322489999831 ) ) ;
#27028 = ORIENTED_EDGE ( 'NONE', *, *, #30294, .T. ) ;
#27029 = CARTESIAN_POINT ( 'NONE',  ( 2.877784302101842773, -3.523144701061436734, -44.10000000002499831 ) ) ;
#27030 = CARTESIAN_POINT ( 'NONE',  ( -24.54452542612009225, -14.48555670042145138, 3.920144560000005107 ) ) ;
#27031 = CARTESIAN_POINT ( 'NONE',  ( -2.322678811625143780, -3.635533071076384015, -21.70891267860000795 ) ) ;
#27032 = DIRECTION ( 'NONE',  ( -1.000000000000000000, -1.433034374091448024E-13, -1.199006074478416896E-12 ) ) ;
#27033 = DIRECTION ( 'NONE',  ( 2.257150022439999944E-12, 0.000000000000000000, 1.000000000000000000 ) ) ;
#27034 = LINE ( 'NONE', #17579, #23351 ) ;
#27035 = CARTESIAN_POINT ( 'NONE',  ( 8.700000000270996736, -18.23122067931645773, -34.51216076560373125 ) ) ;
#27036 = CARTESIAN_POINT ( 'NONE',  ( 2.534862810676351330, -4.171999357468124003, -46.56669147672499065 ) ) ;
#27037 = COLOUR_RGB ( '', 0.08235294, 0.09019608, 0.10196078) ;
#27038 = CARTESIAN_POINT ( 'NONE',  ( -27.92857142860000152, 1.776356839399999804E-15, 37.93968498539999956 ) ) ;
#27039 = CARTESIAN_POINT ( 'NONE',  ( -8.699999999694114194, -28.22468611108677194, -31.13863906519358693 ) ) ;
#27040 = CARTESIAN_POINT ( 'NONE',  ( -19.39816331875209698, 20.00000148357435137, 230.3275357089658542 ) ) ;
#27041 = DIRECTION ( 'NONE',  ( -0.8090169943751909232, 0.5877852522921378498, 0.000000000000000000 ) ) ;
#27042 = ADVANCED_FACE ( 'NONE', ( #13264 ), #14334, .T. ) ;
#27043 = AXIS2_PLACEMENT_3D ( 'NONE', #15838, #3874, #22756 ) ;
#27044 = CARTESIAN_POINT ( 'NONE',  ( -17.10181184920913822, -10.07643063668447958, -0.6999999999999785283 ) ) ;
#27045 = ORIENTED_EDGE ( 'NONE', *, *, #23502, .T. ) ;
#27046 = CARTESIAN_POINT ( 'NONE',  ( -4.188726303739433554, 1.192588472141202560, -31.30158078970000801 ) ) ;
#27047 = CIRCLE ( 'NONE', #30589, 26.80000000000000071 ) ;
#27048 = EDGE_LOOP ( 'NONE', ( #26095, #30980, #2427, #12567, #11690 ) ) ;
#27049 = FACE_OUTER_BOUND ( 'NONE', #29720, .T. ) ;
#27050 = CARTESIAN_POINT ( 'NONE',  ( 5.066518387468507356, -3.138291312573631586, -49.33324460762499797 ) ) ;
#27051 = ORIENTED_EDGE ( 'NONE', *, *, #20909, .F. ) ;
#27052 = ORIENTED_EDGE ( 'NONE', *, *, #8216, .F. ) ;
#27053 = DIRECTION ( 'NONE',  ( 1.000000000000000000, 0.000000000000000000, 0.000000000000000000 ) ) ;
#27054 = VERTEX_POINT ( 'NONE', #6501 ) ;
#27055 = VERTEX_POINT ( 'NONE', #20352 ) ;
#27056 = CARTESIAN_POINT ( 'NONE',  ( 24.48837202150000181, -14.58033361329999877, 226.0424736289999714 ) ) ;
#27057 = CARTESIAN_POINT ( 'NONE',  ( 24.00926693399461342, 14.01467022386263395, 3.957524335000017768 ) ) ;
#27058 = FACE_BOUND ( 'NONE', #10447, .T. ) ;
#27059 = CARTESIAN_POINT ( 'NONE',  ( 3.306876859848844941, 3.897974197644354266, -35.69999999999999574 ) ) ;
#27060 = CIRCLE ( 'NONE', #17986, 27.92857142860000152 ) ;
#27061 = DIRECTION ( 'NONE',  ( 4.428977494234582379E-12, 0.8987940462991651502, -0.4383711467890810676 ) ) ;
#27062 = CARTESIAN_POINT ( 'NONE',  ( -5.096481347195676470, -0.2862171934127135109, -0.6999999999999991784 ) ) ;
#27063 = PLANE ( 'NONE',  #14253 ) ;
#27064 = CARTESIAN_POINT ( 'NONE',  ( -27.63177371549999961, 3.383804565940000193E-15, 42.63947604850000772 ) ) ;
#27065 = CIRCLE ( 'NONE', #22049, 26.80000000000000071 ) ;
#27066 = CARTESIAN_POINT ( 'NONE',  ( 4.310466091822801715, 1.786666325167806546, -11.99261350020000272 ) ) ;
#27067 = CARTESIAN_POINT ( 'NONE',  ( 3.157381476932436648, -2.999772911539579034, -29.55126389020000133 ) ) ;
#27068 = CARTESIAN_POINT ( 'NONE',  ( -7.737355262860049265, -15.87657168464556534, -74.65692906436845533 ) ) ;
#27069 = VECTOR ( 'NONE', #3571, 1000.000000000000114 ) ;
#27070 = CARTESIAN_POINT ( 'NONE',  ( 24.60726958095619565, -14.37955347759689317, 5.901399682999991292 ) ) ;
#27071 = EDGE_CURVE ( 'NONE', #11066, #1347, #2211, .T. ) ;
#27072 = CARTESIAN_POINT ( 'NONE',  ( 10.69999999999999929, 19.99999999999999645, -22.39999999999999858 ) ) ;
#27073 = DIRECTION ( 'NONE',  ( 2.764840495839172918E-12, 0.9128796883888953273, -0.4082287037029531107 ) ) ;
#27074 = CARTESIAN_POINT ( 'NONE',  ( 17.16657240421717390, -9.000000000001264766, -0.6999999999999784173 ) ) ;
#27075 = CARTESIAN_POINT ( 'NONE',  ( 4.556810990865953315, -1.030009251744165688, -32.78377053309999667 ) ) ;
#27076 = EDGE_CURVE ( 'NONE', #10071, #25355, #17375, .T. ) ;
#27077 = CARTESIAN_POINT ( 'NONE',  ( 9.799999999997906386, -15.94902145823454198, -35.53273252495090873 ) ) ;
#27078 = CARTESIAN_POINT ( 'NONE',  ( 14.65261876681249120, -26.16807071656643657, -23.10688672985826742 ) ) ;
#27079 = CARTESIAN_POINT ( 'NONE',  ( 0.3832430167609999772, -28.49789927060000139, 223.9576737099999946 ) ) ;
#27080 = EDGE_LOOP ( 'NONE', ( #17690, #25307, #12585, #12758, #25119, #25738, #12862 ) ) ;
#27081 = EDGE_CURVE ( 'NONE', #27427, #22997, #13771, .T. ) ;
#27082 = AXIS2_PLACEMENT_3D ( 'NONE', #27602, #10617, #19911 ) ;
#27083 = CYLINDRICAL_SURFACE ( 'NONE', #24815, 3.000000000000001776 ) ;
#27084 = CARTESIAN_POINT ( 'NONE',  ( 13.39900052630364335, 20.99999999989583088, -68.94364016086436209 ) ) ;
#27085 = ORIENTED_EDGE ( 'NONE', *, *, #668, .F. ) ;
#27086 = CARTESIAN_POINT ( 'NONE',  ( 7.000000000277405654, -5.572998883592096497, -27.02754848641193419 ) ) ;
#27087 = CARTESIAN_POINT ( 'NONE',  ( -9.999999999969999109, -43.95328087550000618, -27.24755286569999768 ) ) ;
#27088 = ORIENTED_EDGE ( 'NONE', *, *, #10549, .F. ) ;
#27089 = LINE ( 'NONE', #5525, #11179 ) ;
#27090 = EDGE_LOOP ( 'NONE', ( #18601, #21880, #20157, #12229 ) ) ;
#27091 = VERTEX_POINT ( 'NONE', #27904 ) ;
#27092 = PRESENTATION_STYLE_ASSIGNMENT (( #5528 ) ) ;
#27093 = VERTEX_POINT ( 'NONE', #1321 ) ;
#27094 = CARTESIAN_POINT ( 'NONE',  ( -17.59696597919420213, 10.20816091468181774, -0.6999999999999784173 ) ) ;
#27095 = AXIS2_PLACEMENT_3D ( 'NONE', #25259, #3691, #13293 ) ;
#27096 = CARTESIAN_POINT ( 'NONE',  ( -2.020725942269999909, -3.500000000000000000, 230.5235986622430175 ) ) ;
#27097 = EDGE_CURVE ( 'NONE', #2571, #19758, #4723, .T. ) ;
#27098 = CARTESIAN_POINT ( 'NONE',  ( 0.000000000000000000, 0.000000000000000000, -85.94068374632500706 ) ) ;
#27099 = ORIENTED_EDGE ( 'NONE', *, *, #20120, .F. ) ;
#27100 = CARTESIAN_POINT ( 'NONE',  ( -25.05552767696902450, 13.58331698520493269, 6.079865069000017996 ) ) ;
#27101 = LINE ( 'NONE', #25048, #20068 ) ;
#27102 = CARTESIAN_POINT ( 'NONE',  ( 4.933588760076037971, -27.05494253741616362, 209.5115863151182793 ) ) ;
#27103 = EDGE_CURVE ( 'NONE', #29126, #2375, #9531, .T. ) ;
#27104 = CARTESIAN_POINT ( 'NONE',  ( -19.80535357367646654, 19.50875577052770993, 2.200000064000007249 ) ) ;
#27105 = EDGE_LOOP ( 'NONE', ( #28915, #3850, #22258, #8742 ) ) ;
#27106 = CARTESIAN_POINT ( 'NONE',  ( 4.373195337096347224, -2.904765488536225515, -0.5587547301999993277 ) ) ;
#27107 = CARTESIAN_POINT ( 'NONE',  ( 3.931047123110473329, -1.876836795983962469, -20.88180150029999993 ) ) ;
#27108 = CARTESIAN_POINT ( 'NONE',  ( -26.79999999999999361, -1.754055898254257118, 193.2171415879999756 ) ) ;
#27109 = CARTESIAN_POINT ( 'NONE',  ( 23.81866167241657806, 14.33570040768432996, 6.099998581000020792 ) ) ;
#27110 = CARTESIAN_POINT ( 'NONE',  ( -14.00000000000000000, 21.70000000000000284, -62.80809805499999499 ) ) ;
#27111 = LINE ( 'NONE', #20647, #17313 ) ;
#27112 = CARTESIAN_POINT ( 'NONE',  ( 10.69999999995908091, -34.38203972397853647, -24.27123760832591515 ) ) ;
#27113 = MECHANICAL_DESIGN_GEOMETRIC_PRESENTATION_REPRESENTATION (  '', ( #6515 ), #29625 ) ;
#27114 = AXIS2_PLACEMENT_3D ( 'NONE', #19906, #24161, #16911 ) ;
#27115 = LINE ( 'NONE', #17052, #7670 ) ;
#27116 = CARTESIAN_POINT ( 'NONE',  ( -11.02573875399999892, -24.63456740089999997, -1.660048605199998528 ) ) ;
#27117 = CARTESIAN_POINT ( 'NONE',  ( 4.639038166103790495, -9.671115015700310735, -32.76225121019675157 ) ) ;
#27118 = ORIENTED_EDGE ( 'NONE', *, *, #26168, .F. ) ;
#27119 = CARTESIAN_POINT ( 'NONE',  ( -4.907595108195073941, 2.436408417514825953, -55.99877225282499182 ) ) ;
#27120 = CARTESIAN_POINT ( 'NONE',  ( -13.67718144140000014, 20.99999999999999645, -57.16242377749999548 ) ) ;
#27121 = EDGE_CURVE ( 'NONE', #19928, #28095, #29415, .T. ) ;
#27122 = B_SPLINE_CURVE_WITH_KNOTS ( 'NONE', 5,
 ( #20722, #10652, #30157, #1061, #3407, #11125, #8277, #7971, #8429, #10816, #18190, #3724, #10505, #17871, #27476 ),
 .UNSPECIFIED., .F., .F.,
 ( 6, 3, 3, 3, 6 ),
 ( 0.000000000000000000, 0.1000000000028630903, 0.3999999999999999667, 0.7000000000005727196, 1.000000000000000000 ),
 .UNSPECIFIED. ) ;
#27123 = CARTESIAN_POINT ( 'NONE',  ( -24.92917479049725316, 13.61031708633488613, 0.7069258409999890080 ) ) ;
#27124 = CARTESIAN_POINT ( 'NONE',  ( -4.078087104978500577, -0.3378962543220449533, -68.10000000002501963 ) ) ;
#27125 = ORIENTED_EDGE ( 'NONE', *, *, #5870, .T. ) ;
#27126 = EDGE_LOOP ( 'NONE', ( #11126, #22328, #19111, #5492 ) ) ;
#27127 = CARTESIAN_POINT ( 'NONE',  ( -1.097913990535764883, 3.477304208260869167, -92.06382165379621085 ) ) ;
#27128 = FILL_AREA_STYLE_COLOUR ( '', #9252 ) ;
#27129 = ORIENTED_EDGE ( 'NONE', *, *, #1198, .F. ) ;
#27130 = CARTESIAN_POINT ( 'NONE',  ( -17.79876841389999598, -8.472631907500000281, -1.399999999599998990 ) ) ;
#27131 = LINE ( 'NONE', #862, #1915 ) ;
#27132 = ADVANCED_FACE ( 'NONE', ( #12414 ), #5172, .T. ) ;
#27133 = ORIENTED_EDGE ( 'NONE', *, *, #20399, .F. ) ;
#27134 = CARTESIAN_POINT ( 'NONE',  ( -4.543473910928013559, 0.02303893552233737124, -62.17122063472501026 ) ) ;
#27135 = CARTESIAN_POINT ( 'NONE',  ( -27.71720220739999974, 1.978861519090000090E-11, 229.4485730569999760 ) ) ;
#27136 = ADVANCED_FACE ( 'NONE', ( #164 ), #2760, .F. ) ;
#27137 = B_SPLINE_CURVE_WITH_KNOTS ( 'NONE', 3,
 ( #6939, #5044, #21263, #21895, #14653, #4578, #24238, #2683, #9925, #12278, #26145, #342 ),
 .UNSPECIFIED., .F., .F.,
 ( 4, 2, 2, 2, 2, 4 ),
 ( 0.000000000000000000, 0.2500000000000012212, 0.3750000000000017208, 0.5000000000000022204, 0.7500000000000011102, 1.000000000000000000 ),
 .UNSPECIFIED. ) ;
#27138 = CARTESIAN_POINT ( 'NONE',  ( 16.29899378188139281, 10.30852736161794958, 0.000000000000000000 ) ) ;
#27139 = DIRECTION ( 'NONE',  ( 0.000000000000000000, 0.3420201433259318913, -0.9396926207858126157 ) ) ;
#27140 = CARTESIAN_POINT ( 'NONE',  ( 9.897162125286889989, -25.37356426548040389, 188.3395398250000028 ) ) ;
#27141 = CARTESIAN_POINT ( 'NONE',  ( -4.861312627816292142, -17.80543024185618606, -28.79488058873301171 ) ) ;
#27142 = ORIENTED_EDGE ( 'NONE', *, *, #2524, .T. ) ;
#27143 = ADVANCED_FACE ( 'NONE', ( #27049 ), #14482, .T. ) ;
#27144 = CARTESIAN_POINT ( 'NONE',  ( -24.49999999589999788, 3.000285566369999841E-15, 90.00000000000000000 ) ) ;
#27145 = CARTESIAN_POINT ( 'NONE',  ( 17.99586598600000187, 19.96083381589999917, 229.9999934530000019 ) ) ;
#27146 = ORIENTED_EDGE ( 'NONE', *, *, #21380, .F. ) ;
#27147 = CARTESIAN_POINT ( 'NONE',  ( -8.000000000000000000, -17.05999687705277879, -77.21601615383784178 ) ) ;
#27148 = DIRECTION ( 'NONE',  ( 4.901511854548699870E-24, -1.000000000000000000, 2.257145581550420047E-12 ) ) ;
#27149 = DIRECTION ( 'NONE',  ( -1.224646799149999836E-16, 1.000000000000000000, 0.000000000000000000 ) ) ;
#27150 = CARTESIAN_POINT ( 'NONE',  ( 23.50666810109999716, -14.84174128299999929, 224.8958160969999938 ) ) ;
#27151 = CARTESIAN_POINT ( 'NONE',  ( -23.24663841809999809, -14.69162354060000020, 5.000000000000000000 ) ) ;
#27152 = CIRCLE ( 'NONE', #29664, 27.23548387080000310 ) ;
#27153 = CARTESIAN_POINT ( 'NONE',  ( -0.8663085823657415974, -3.674610306298811135, -0.6999999999999992895 ) ) ;
#27154 = EDGE_CURVE ( 'NONE', #30881, #9514, #23020, .T. ) ;
#27155 = CARTESIAN_POINT ( 'NONE',  ( -25.65182985565638418, -15.32775674290634704, 0.2374258030000131470 ) ) ;
#27156 = DIRECTION ( 'NONE',  ( 0.000000000000000000, 1.000000000000000000, 0.000000000000000000 ) ) ;
#27157 = FACE_OUTER_BOUND ( 'NONE', #27048, .T. ) ;
#27158 = DIRECTION ( 'NONE',  ( 0.000000000000000000, 0.000000000000000000, 1.000000000000000000 ) ) ;
#27159 = CARTESIAN_POINT ( 'NONE',  ( -8.158046243928263053, -25.52871334855630892, 23.09233687717909334 ) ) ;
#27160 = CARTESIAN_POINT ( 'NONE',  ( 0.000000000000000000, 0.000000000000000000, 115.0000000000000000 ) ) ;
#27161 = VERTEX_POINT ( 'NONE', #12568 ) ;
#27162 = CIRCLE ( 'NONE', #21648, 2.999999999999999112 ) ;
#27163 = EDGE_CURVE ( 'NONE', #10568, #19354, #3122, .T. ) ;
#27164 = CARTESIAN_POINT ( 'NONE',  ( 11.62710820729999917, -24.17108566339999953, -1.401657795999995626 ) ) ;
#27165 = CARTESIAN_POINT ( 'NONE',  ( 9.700000000183711890, -14.03197393871519516, -36.39001241340137938 ) ) ;
#27166 = CARTESIAN_POINT ( 'NONE',  ( 1.645540681903832070, 2.658966097310066168, -42.11383941009797383 ) ) ;
#27167 = CARTESIAN_POINT ( 'NONE',  ( 2.637655088286918748, -3.673227524439518277, -61.92197827312500635 ) ) ;
#27168 = ORIENTED_EDGE ( 'NONE', *, *, #8132, .T. ) ;
#27169 = ORIENTED_EDGE ( 'NONE', *, *, #12468, .F. ) ;
#27170 = CARTESIAN_POINT ( 'NONE',  ( 27.26968166180262898, -9.459502808761374837, 0.02487529600000981667 ) ) ;
#27171 = VERTEX_POINT ( 'NONE', #935 ) ;
#27172 = ORIENTED_EDGE ( 'NONE', *, *, #26132, .T. ) ;
#27173 = CARTESIAN_POINT ( 'NONE',  ( 353541.3905930228066, -322767.6580542778247, 144295.1096003104758 ) ) ;
#27174 = CARTESIAN_POINT ( 'NONE',  ( 25.12046395012945155, -13.46291002088068289, 3.957489296000010981 ) ) ;
#27175 = CARTESIAN_POINT ( 'NONE',  ( -25.22658730140538808, -13.26242337740151811, 224.8524123125729943 ) ) ;
#27176 = CARTESIAN_POINT ( 'NONE',  ( -17.04621913067799710, -27.00000000000000355, -34.17350269210000135 ) ) ;
#27177 = CARTESIAN_POINT ( 'NONE',  ( 24.70448873180906446, -12.74983733560190302, 5.760266709000011254 ) ) ;
#27178 = CARTESIAN_POINT ( 'NONE',  ( 1.423247168829999991E-05, 20.00000000000000000, 230.0000000010000178 ) ) ;
#27179 = ORIENTED_EDGE ( 'NONE', *, *, #19917, .T. ) ;
#27180 = CARTESIAN_POINT ( 'NONE',  ( 2.047979779693930524, -3.657782141751653615, -44.10000000002499121 ) ) ;
#27181 = DIRECTION ( 'NONE',  ( 2.416122857340496113E-12, -0.9341647027306024809, -0.3568421334038978099 ) ) ;
#27182 = VECTOR ( 'NONE', #17851, 1000.000000000000000 ) ;
#27183 = CARTESIAN_POINT ( 'NONE',  ( -3.251750336246070461, -5.089746299513510763, -22.30891267860000937 ) ) ;
#27184 = CARTESIAN_POINT ( 'NONE',  ( -12.75378086759999796, -27.00000000000000355, -34.17350269210000135 ) ) ;
#27185 = CARTESIAN_POINT ( 'NONE',  ( -16.52606180369280864, 9.934045360728056551, -4.336808689942018722E-16 ) ) ;
#27186 = EDGE_CURVE ( 'NONE', #6080, #19159, #29714, .T. ) ;
#27187 = DIRECTION ( 'NONE',  ( 0.000000000000000000, 0.000000000000000000, 1.000000000000000000 ) ) ;
#27188 = CARTESIAN_POINT ( 'NONE',  ( -13.99999999969999820, 20.99999999999999645, -63.10000000000000142 ) ) ;
#27189 = CARTESIAN_POINT ( 'NONE',  ( 3.054834669310706907, -5.027794097514915350, -45.76669147682500238 ) ) ;
#27190 = ADVANCED_FACE ( 'NONE', ( #6099 ), #27354, .F. ) ;
#27191 = CARTESIAN_POINT ( 'NONE',  ( -17.00495585196167525, 12.09604337527003892, -1.400000000000001910 ) ) ;
#27192 = EDGE_CURVE ( 'NONE', #19512, #6463, #17593, .T. ) ;
#27193 = FACE_OUTER_BOUND ( 'NONE', #329, .T. ) ;
#27194 = CARTESIAN_POINT ( 'NONE',  ( -18.40310945181386515, 20.00006322233851108, 230.6579732124013162 ) ) ;
#27195 = CARTESIAN_POINT ( 'NONE',  ( -24.76521256262104842, -10.24325429074770000, 43.21714158839976250 ) ) ;
#27196 = EDGE_CURVE ( 'NONE', #14172, #7936, #2403, .T. ) ;
#27197 = CARTESIAN_POINT ( 'NONE',  ( 7.838355892653583012, -25.63086664713628693, 22.66947412054902244 ) ) ;
#27198 = ORIENTED_EDGE ( 'NONE', *, *, #23830, .F. ) ;
#27199 = CARTESIAN_POINT ( 'NONE',  ( 6.379535387291454640, -1.442012952481606991, -33.38377053310000520 ) ) ;
#27200 = VERTEX_POINT ( 'NONE', #8298 ) ;
#27201 = CARTESIAN_POINT ( 'NONE',  ( -8.699999999675029017, -13.90762120762749809, -34.05293844846480056 ) ) ;
#27202 = CARTESIAN_POINT ( 'NONE',  ( 5.782578939028539367, 2.564649547393091478, -52.35998794302499704 ) ) ;
#27203 = EDGE_LOOP ( 'NONE', ( #14638, #24616, #10904, #13891 ) ) ;
#27204 = EDGE_LOOP ( 'NONE', ( #2210, #10744, #19867, #19310 ) ) ;
#27205 = CARTESIAN_POINT ( 'NONE',  ( -34.49410526157860346, 3.395238951591843080, 2.221583959605973657 ) ) ;
#27206 = AXIS2_PLACEMENT_3D ( 'NONE', #24067, #5471, #12706 ) ;
#27207 = EDGE_LOOP ( 'NONE', ( #23776, #11222, #22142, #17406 ) ) ;
#27208 = EDGE_LOOP ( 'NONE', ( #13505, #21596, #15570, #6728 ) ) ;
#27209 = CARTESIAN_POINT ( 'NONE',  ( 1.057488903014505443E-10, -103.0613381315276484, 16.56805218638653798 ) ) ;
#27210 = CARTESIAN_POINT ( 'NONE',  ( 14.60916111670818474, -28.04296597385482315, 1.000000000000000888 ) ) ;
#27211 = CARTESIAN_POINT ( 'NONE',  ( 0.000000000000000000, 0.000000000000000000, 137.9396849850000137 ) ) ;
#27212 = CARTESIAN_POINT ( 'NONE',  ( 1.669414676675136322, 4.650989935738711445, -35.69999999999999574 ) ) ;
#27213 = FACE_BOUND ( 'NONE', #2024, .T. ) ;
#27214 = CARTESIAN_POINT ( 'NONE',  ( -20.50698707569999968, 18.79638478329999884, 226.0000000000000000 ) ) ;
#27215 = CARTESIAN_POINT ( 'NONE',  ( -3.915568621502395708, 1.076153403323427682, -0.6999999999999992895 ) ) ;
#27216 = CARTESIAN_POINT ( 'NONE',  ( 3.123710955063065065, -2.074832491810036039, 0.04124526979999709742 ) ) ;
#27217 = DIRECTION ( 'NONE',  ( 0.000000000000000000, 0.000000000000000000, 1.000000000000000000 ) ) ;
#27218 = CARTESIAN_POINT ( 'NONE',  ( 8.903108651239925564, -22.82508830966962421, 190.0000000000000000 ) ) ;
#27219 = CARTESIAN_POINT ( 'NONE',  ( 2.880392382415891017, 3.817472992077249661, -15.16546858840000489 ) ) ;
#27220 = CARTESIAN_POINT ( 'NONE',  ( 2.039164074698236906, -5.746172002732055084, -29.65632401680000285 ) ) ;
#27221 = LINE ( 'NONE', #5664, #3116 ) ;
#27222 = CARTESIAN_POINT ( 'NONE',  ( -24.21578250576721913, -13.65559031243956412, 226.0732541239276259 ) ) ;
#27223 = CARTESIAN_POINT ( 'NONE',  ( -7.861312627756137594, -6.912605513598457208, -37.44547201166600559 ) ) ;
#27224 = DIRECTION ( 'NONE',  ( 0.000000000000000000, 0.000000000000000000, -1.000000000000000000 ) ) ;
#27225 = FACE_OUTER_BOUND ( 'NONE', #16409, .T. ) ;
#27226 = AXIS2_PLACEMENT_3D ( 'NONE', #10822, #8436, #3570 ) ;
#27227 = CARTESIAN_POINT ( 'NONE',  ( 0.5401834767575381946, -27.79499634052776358, 6.099998581000020792 ) ) ;
#27228 = CARTESIAN_POINT ( 'NONE',  ( -16.81341597756113515, 9.900182044522454206, -1.000005633855494125E-09 ) ) ;
#27229 = CARTESIAN_POINT ( 'NONE',  ( -7.300482373339721498, -8.173122728246529078, -36.83067668763386848 ) ) ;
#27230 = ADVANCED_FACE ( 'NONE', ( #29865, #18051 ), #22331, .F. ) ;
#27231 = ORIENTED_EDGE ( 'NONE', *, *, #12169, .F. ) ;
#27232 = DIRECTION ( 'NONE',  ( -0.7198537139083028835, 0.6941258031311204890, 0.000000000000000000 ) ) ;
#27233 = CARTESIAN_POINT ( 'NONE',  ( 11.25000838620000110, 19.99999999999999645, -0.7501799203000064642 ) ) ;
#27234 = ORIENTED_EDGE ( 'NONE', *, *, #26568, .T. ) ;
#27235 = LINE ( 'NONE', #5675, #24889 ) ;
#27236 = DIRECTION ( 'NONE',  ( 0.000000000000000000, 0.000000000000000000, 1.000000000000000000 ) ) ;
#27237 = EDGE_LOOP ( 'NONE', ( #27814, #7012, #28991, #4415 ) ) ;
#27238 = CARTESIAN_POINT ( 'NONE',  ( 24.93720649360215802, -13.79881813812812297, 6.099998581000020792 ) ) ;
#27239 = EDGE_LOOP ( 'NONE', ( #15162, #16596, #26965, #9669 ) ) ;
#27240 = ORIENTED_EDGE ( 'NONE', *, *, #19711, .T. ) ;
#27241 = FILL_AREA_STYLE ('',( #825 ) ) ;
#27242 = ORIENTED_EDGE ( 'NONE', *, *, #2351, .F. ) ;
#27243 = CARTESIAN_POINT ( 'NONE',  ( 28.45771199730000234, 2.371705317339999772E-14, 229.4982322489999831 ) ) ;
#27244 = PRESENTATION_LAYER_ASSIGNMENT (  '', '', ( #22222 ) ) ;
#27245 = AXIS2_PLACEMENT_3D ( 'NONE', #8393, #30452, #1181 ) ;
#27246 = DIRECTION ( 'NONE',  ( 0.000000000000000000, 0.000000000000000000, 1.000000000000000000 ) ) ;
#27247 = EDGE_CURVE ( 'NONE', #30387, #368, #21916, .T. ) ;
#27248 = CARTESIAN_POINT ( 'NONE',  ( -7.999999999659703320, -18.25871770053183596, -36.49215491283803914 ) ) ;
#27249 = CARTESIAN_POINT ( 'NONE',  ( 10.45000000009999930, -26.99999999999950617, -28.39999999990030588 ) ) ;
#27250 = CARTESIAN_POINT ( 'NONE',  ( -24.83273907627866706, 12.49792087830325471, 5.208434320000010942 ) ) ;
#27251 = PRODUCT_DEFINITION_SHAPE ( 'NONE', 'NONE',  #3296 ) ;
#27252 = B_SPLINE_CURVE_WITH_KNOTS ( 'NONE', 3,
 ( #11140, #21204, #6092, #20577, #4058, #13654 ),
 .UNSPECIFIED., .F., .F.,
 ( 4, 2, 4 ),
 ( 0.000000000000000000, 0.5000000000000000000, 1.000000000000000000 ),
 .UNSPECIFIED. ) ;
#27253 = CARTESIAN_POINT ( 'NONE',  ( 28.35945635836379708, 7.983396865348648674, 8.000000000000007105 ) ) ;
#27254 = CARTESIAN_POINT ( 'NONE',  ( -7.665314379701609226, -5.675505773878507298, -27.25677405838692735 ) ) ;
#27255 = CARTESIAN_POINT ( 'NONE',  ( 23.88690489929999927, -14.22221811490000043, 223.9575292099999899 ) ) ;
#27256 = ADVANCED_FACE ( 'NONE', ( #3583 ), #5797, .T. ) ;
#27257 = CARTESIAN_POINT ( 'NONE',  ( 5.523879335194060936, -0.1907134851046367874, -3.685409721200002320 ) ) ;
#27258 = CARTESIAN_POINT ( 'NONE',  ( 6.096654317658788180, 0.1519075334363156893, -20.07661200060000084 ) ) ;
#27259 = CARTESIAN_POINT ( 'NONE',  ( -1.097519451206210750, -28.47920044965180608, 224.7095162403817312 ) ) ;
#27260 = AXIS2_PLACEMENT_3D ( 'NONE', #2367, #22449, #9594 ) ;
#27261 = DIRECTION ( 'NONE',  ( 0.000000000000000000, 0.9396926207858125046, 0.3420201433259318358 ) ) ;
#27262 = CARTESIAN_POINT ( 'NONE',  ( 24.80399018339999628, -14.03663607480000053, 223.9201473980000117 ) ) ;
#27263 = CARTESIAN_POINT ( 'NONE',  ( -25.42409647459999888, 14.10343940200000112, 229.4982322489999831 ) ) ;
#27264 = DIRECTION ( 'NONE',  ( 0.000000000000000000, 1.000000000000000000, 0.000000000000000000 ) ) ;
#27265 = CARTESIAN_POINT ( 'NONE',  ( 1.366018022090341510, 3.254826447622997776, -0.6999999999999783062 ) ) ;
#27266 = CARTESIAN_POINT ( 'NONE',  ( -19.80526803560000104, 19.50877411510000314, 227.3999999999999773 ) ) ;
#27267 = CARTESIAN_POINT ( 'NONE',  ( 10.97092067110000002, -24.67424207510000045, -1.714865450400004931 ) ) ;
#27268 = VERTEX_POINT ( 'NONE', #24993 ) ;
#27269 = CARTESIAN_POINT ( 'NONE',  ( 1.078097839695846494, -5.807694627614346849, -57.94125695792499897 ) ) ;
#27270 = VECTOR ( 'NONE', #8836, 999.9999999999998863 ) ;
#27271 = DIRECTION ( 'NONE',  ( 0.8660254037843290176, 0.5000000000001899592, 1.018673689593249976E-32 ) ) ;
#27272 = CARTESIAN_POINT ( 'NONE',  ( -6.108812354261965005, 0.1812703649581512422, -13.18304957890000040 ) ) ;
#27273 = CARTESIAN_POINT ( 'NONE',  ( -21.85583880085616570, 17.39748151240578267, 0.2686751170000167832 ) ) ;
#27274 = CARTESIAN_POINT ( 'NONE',  ( -4.205306023310510177, 0.5530484625032894286, -68.10000000002501963 ) ) ;
#27275 = EDGE_CURVE ( 'NONE', #14643, #21319, #215, .T. ) ;
#27276 = EDGE_LOOP ( 'NONE', ( #20339, #26786, #2371, #9875 ) ) ;
#27277 = EDGE_LOOP ( 'NONE', ( #30186, #14071, #5527, #13821, #7512 ) ) ;
#27278 = CARTESIAN_POINT ( 'NONE',  ( -1.294030826674742229, 2.220820491787859119, -95.37004441182592984 ) ) ;
#27279 =( NAMED_UNIT ( * ) SI_UNIT ( $, .STERADIAN. ) SOLID_ANGLE_UNIT ( ) );
#27280 = ORIENTED_EDGE ( 'NONE', *, *, #13051, .T. ) ;
#27281 = CARTESIAN_POINT ( 'NONE',  ( -24.39135169139981940, 14.74223402956394402, 4.689353541000001790 ) ) ;
#27282 = DIRECTION ( 'NONE',  ( 0.000000000000000000, 0.000000000000000000, -1.000000000000000000 ) ) ;
#27283 = CARTESIAN_POINT ( 'NONE',  ( 5.258991878263315378, 0.1257858540645254708, -63.31686508972500604 ) ) ;
#27284 = DIRECTION ( 'NONE',  ( 1.224606353819999829E-16, 1.000000000000000000, 0.000000000000000000 ) ) ;
#27285 = CARTESIAN_POINT ( 'NONE',  ( -25.57973247309962872, 13.96556750262912416, 1.000000000000000888 ) ) ;
#27286 = CARTESIAN_POINT ( 'NONE',  ( 10.61898076289999970, 19.99999999999999645, -42.96980960428000174 ) ) ;
#27287 = AXIS2_PLACEMENT_3D ( 'NONE', #27488, #5936, #15688 ) ;
#27288 = CARTESIAN_POINT ( 'NONE',  ( -27.54391552369999729, 3.373045395949999841E-15, 192.9562530129999800 ) ) ;
#27289 = ADVANCED_FACE ( 'NONE', ( #29559 ), #13029, .T. ) ;
#27290 = LINE ( 'NONE', #5731, #19532 ) ;
#27291 = ORIENTED_EDGE ( 'NONE', *, *, #25272, .T. ) ;
#27292 = B_SPLINE_CURVE_WITH_KNOTS ( 'NONE', 3,
 ( #13391, #25986, #18581, #16222, #6152, #15750, #28180, #23633, #25520, #25835, #20634, #4273, #27870, #11044, #3803, #1911, #21109, #9132, #11660, #4425, #18733, #6783, #2069, #18896, #23000, #1448, #6317, #30230, #4890, #14800, #12117, #21725, #14496, #21892, #9608, #24091, #16681, #28492, #2530, #26749, #12427, #11967, #23944, #493, #26601, #26291, #10078, #177, #7554, #9921, #31012, #7399, #19206, #24399, #16843, #28649, #9447, #16532, #26142, #9760, #21578, #6932, #24235, #19050, #28791, #25, #14649, #17144, #4735, #7249, #2833, #5040, #5186, #26448, #4575, #2382, #19367, #28957, #338, #16996, #2680, #22043, #7093, #11816, #14345, #14180, #19521, #23784, #12275, #29107, #2226, #21423, #17302, #27212, #5955, #3288, #12892, #5651, #13040, #794, #15105, #22343, #10384, #25004, #27059, #27365, #17747, #15249, #10537, #5807, #1252, #22801, #3437, #17604 ),
 .UNSPECIFIED., .F., .F.,
 ( 4, 2, 2, 2, 2, 1, 2, 2, 1, 1, 1, 2, 2, 1, 1, 1, 1, 1, 2, 2, 1, 1, 1, 2, 2, 1, 1, 1, 1, 2, 2, 1, 1, 1, 1, 2, 2, 1, 2, 2, 1, 2, 2, 1, 1, 1, 1, 2, 2, 1, 1, 2, 2, 1, 1, 2, 2, 1, 1, 2, 2, 1, 2, 2, 1, 1, 2, 2, 1, 2, 2, 2, 2, 2, 4 ),
 ( 0.000000000000000000, 0.06249999999999901468, 0.1249999999999980016, 0.1562499999999974742, 0.1874999999999969746, 0.2187499999999964473, 0.2343749999999961975, 0.2499999999999959477, 0.2812499999999953926, 0.2968749999999951150, 0.3046874999999949485, 0.3085937499999948930, 0.3124999999999947820, 0.3437499999999938938, 0.3593749999999935052, 0.3671874999999932832, 0.3710937499999931721, 0.3730468749999931166, 0.3740234374999931166, 0.3749999999999931166, 0.3906249999999933387, 0.3984374999999935052, 0.4023437499999935052, 0.4042968749999935052, 0.4062499999999935607, 0.4140624999999935052, 0.4179687499999935052, 0.4199218749999935607, 0.4208984374999935052, 0.4213867187499935607, 0.4218749999999936162, 0.4296874999999941158, 0.4335937499999943934, 0.4355468749999945599, 0.4365234374999946154, 0.4370117187499945599, 0.4374999999999945044, 0.4453124999999940048, 0.4462890624999938938, 0.4472656249999938383, 0.4492187499999936162, 0.4531249999999932276, 0.4570312499999928391, 0.4609374999999924505, 0.4648437499999920619, 0.4667968749999918399, 0.4677734374999917843, 0.4682617187499917288, 0.4687499999999916733, 0.4765624999999916733, 0.4804687499999916733, 0.4824218749999916733, 0.4843749999999916733, 0.4921874999999917288, 0.4960937499999917843, 0.4980468749999918399, 0.4999999999999918399, 0.5156249999999921174, 0.5234374999999922284, 0.5273437499999922284, 0.5312499999999923395, 0.5468749999999925615, 0.5546874999999927836, 0.5624999999999930056, 0.5937499999999937828, 0.6093749999999940048, 0.6171874999999941158, 0.6249999999999942268, 0.6562499999999947820, 0.6718749999999950040, 0.6874999999999951150, 0.7187499999999956701, 0.7499999999999961142, 0.8749999999999981126, 1.000000000000000000 ),
 .UNSPECIFIED. ) ;
#27293 = CARTESIAN_POINT ( 'NONE',  ( 13.99999999992460076, 21.69999999930106682, -58.04802353003142912 ) ) ;
#27294 = CARTESIAN_POINT ( 'NONE',  ( 14.84171152945997640, -29.89464157630768781, -32.50228059851001206 ) ) ;
#27295 = ORIENTED_EDGE ( 'NONE', *, *, #29764, .F. ) ;
#27296 = CARTESIAN_POINT ( 'NONE',  ( 3.691781163184647330, 0.6055607618373975987, 227.7772386881597697 ) ) ;
#27297 = CARTESIAN_POINT ( 'NONE',  ( 9.000000000000000000, 21.69999999990000106, -67.10000000019999788 ) ) ;
#27298 = FACE_BOUND ( 'NONE', #16481, .T. ) ;
#27299 = CARTESIAN_POINT ( 'NONE',  ( 24.04107748430000058, -13.95955969929999974, 223.9013459049999994 ) ) ;
#27300 = CARTESIAN_POINT ( 'NONE',  ( 16.06675444876397307, -9.020011618195203695, -1.000005633855494125E-09 ) ) ;
#27302 = B_SPLINE_CURVE_WITH_KNOTS ( 'NONE', 5,
 ( #29105, #18894, #174, #24089, #2528, #21722, #6929, #9918, #9757 ),
 .UNSPECIFIED., .F., .F.,
 ( 6, 3, 6 ),
 ( 0.000000000000000000, 53.95537973340000093, 92.42745556099998794 ),
 .UNSPECIFIED. ) ;
#27301 = DIRECTION ( 'NONE',  ( 0.000000000000000000, -1.000000000000000000, 0.000000000000000000 ) ) ;
#27303 = CARTESIAN_POINT ( 'NONE',  ( 4.216378357570000000E-10, -6.866525126269999101E-10, 227.6412452697800006 ) ) ;
#27304 = CARTESIAN_POINT ( 'NONE',  ( 11.50000000000000000, 22.40709319595134730, -62.85117013414870257 ) ) ;
#27305 = ORIENTED_EDGE ( 'NONE', *, *, #29808, .T. ) ;
#27306 = EDGE_CURVE ( 'NONE', #4930, #7075, #10754, .T. ) ;
#27307 = CARTESIAN_POINT ( 'NONE',  ( -5.361385120500000490, 31.61859227569999931, 229.0000000000000000 ) ) ;
#27308 = AXIS2_PLACEMENT_3D ( 'NONE', #13170, #20116, #27344 ) ;
#27309 = EDGE_CURVE ( 'NONE', #6070, #26662, #3754, .T. ) ;
#27310 = B_SPLINE_CURVE_WITH_KNOTS ( 'NONE', 3,
 ( #22400, #22556, #698, #7904, #7605, #15152, #847, #20030, #12947, #10438, #29628, #8057, #17653, #27265, #5702, #15310, #24913, #9820 ),
 .UNSPECIFIED., .F., .F.,
 ( 4, 2, 2, 2, 2, 2, 2, 2, 4 ),
 ( 0.000000000000000000, 0.1250000000000000000, 0.2500000000000000000, 0.3750000000000000000, 0.5000000000000000000, 0.6250000000000000000, 0.7500000000000000000, 0.8750000000000000000, 1.000000000000000000 ),
 .UNSPECIFIED. ) ;
#27311 = CARTESIAN_POINT ( 'NONE',  ( -24.76259292740833828, -10.24958551592170508, 93.21714158839989750 ) ) ;
#27312 = CARTESIAN_POINT ( 'NONE',  ( 0.1352650258152492124, -28.50015511220863118, 6.042326290000010758 ) ) ;
#27313 = EDGE_LOOP ( 'NONE', ( #3050, #25352, #21969, #2490 ) ) ;
#27314 = LINE ( 'NONE', #20228, #14275 ) ;
#27315 = EDGE_CURVE ( 'NONE', #14873, #9577, #17575, .T. ) ;
#27316 = DIRECTION ( 'NONE',  ( 0.000000000000000000, 2.256504834499999987E-12, 1.000000000000000000 ) ) ;
#27317 = CARTESIAN_POINT ( 'NONE',  ( -19.45974949220212480, 18.55460157459818760, -0.6999999999999992895 ) ) ;
#27318 = CARTESIAN_POINT ( 'NONE',  ( 3.449241269337446791, -4.803451378176493591, -62.00197827312499754 ) ) ;
#27319 = VERTEX_POINT ( 'NONE', #15220 ) ;
#27320 = VERTEX_POINT ( 'NONE', #5153 ) ;
#27322 = ADVANCED_FACE ( 'NONE', ( #10046 ), #19489, .F. ) ;
#27321 = CARTESIAN_POINT ( 'NONE',  ( 27.95617443546494130, -9.697638328662621987, 0.7069222069999991920 ) ) ;
#27323 = ORIENTED_EDGE ( 'NONE', *, *, #3810, .T. ) ;
#27324 = CIRCLE ( 'NONE', #26829, 18.16530045500000057 ) ;
#27325 = VECTOR ( 'NONE', #25934, 1000.000000000000000 ) ;
#27326 = CARTESIAN_POINT ( 'NONE',  ( 9.999999999980001775, -27.39269908193462655, -31.40000000000158664 ) ) ;
#27327 = AXIS2_PLACEMENT_3D ( 'NONE', #23851, #2294, #26361 ) ;
#27328 = CARTESIAN_POINT ( 'NONE',  ( -7.000000000054375171, -115.1185614904109542, 21.95989595794997129 ) ) ;
#27329 = DIRECTION ( 'NONE',  ( 0.8090169943751909232, 0.5877852522921378498, 0.000000000000000000 ) ) ;
#27330 = AXIS2_PLACEMENT_3D ( 'NONE', #11881, #14095, #11724 ) ;
#27331 = CARTESIAN_POINT ( 'NONE',  ( 8.700000000280979862, -17.99038303693934893, -37.01276636704596967 ) ) ;
#27332 = CARTESIAN_POINT ( 'NONE',  ( 24.32472894995379420, -13.45989151107506387, 6.099998581000020792 ) ) ;
#27333 = DIRECTION ( 'NONE',  ( 0.000000000000000000, 0.000000000000000000, -1.000000000000000000 ) ) ;
#27334 = ORIENTED_EDGE ( 'NONE', *, *, #29983, .T. ) ;
#27335 = CARTESIAN_POINT ( 'NONE',  ( 1.694282209123973093, -3.767548914987134623, -44.10000000002498410 ) ) ;
#27336 = CARTESIAN_POINT ( 'NONE',  ( 24.66346747934186112, 14.28208995963568739, 3.997248600000002927 ) ) ;
#27337 = EDGE_CURVE ( 'NONE', #6458, #15510, #5397, .T. ) ;
#27338 = CARTESIAN_POINT ( 'NONE',  ( 4.700333466414979178, 3.591691549163662511, -24.36727430110000370 ) ) ;
#27339 = CARTESIAN_POINT ( 'NONE',  ( -12.34110296562673881, -25.26652124847552017, -33.17257366193984325 ) ) ;
#27340 = CARTESIAN_POINT ( 'NONE',  ( 18.13191322300000152, 10.47263190709999492, -0.6999999999999992895 ) ) ;
#27341 = CARTESIAN_POINT ( 'NONE',  ( 2.137930486642451555, 6.059703978454344941, -45.01079303332499393 ) ) ;
#27342 = CARTESIAN_POINT ( 'NONE',  ( 8.999999999770000869, 20.99999999999999645, -45.10000000000000142 ) ) ;
#27343 = EDGE_CURVE ( 'NONE', #22531, #8030, #17116, .T. ) ;
#27344 = DIRECTION ( 'NONE',  ( 0.000000000000000000, 1.000000000000000000, 0.000000000000000000 ) ) ;
#27345 = CARTESIAN_POINT ( 'NONE',  ( -18.53535511557664961, 20.00004277161199440, 230.6343261903482187 ) ) ;
#27346 = CARTESIAN_POINT ( 'NONE',  ( -25.15951549259922260, -9.235088186050575132, 43.21714158838125996 ) ) ;
#27347 = CIRCLE ( 'NONE', #11300, 2.999999999999999556 ) ;
#27348 = AXIS2_PLACEMENT_3D ( 'NONE', #18003, #1512, #6532 ) ;
#27349 = TOROIDAL_SURFACE ( 'NONE', #3224, 18.16530045470000232, 1.000000000000000000 ) ;
#27350 = CARTESIAN_POINT ( 'NONE',  ( 5.395560604220515977, -26.25584002662961680, 20.78043813435757414 ) ) ;
#27351 = ORIENTED_EDGE ( 'NONE', *, *, #6167, .T. ) ;
#27352 = CARTESIAN_POINT ( 'NONE',  ( -0.3609073012553025150, 5.149274899367955349, -35.83268930509999706 ) ) ;
#27353 = ORIENTED_EDGE ( 'NONE', *, *, #13149, .F. ) ;
#27354 = CYLINDRICAL_SURFACE ( 'NONE', #1712, 3.999999999999999112 ) ;
#27355 = CARTESIAN_POINT ( 'NONE',  ( 3.874396413951479268, -2.399869827310083803, -49.33324460762499797 ) ) ;
#27356 = ORIENTED_EDGE ( 'NONE', *, *, #28493, .T. ) ;
#27357 = ORIENTED_EDGE ( 'NONE', *, *, #291, .F. ) ;
#27358 = CARTESIAN_POINT ( 'NONE',  ( 0.000000000000000000, 0.000000000000000000, 0.000000000000000000 ) ) ;
#27359 = ORIENTED_EDGE ( 'NONE', *, *, #7073, .F. ) ;
#27360 = EDGE_CURVE ( 'NONE', #23263, #9397, #2238, .T. ) ;
#27361 = EDGE_LOOP ( 'NONE', ( #9876, #887, #12101, #23843 ) ) ;
#27362 = COLOUR_RGB ( '', 0.40784314, 0.44705882, 0.49803922) ;
#27363 = CARTESIAN_POINT ( 'NONE',  ( -17.86397328150795971, -9.404917770633179686, 0.000000000000000000 ) ) ;
#27364 = DIRECTION ( 'NONE',  ( 0.4353787270609792981, 0.9002473904559574747, 0.000000000000000000 ) ) ;
#27365 = CARTESIAN_POINT ( 'NONE',  ( 3.491126794077959783, 3.756748552635288174, -35.70000000000000284 ) ) ;
#27366 = EDGE_CURVE ( 'NONE', #1319, #17864, #7974, .T. ) ;
#27367 = DIRECTION ( 'NONE',  ( 0.7071067811870476172, 0.7071067811860475283, -3.047758891780202378E-14 ) ) ;
#27368 = B_SPLINE_CURVE_WITH_KNOTS ( 'NONE', 3,
 ( #7874, #3313, #29131, #22067, #29283, #10103, #17331, #19861 ),
 .UNSPECIFIED., .F., .F.,
 ( 4, 2, 2, 4 ),
 ( 0.000000000000000000, 0.2500000000000001110, 0.5000000000000002220, 1.000000000000000000 ),
 .UNSPECIFIED. ) ;
#27369 = CARTESIAN_POINT ( 'NONE',  ( -18.95046173579999760, -18.95046173579999760, 115.0000000000000000 ) ) ;
#27370 = CARTESIAN_POINT ( 'NONE',  ( -4.478443094736791252, 1.857700152298996210, -0.6999999999999994005 ) ) ;
#27371 = CARTESIAN_POINT ( 'NONE',  ( 23.81776757409229361, 15.65134803726813217, 4.999998581000003384 ) ) ;
#27372 = VECTOR ( 'NONE', #15690, 1000.000000000000000 ) ;
#27373 = CARTESIAN_POINT ( 'NONE',  ( -10.00000000045684523, -29.92191803000534023, -29.18524365307803947 ) ) ;
#27374 = CARTESIAN_POINT ( 'NONE',  ( 10.46446609389999871, 20.99999999999999645, -54.63553390589999736 ) ) ;
#27375 = AXIS2_PLACEMENT_3D ( 'NONE', #13931, #23540, #9192 ) ;
#27376 = CARTESIAN_POINT ( 'NONE',  ( 3.665953941183818010, 4.858601989977915814, -14.82796858839999921 ) ) ;
#27377 = CARTESIAN_POINT ( 'NONE',  ( -3.231711866632715147, -5.662799918003592836, -30.07642233980000057 ) ) ;
#27378 = DIRECTION ( 'NONE',  ( 1.000000000000000000, -1.317089015970003879E-16, -1.110223024630000146E-15 ) ) ;
#27379 = CARTESIAN_POINT ( 'NONE',  ( -24.55259642772470130, -13.03965859083635515, 225.4961348835367971 ) ) ;
#27380 = CARTESIAN_POINT ( 'NONE',  ( -2.992535305846383054, -1.816776806824856427, 227.6446713698603617 ) ) ;
#27381 = CARTESIAN_POINT ( 'NONE',  ( 24.68173674080000168, -14.25001227039999918, 226.1000014189999945 ) ) ;
#27382 = CARTESIAN_POINT ( 'NONE',  ( 3.710789578725101734, 2.835545959904678170, -23.36727430110000014 ) ) ;
#27383 = CARTESIAN_POINT ( 'NONE',  ( 25.33584480268815042, 14.29478671867460982, 1.000000000000000888 ) ) ;
#27384 = DIRECTION ( 'NONE',  ( -0.000000000000000000, -0.000000000000000000, -1.000000000000000000 ) ) ;
#27385 = DIRECTION ( 'NONE',  ( 0.000000000000000000, 0.000000000000000000, 1.000000000000000000 ) ) ;
#27386 = ORIENTED_EDGE ( 'NONE', *, *, #24242, .T. ) ;
#27387 = CARTESIAN_POINT ( 'NONE',  ( 23.23277125981546476, 15.26692728828886025, 4.999998581000003384 ) ) ;
#27388 = CARTESIAN_POINT ( 'NONE',  ( 14.94562240850000023, -8.628859120750000500, 5.000000000000000000 ) ) ;
#27389 = VERTEX_POINT ( 'NONE', #17423 ) ;
#27390 = CARTESIAN_POINT ( 'NONE',  ( -26.57440914490000239, -3.469982507400000582, -0.6999999999999992895 ) ) ;
#27391 = CARTESIAN_POINT ( 'NONE',  ( 7.998464191499309983, -115.5020148795422728, 21.10241874685433672 ) ) ;
#27392 = ORIENTED_EDGE ( 'NONE', *, *, #4249, .F. ) ;
#27393 = CARTESIAN_POINT ( 'NONE',  ( -3.928578988383292003, -27.21916582938555251, 20.19379707351126285 ) ) ;
#27394 = VECTOR ( 'NONE', #14056, 1000.000000000000000 ) ;
#27395 = ORIENTED_EDGE ( 'NONE', *, *, #24737, .F. ) ;
#27396 = VERTEX_POINT ( 'NONE', #12550 ) ;
#27397 = SHAPE_REPRESENTATION_RELATIONSHIP ( 'NONE' , 'NONE' ,  #19806, #24185 ) ;
#27398 = ORIENTED_EDGE ( 'NONE', *, *, #22431, .F. ) ;
#27399 = CARTESIAN_POINT ( 'NONE',  ( 0.000000000000000000, 0.000000000000000000, 190.0000000000000000 ) ) ;
#27400 = CARTESIAN_POINT ( 'NONE',  ( -17.59696597926837214, -9.791839085300418688, -0.6999999999999784173 ) ) ;
#27401 = DIRECTION ( 'NONE',  ( -1.000000000000000000, 0.000000000000000000, -2.257144471330000330E-12 ) ) ;
#27402 = DIRECTION ( 'NONE',  ( 1.000000000000000000, 0.000000000000000000, 0.000000000000000000 ) ) ;
#27403 = EDGE_CURVE ( 'NONE', #11023, #29126, #12241, .T. ) ;
#27404 = CARTESIAN_POINT ( 'NONE',  ( -17.83929479963776288, 19.99998902616253105, -0.6999999999999784173 ) ) ;
#27405 = EDGE_CURVE ( 'NONE', #10264, #13631, #24669, .T. ) ;
#27406 = CARTESIAN_POINT ( 'NONE',  ( 8.982833346883268177, -25.99322455654492003, 206.0440937483093649 ) ) ;
#27407 = AXIS2_PLACEMENT_3D ( 'NONE', #16834, #4417, #19359 ) ;
#27408 = CARTESIAN_POINT ( 'NONE',  ( 2.100000000000000089, -1.998401444330000344E-15, 226.6412452697800006 ) ) ;
#27409 = CARTESIAN_POINT ( 'NONE',  ( -4.325159770583737462, -1.744232581393518444, -0.9971974345000036433 ) ) ;
#27410 = CARTESIAN_POINT ( 'NONE',  ( -3.316315296248301792, 4.409923538414076027, -18.63064294430000345 ) ) ;
#27411 = DIRECTION ( 'NONE',  ( 1.000000000000000000, 0.000000000000000000, 0.000000000000000000 ) ) ;
#27412 = CARTESIAN_POINT ( 'NONE',  ( 5.423538825346226666, 5.076873815721838490, -43.29313180051233445 ) ) ;
#27413 = CARTESIAN_POINT ( 'NONE',  ( -2.363020471776699605, -4.627995288602582136, -93.44632962453067648 ) ) ;
#27414 = CARTESIAN_POINT ( 'NONE',  ( -18.87722060250000311, 21.16361474240000007, 229.7625741969999922 ) ) ;
#27415 = CARTESIAN_POINT ( 'NONE',  ( 10.70000000009999930, -27.00000000000000000, -28.39999999989999679 ) ) ;
#27416 = CARTESIAN_POINT ( 'NONE',  ( 5.229687933660000176, -30.84198039109999812, 222.0000000000000000 ) ) ;
#27417 = CARTESIAN_POINT ( 'NONE',  ( -16.06988921231594603, 11.79183908526949054, 0.000000000000000000 ) ) ;
#27418 = CARTESIAN_POINT ( 'NONE',  ( 26.80000000000000071, -3.552713678799999608E-15, 93.21714158839999698 ) ) ;
#27419 = VERTEX_POINT ( 'NONE', #614 ) ;
#27420 = CARTESIAN_POINT ( 'NONE',  ( -3.468517234904579194, -2.575357395510371461, -56.27895058492499913 ) ) ;
#27421 = CARTESIAN_POINT ( 'NONE',  ( -24.90302310912370132, 13.86047864606265279, 6.098655051000018368 ) ) ;
#27422 = CARTESIAN_POINT ( 'NONE',  ( 6.482330152203070739, 0.4632910120546396282, -14.64454535870000207 ) ) ;
#27423 = ORIENTED_EDGE ( 'NONE', *, *, #10636, .F. ) ;
#27424 = SHAPE_REPRESENTATION ( 'Plunger Disc', ( #17722 ), #14824 ) ;
#27425 = CARTESIAN_POINT ( 'NONE',  ( -17.93344248771828475, 20.10553726043776734, 0.000000000000000000 ) ) ;
#27426 = CARTESIAN_POINT ( 'NONE',  ( -4.304922296158920858, 1.087454836608482855, -68.10000000002500542 ) ) ;
#27427 = VERTEX_POINT ( 'NONE', #12864 ) ;
#27428 = ORIENTED_EDGE ( 'NONE', *, *, #13702, .T. ) ;
#27429 = EDGE_CURVE ( 'NONE', #15836, #12111, #12398, .T. ) ;
#27430 = VERTEX_POINT ( 'NONE', #17269 ) ;
#27431 = CARTESIAN_POINT ( 'NONE',  ( 3.388043077353672494, 1.111846212962369629, -88.52261276243450538 ) ) ;
#27432 = ORIENTED_EDGE ( 'NONE', *, *, #11856, .T. ) ;
#27433 = LINE ( 'NONE', #13268, #7915 ) ;
#27434 = B_SPLINE_CURVE_WITH_KNOTS ( 'NONE', 3,
 ( #17951, #8356, #27412, #29621, #5393, #27561 ),
 .UNSPECIFIED., .F., .F.,
 ( 4, 2, 4 ),
 ( 0.000000000000000000, 0.5000000000000000000, 1.000000000000000000 ),
 .UNSPECIFIED. ) ;
#27435 = CARTESIAN_POINT ( 'NONE',  ( -8.000000000030556890, -116.5561065465021784, 18.74526241810166027 ) ) ;
#27436 = CARTESIAN_POINT ( 'NONE',  ( -4.568101251970387189, -0.2431723019811170283, -65.16421022022500154 ) ) ;
#27437 = CARTESIAN_POINT ( 'NONE',  ( -27.09307779329999732, -9.954037724019999089, 229.9751247039999953 ) ) ;
#27438 = DIRECTION ( 'NONE',  ( -1.000000000000000000, -0.000000000000000000, 0.000000000000000000 ) ) ;
#27439 = CARTESIAN_POINT ( 'NONE',  ( -13.00000000000000000, 24.54213077165692525, -59.94572446259928711 ) ) ;
#27440 = DIRECTION ( 'NONE',  ( 0.000000000000000000, 0.9986295347545772749, 0.05233595624287791515 ) ) ;
#27441 = EDGE_LOOP ( 'NONE', ( #27685, #18879, #19333, #24654 ) ) ;
#27442 = CARTESIAN_POINT ( 'NONE',  ( 24.43008698959658176, -14.67811372800087000, 4.492876031999992748 ) ) ;
#27443 = LINE ( 'NONE', #5884, #9995 ) ;
#27444 = ORIENTED_EDGE ( 'NONE', *, *, #6739, .F. ) ;
#27445 = CARTESIAN_POINT ( 'NONE',  ( 24.39498713390000262, -13.33204241800000034, 224.0987054560000047 ) ) ;
#27446 = LINE ( 'NONE', #27297, #14783 ) ;
#27447 = CYLINDRICAL_SURFACE ( 'NONE', #24350, 2.000000000000000000 ) ;
#27448 = CARTESIAN_POINT ( 'NONE',  ( 27.77052805885580966, 0.5052956280425284774, 0.7069222069999991920 ) ) ;
#27449 = CARTESIAN_POINT ( 'NONE',  ( -10.60826873110000079, -24.73114799900000094, -1.605882352700004123 ) ) ;
#27450 = CARTESIAN_POINT ( 'NONE',  ( -5.623491485972666126, 3.092612689740418919, -59.81908057272499946 ) ) ;
#27451 = DIRECTION ( 'NONE',  ( -1.000000000000000000, 0.000000000000000000, 0.000000000000000000 ) ) ;
#27452 = LINE ( 'NONE', #12837, #13766 ) ;
#27453 = ORIENTED_EDGE ( 'NONE', *, *, #13004, .T. ) ;
#27454 = CARTESIAN_POINT ( 'NONE',  ( 23.77307140678977504, -14.41181874416537134, 4.999998581000003384 ) ) ;
#27455 = CARTESIAN_POINT ( 'NONE',  ( 11.69999999989999928, -25.00000000000000000, -2.399999999999999467 ) ) ;
#27456 = EDGE_CURVE ( 'NONE', #26584, #30026, #519, .T. ) ;
#27457 = B_SPLINE_CURVE_WITH_KNOTS ( 'NONE', 3,
 ( #2609, #10161, #268, #24169, #29501, #7486 ),
 .UNSPECIFIED., .F., .F.,
 ( 4, 2, 4 ),
 ( 0.000000000000000000, 0.5000000000000000000, 1.000000000000000000 ),
 .UNSPECIFIED. ) ;
#27458 = CARTESIAN_POINT ( 'NONE',  ( -26.62724484483074150, -3.508068424025498455, 93.21714158835001740 ) ) ;
#27459 = LINE ( 'NONE', #3081, #24868 ) ;
#27460 = EDGE_CURVE ( 'NONE', #7914, #29606, #25608, .T. ) ;
#27461 = CARTESIAN_POINT ( 'NONE',  ( -25.22658730140000216, -13.26242337740000110, 225.0000014190000002 ) ) ;
#27462 = FILL_AREA_STYLE_COLOUR ( '', #1169 ) ;
#27463 = CARTESIAN_POINT ( 'NONE',  ( 11.20000000009999930, -22.00000000000000000, -25.51324865394999719 ) ) ;
#27464 = CARTESIAN_POINT ( 'NONE',  ( 2.760998891309374148, 1.965471783823139473, -41.77559963342530125 ) ) ;
#27465 = CARTESIAN_POINT ( 'NONE',  ( 2.637655088286928962, -3.673227524439524050, -61.52197827312500067 ) ) ;
#27466 = ORIENTED_EDGE ( 'NONE', *, *, #30961, .T. ) ;
#27467 = CARTESIAN_POINT ( 'NONE',  ( 18.25326690153244513, 20.00000274250295718, 230.6772558227679042 ) ) ;
#27468 = EDGE_LOOP ( 'NONE', ( #23030, #23769, #295, #6343, #7845, #12311, #3427, #3940 ) ) ;
#27469 = CARTESIAN_POINT ( 'NONE',  ( 27.98121187870611593, -9.706323496128696604, 0.8585786439999909536 ) ) ;
#27470 = ORIENTED_EDGE ( 'NONE', *, *, #5836, .F. ) ;
#27471 = ADVANCED_FACE ( 'NONE', ( #8757 ), #7740, .T. ) ;
#27472 = CARTESIAN_POINT ( 'NONE',  ( -12.30000000006999805, -24.00000000000000000, -28.40000000020000215 ) ) ;
#27473 = CARTESIAN_POINT ( 'NONE',  ( -18.95046173579999760, -18.95046173579999760, 136.7828584120000244 ) ) ;
#27474 = CARTESIAN_POINT ( 'NONE',  ( 17.83931306984926835, 20.00000000000176570, -0.6999999999999784173 ) ) ;
#27475 = CARTESIAN_POINT ( 'NONE',  ( 24.63375101535647360, -12.88633855010671247, 5.901400366999986602 ) ) ;
#27476 = CARTESIAN_POINT ( 'NONE',  ( -1.100001419170000050, -27.77850706310000106, 225.0000014190000002 ) ) ;
#27477 = VERTEX_POINT ( 'NONE', #23097 ) ;
#27478 = CARTESIAN_POINT ( 'NONE',  ( -8.000000000477658801, -25.77531388886969310, -25.66136093485691916 ) ) ;
#27479 = CARTESIAN_POINT ( 'NONE',  ( 27.04041630560000087, -5.217841840389998853E-14, 230.6999999999999886 ) ) ;
#27480 = AXIS2_PLACEMENT_3D ( 'NONE', #19244, #2417, #16876 ) ;
#27481 = CARTESIAN_POINT ( 'NONE',  ( 5.972505199797514486, -1.290950946386169917, -23.79036215650000230 ) ) ;
#27482 = CARTESIAN_POINT ( 'NONE',  ( 7.105427357599999217E-15, 3.552713678799999608E-15, 93.60555127549999099 ) ) ;
#27483 = CARTESIAN_POINT ( 'NONE',  ( 0.000000000000000000, 0.000000000000000000, 190.0000000000000000 ) ) ;
#27484 = AXIS2_PLACEMENT_3D ( 'NONE', #11823, #10082, #7401 ) ;
#27485 = LINE ( 'NONE', #24831, #17644 ) ;
#27486 = DIRECTION ( 'NONE',  ( -1.000000000000000000, 5.665498452320000818E-16, 0.000000000000000000 ) ) ;
#27487 = CARTESIAN_POINT ( 'NONE',  ( -3.099154212379724882, 4.549648463301534385, -47.25391720692500286 ) ) ;
#27488 = CARTESIAN_POINT ( 'NONE',  ( 17.16657240421717390, -9.000000000001264766, -0.6999999999999784173 ) ) ;
#27489 = CARTESIAN_POINT ( 'NONE',  ( 2.373622499810743136, -26.70000180411620505, 210.0000000000000284 ) ) ;
#27490 = CARTESIAN_POINT ( 'NONE',  ( -10.69999999999893703, -28.46561708982691030, -25.75493691888135572 ) ) ;
#27491 = PLANE ( 'NONE',  #2763 ) ;
#27492 = EDGE_CURVE ( 'NONE', #25227, #12548, #23247, .T. ) ;
#27493 = CARTESIAN_POINT ( 'NONE',  ( 0.5184513693225726305, -28.49550581263314086, 6.099998581000020792 ) ) ;
#27494 = B_SPLINE_CURVE_WITH_KNOTS ( 'NONE', 5,
 ( #17838, #24783, #15340, #10931, #5735, #24938 ),
 .UNSPECIFIED., .F., .F.,
 ( 6, 6 ),
 ( -2.319814960320000008, 0.000000000000000000 ),
 .UNSPECIFIED. ) ;
#27495 = ORIENTED_EDGE ( 'NONE', *, *, #4104, .F. ) ;
#27496 = CARTESIAN_POINT ( 'NONE',  ( -3.910239773549598397, 2.823051725158805425, -35.40446136359998519 ) ) ;
#27497 = VECTOR ( 'NONE', #9097, 1000.000000000000114 ) ;
#27498 = EDGE_LOOP ( 'NONE', ( #29721, #11224, #31, #7879 ) ) ;
#27499 = CARTESIAN_POINT ( 'NONE',  ( -8.699999999674142614, -13.61360970150653316, -34.64062719139432289 ) ) ;
#27500 = CARTESIAN_POINT ( 'NONE',  ( 4.894650655971835462, -0.3620128515310818140, -49.87442242802501369 ) ) ;
#27501 = ORIENTED_EDGE ( 'NONE', *, *, #19030, .T. ) ;
#27502 = ITEM_DEFINED_TRANSFORMATION ( 'NONE', 'NONE', #26409,  #17722 ) ;
#27503 = ORIENTED_EDGE ( 'NONE', *, *, #18161, .T. ) ;
#27504 = CIRCLE ( 'NONE', #5900, 2.000000000000000000 ) ;
#27505 = ORIENTED_EDGE ( 'NONE', *, *, #12854, .F. ) ;
#27506 = CARTESIAN_POINT ( 'NONE',  ( 24.05769993097482029, 13.93129956292569638, 3.997248600000002927 ) ) ;
#27507 = CARTESIAN_POINT ( 'NONE',  ( 10.00000000000000000, 21.70000000000000284, -60.10000000000000142 ) ) ;
#27508 = CARTESIAN_POINT ( 'NONE',  ( -10.69999999999999929, 19.99999999999999645, -22.39999999999999858 ) ) ;
#27509 = EDGE_CURVE ( 'NONE', #4659, #8882, #6901, .T. ) ;
#27510 = B_SPLINE_CURVE_WITH_KNOTS ( 'NONE', 3,
 ( #2227, #28335, #26603, #23947, #6784, #12118, #21261, #26, #21726, #26449, #26143, #9609, #7094, #14651, #24093, #16380, #19207, #26292, #2070, #31013, #2681, #25987, #24236, #2383, #23634, #19052, #178, #30862, #28650, #28494, #4893, #11661, #9294, #28792, #5041, #4427, #18897, #16682, #14030, #4736, #4576, #9762, #19368, #28958 ),
 .UNSPECIFIED., .F., .F.,
 ( 4, 2, 2, 1, 2, 2, 2, 2, 1, 1, 2, 2, 2, 2, 1, 1, 1, 2, 2, 2, 2, 1, 1, 2, 2, 4 ),
 ( 0.000000000000000000, 0.06250000000003701206, 0.09375000000005716261, 0.1093750000000685701, 0.1171875000000742878, 0.1250000000000799916, 0.1875000000001231792, 0.2187500000001463274, 0.2343750000001579292, 0.2421875000001617317, 0.2460937500001615930, 0.2500000000001614264, 0.3750000000001613154, 0.4375000000001627587, 0.4687500000001635359, 0.4843750000001654787, 0.4921875000001664779, 0.4960937500001669220, 0.5000000000001674216, 0.6250000000001194600, 0.6875000000000943690, 0.7187500000000829337, 0.7343750000000781597, 0.7421875000000758282, 0.7500000000000733857, 1.000000000000000000 ),
 .UNSPECIFIED. ) ;
#27511 = CARTESIAN_POINT ( 'NONE',  ( 353532.1637640000554, 353526.3905929999892, -28.40000001513906724 ) ) ;
#27512 = CARTESIAN_POINT ( 'NONE',  ( -24.49999999589999788, 3.000285566369999841E-15, 40.00000000000000000 ) ) ;
#27513 = EDGE_CURVE ( 'NONE', #5832, #10448, #24523, .T. ) ;
#27514 = CARTESIAN_POINT ( 'NONE',  ( -3.762209872552725543, 2.386954303616800388, -0.6999999999999992895 ) ) ;
#27515 = CARTESIAN_POINT ( 'NONE',  ( -1.763726019828893321, -5.203278105301040846, 0.4243694872999951850 ) ) ;
#27516 = CARTESIAN_POINT ( 'NONE',  ( 11.26179938798771474, 26.42151601322854759, -59.26168417594740134 ) ) ;
#27517 = CARTESIAN_POINT ( 'NONE',  ( -20.30403093128963476, 20.00000000003735323, 3.000000106999994642 ) ) ;
#27518 = EDGE_CURVE ( 'NONE', #30584, #4237, #13652, .T. ) ;
#27519 = CARTESIAN_POINT ( 'NONE',  ( 4.310466091822805268, 1.786666325167808544, -11.49261350019999739 ) ) ;
#27520 = CARTESIAN_POINT ( 'NONE',  ( 0.07512830594655582617, -4.346272141329937888, -32.91110030500001216 ) ) ;
#27521 = VECTOR ( 'NONE', #30590, 1000.000000000000000 ) ;
#27522 = CYLINDRICAL_SURFACE ( 'NONE', #20212, 27.50000000000000000 ) ;
#27523 = DIRECTION ( 'NONE',  ( 0.000000000000000000, 0.000000000000000000, -1.000000000000000000 ) ) ;
#27524 = CARTESIAN_POINT ( 'NONE',  ( -28.35945636601969611, -7.983396444588293228, 8.000000000000007105 ) ) ;
#27525 = CARTESIAN_POINT ( 'NONE',  ( 0.3737937747469999850, -27.79795631750000240, 226.0423291289999952 ) ) ;
#27526 = CARTESIAN_POINT ( 'NONE',  ( 3.375516224911112584, -2.766870103071181308, -23.99674734060000603 ) ) ;
#27527 = AXIS2_PLACEMENT_3D ( 'NONE', #7919, #18141, #25401 ) ;
#27528 = CARTESIAN_POINT ( 'NONE',  ( 18.87721748640135644, 21.16361474300574841, 0.2374258030000131470 ) ) ;
#27529 = CARTESIAN_POINT ( 'NONE',  ( -8.699999999668968087, -13.49637763710977900, -34.94770709601201020 ) ) ;
#27530 = CARTESIAN_POINT ( 'NONE',  ( -7.428071722523742260, -8.043573579563092935, -36.89386202926774416 ) ) ;
#27532 = EDGE_CURVE ( 'NONE', #17862, #6732, #12779, .T. ) ;
#27531 = TOROIDAL_SURFACE ( 'NONE', #5414, 29.80000000000000071, 3.000000000000000000 ) ;
#27533 = ORIENTED_EDGE ( 'NONE', *, *, #29066, .F. ) ;
#27534 = EDGE_LOOP ( 'NONE', ( #18109, #11384, #18578, #8221 ) ) ;
#27535 = B_SPLINE_CURVE_WITH_KNOTS ( 'NONE', 4,
 ( #25519, #3956, #23161, #1602, #11192 ),
 .UNSPECIFIED., .F., .F.,
 ( 5, 5 ),
 ( -0.9817477042469999748, 0.9817477042469999748 ),
 .UNSPECIFIED. ) ;
#27536 = EDGE_CURVE ( 'NONE', #26442, #5618, #1221, .T. ) ;
#27537 = CARTESIAN_POINT ( 'NONE',  ( 8.699999999502342263, -25.77531388888509056, -25.66136093477824431 ) ) ;
#27538 = LINE ( 'NONE', #817, #3697 ) ;
#27539 = EDGE_LOOP ( 'NONE', ( #977, #15246, #9012, #7759 ) ) ;
#27540 = CARTESIAN_POINT ( 'NONE',  ( 6.585786437629999490, -16.41511111490214603, -74.85294138696069410 ) ) ;
#27541 = CARTESIAN_POINT ( 'NONE',  ( 9.000000000000000000, -130.0000000000000000, -42.39999999999999858 ) ) ;
#27542 = VERTEX_POINT ( 'NONE', #6082 ) ;
#27543 = CARTESIAN_POINT ( 'NONE',  ( -3.160606383828813204, -27.32265456628853784, 20.04828141274519027 ) ) ;
#27544 = ORIENTED_EDGE ( 'NONE', *, *, #16389, .F. ) ;
#27545 = EDGE_CURVE ( 'NONE', #25546, #21137, #30376, .T. ) ;
#27546 = EDGE_LOOP ( 'NONE', ( #12104, #15601, #27694, #2591, #4107, #7686, #16905, #6039 ) ) ;
#27547 = AXIS2_PLACEMENT_3D ( 'NONE', #8790, #16034, #3294 ) ;
#27548 = SURFACE_SIDE_STYLE ('',( #25192 ) ) ;
#27549 = ORIENTED_EDGE ( 'NONE', *, *, #22367, .T. ) ;
#27550 = CARTESIAN_POINT ( 'NONE',  ( 26.80000000000000071, 4.525613202489999765, 230.6999999999999886 ) ) ;
#27551 = CARTESIAN_POINT ( 'NONE',  ( -7.861312627696711353, 6.462009008233210672, -40.63090155204401555 ) ) ;
#27552 = CARTESIAN_POINT ( 'NONE',  ( 10.69999999999999929, 19.99999999999999645, -22.39999999999999858 ) ) ;
#27553 = SURFACE_STYLE_FILL_AREA ( #10574 ) ;
#27554 = CARTESIAN_POINT ( 'NONE',  ( -24.37451445311242892, 13.36962324138351299, 6.095967861000000987 ) ) ;
#27555 = CARTESIAN_POINT ( 'NONE',  ( -0.6094664100040195764, -28.49364619262437870, 4.999998581000003384 ) ) ;
#27556 = VECTOR ( 'NONE', #13325, 1000.000000000000114 ) ;
#27557 = CARTESIAN_POINT ( 'NONE',  ( -0.03526712872429999673, -28.50022367440000082, 226.1000014189999945 ) ) ;
#27558 = CARTESIAN_POINT ( 'NONE',  ( 0.5877407897813130555, -4.297347728519515186, -0.3731240480000022619 ) ) ;
#27559 = CARTESIAN_POINT ( 'NONE',  ( -1.058439502263211374, 6.005994971325610443, -19.23583244400001036 ) ) ;
#27560 = CARTESIAN_POINT ( 'NONE',  ( -17.62526668112344908, -8.236461616547455122, -0.6999999999999784173 ) ) ;
#27561 = CARTESIAN_POINT ( 'NONE',  ( 6.760007715859396527, 4.357143524031256376, -42.94209588227683128 ) ) ;
#27562 = CARTESIAN_POINT ( 'NONE',  ( 3.181902231748806376, -1.609514238137543796, -88.52261276306772686 ) ) ;
#27563 = CARTESIAN_POINT ( 'NONE',  ( -26.32808186270000306, 9.205804489829999326, 230.6577119970000069 ) ) ;
#27564 = LINE ( 'NONE', #10163, #5734 ) ;
#27565 = CARTESIAN_POINT ( 'NONE',  ( -23.74292845506526461, -13.87604159535428927, 223.8999999999999773 ) ) ;
#27566 = VECTOR ( 'NONE', #724, 1000.000000000000114 ) ;
#27567 = DIRECTION ( 'NONE',  ( 1.000000000000000000, 0.000000000000000000, 0.000000000000000000 ) ) ;
#27568 = CARTESIAN_POINT ( 'NONE',  ( 21.73374413810000050, -15.98809491730000154, 230.6999999999999886 ) ) ;
#27569 = LINE ( 'NONE', #29776, #12795 ) ;
#27570 = EDGE_CURVE ( 'NONE', #1526, #20656, #6241, .T. ) ;
#27571 = ORIENTED_EDGE ( 'NONE', *, *, #29945, .F. ) ;
#27572 = CARTESIAN_POINT ( 'NONE',  ( 3.567773119718944397, 3.614166260817118559, -56.95805965152499084 ) ) ;
#27573 = CARTESIAN_POINT ( 'NONE',  ( -8.699999999655181782, -13.66682223737418944, -36.55330428419230060 ) ) ;
#27574 = ORIENTED_EDGE ( 'NONE', *, *, #23939, .T. ) ;
#27575 = EDGE_CURVE ( 'NONE', #4259, #3218, #1376, .T. ) ;
#27576 = CARTESIAN_POINT ( 'NONE',  ( -6.277996069133942925, 1.777976852108807737, -7.310827254900003069 ) ) ;
#27577 = ORIENTED_EDGE ( 'NONE', *, *, #21723, .F. ) ;
#27578 = EDGE_CURVE ( 'NONE', #16829, #17637, #5727, .T. ) ;
#27579 = DIRECTION ( 'NONE',  ( -0.4353787270609792981, -0.9002473904559574747, 0.000000000000000000 ) ) ;
#27580 = AXIS2_PLACEMENT_3D ( 'NONE', #3731, #13330, #22939 ) ;
#27581 = CARTESIAN_POINT ( 'NONE',  ( -4.041264224475901834, -0.4991584895587213300, -68.10000000002499121 ) ) ;
#27582 = EDGE_CURVE ( 'NONE', #18237, #20880, #3889, .T. ) ;
#27583 = ORIENTED_EDGE ( 'NONE', *, *, #15967, .T. ) ;
#27584 = VERTEX_POINT ( 'NONE', #20892 ) ;
#27585 = VERTEX_POINT ( 'NONE', #14114 ) ;
#27586 = CARTESIAN_POINT ( 'NONE',  ( -2.020725942269999909, -3.500000000000000000, 227.9588918784999976 ) ) ;
#27587 =( NAMED_UNIT ( * ) PLANE_ANGLE_UNIT ( ) SI_UNIT ( $, .RADIAN. ) );
#27588 = ORIENTED_EDGE ( 'NONE', *, *, #24497, .F. ) ;
#27589 = CARTESIAN_POINT ( 'NONE',  ( -24.88589369081283920, 13.89120818323882922, 3.904029272000009154 ) ) ;
#27590 = CARTESIAN_POINT ( 'NONE',  ( -8.699999999628365899, -17.59709758660007139, -40.94395633085227360 ) ) ;
#27591 = CARTESIAN_POINT ( 'NONE',  ( -2.911316102855189492, -3.927725552494646166, -64.73409070562500744 ) ) ;
#27592 = CARTESIAN_POINT ( 'NONE',  ( 1.360000222151617422, -28.46784699774883975, 5.735069644430439872 ) ) ;
#27593 = TOROIDAL_SURFACE ( 'NONE', #5980, 29.80000000000000071, 3.000000000000000000 ) ;
#27594 = CARTESIAN_POINT ( 'NONE',  ( -22.62479587716747886, 18.00962536160662708, 0.7595836940000044724 ) ) ;
#27595 = DIRECTION ( 'NONE',  ( 0.000000000000000000, 0.000000000000000000, 1.000000000000000000 ) ) ;
#27596 = CARTESIAN_POINT ( 'NONE',  ( -23.73450314257943816, -12.44732035342869203, 5.218051572315431486 ) ) ;
#27597 = CARTESIAN_POINT ( 'NONE',  ( 0.000000000000000000, 0.000000000000000000, 115.0000000000000000 ) ) ;
#27598 = VERTEX_POINT ( 'NONE', #4516 ) ;
#27599 = AXIS2_PLACEMENT_3D ( 'NONE', #15172, #27595, #3361 ) ;
#27600 = CARTESIAN_POINT ( 'NONE',  ( -5.530047734074942767, 3.478668956039820959, -9.845475902800000512 ) ) ;
#27601 = CARTESIAN_POINT ( 'NONE',  ( 24.52721838744982463, -14.51532614974687796, 4.239732040000027347 ) ) ;
#27602 = CARTESIAN_POINT ( 'NONE',  ( 5.797918471924832673, -115.0360660102050048, 22.14437208032004989 ) ) ;
#27603 = ORIENTED_EDGE ( 'NONE', *, *, #19093, .F. ) ;
#27604 = CARTESIAN_POINT ( 'NONE',  ( 25.22625794089999829, -13.26224522399999906, 225.0000014190000002 ) ) ;
#27605 = CARTESIAN_POINT ( 'NONE',  ( -22.63992238021891978, -14.34133587286723710, 4.902940995466560814 ) ) ;
#27606 = B_SPLINE_CURVE_WITH_KNOTS ( 'NONE', 3,
 ( #12945, #1305, #5547, #27112, #18118, #20181, #997, #10587, #3646, #8517 ),
 .UNSPECIFIED., .F., .F.,
 ( 4, 2, 2, 2, 4 ),
 ( 0.000000000000000000, 0.2500000000000000000, 0.5000000000000000000, 0.7500000000000000000, 1.000000000000000000 ),
 .UNSPECIFIED. ) ;
#27607 = CARTESIAN_POINT ( 'NONE',  ( 27.71196445724500990, 5.091237891590008502, 1.000000000000000888 ) ) ;
#27608 = CARTESIAN_POINT ( 'NONE',  ( 5.925978784015399903, -0.8792241758803844842, -46.13818262062499542 ) ) ;
#27609 = LINE ( 'NONE', #20221, #11723 ) ;
#27610 = CYLINDRICAL_SURFACE ( 'NONE', #19811, 3.000000000000002220 ) ;
#27611 = VERTEX_POINT ( 'NONE', #21192 ) ;
#27612 = DIRECTION ( 'NONE',  ( 0.000000000000000000, 0.000000000000000000, 1.000000000000000000 ) ) ;
#27613 = CARTESIAN_POINT ( 'NONE',  ( 25.26809612939999994, 12.77001324749999966, 224.8000000000000114 ) ) ;
#27614 = DIRECTION ( 'NONE',  ( 0.000000000000000000, 0.000000000000000000, 1.000000000000000000 ) ) ;
#27615 = CARTESIAN_POINT ( 'NONE',  ( -9.000000000000000000, 21.69999999998272244, -51.75635761556686987 ) ) ;
#27616 = CARTESIAN_POINT ( 'NONE',  ( -24.28117756982639364, -12.91036561269763716, 225.5561643545236734 ) ) ;
#27617 = B_SPLINE_CURVE_WITH_KNOTS ( 'NONE', 3,
 ( #23596, #18061, #16027, #25795, #18219, #21072, #10848, #4230, #13670, #30357, #13510, #1566, #13830, #27827, #18542, #8944, #6430, #1719, #23443, #30032 ),
 .UNSPECIFIED., .F., .F.,
 ( 4, 1, 1, 1, 2, 2, 2, 1, 1, 1, 2, 2, 4 ),
 ( 0.000000000000000000, 0.1250000000000007494, 0.1875000000000013600, 0.2187500000000012212, 0.2343750000000005829, 0.2499999999999999167, 0.5000000000000047740, 0.6250000000000075495, 0.6875000000000081046, 0.7187500000000083267, 0.7343750000000085487, 0.7500000000000087708, 1.000000000000000000 ),
 .UNSPECIFIED. ) ;
#27618 = AXIS2_PLACEMENT_3D ( 'NONE', #4035, #15247, #13632 ) ;
#27619 = CARTESIAN_POINT ( 'NONE',  ( 14.81448010921499225, -25.26807234752766718, -33.17346377528555479 ) ) ;
#27620 = DIRECTION ( 'NONE',  ( 1.000000000000000000, 0.000000000000000000, 0.000000000000000000 ) ) ;
#27621 = CARTESIAN_POINT ( 'NONE',  ( -1.143212971672622036, -4.711439499498762729, -61.94311227092499195 ) ) ;
#27622 = ORIENTED_EDGE ( 'NONE', *, *, #2660, .T. ) ;
#27623 = CARTESIAN_POINT ( 'NONE',  ( 20.08457158244946683, 19.99997717933547392, 229.7115254020307020 ) ) ;
#27624 = ORIENTED_EDGE ( 'NONE', *, *, #3481, .F. ) ;
#27625 = CARTESIAN_POINT ( 'NONE',  ( 14.11260095516644242, -27.08984601216539190, 0.2686766510000271335 ) ) ;
#27626 = ORIENTED_EDGE ( 'NONE', *, *, #16774, .T. ) ;
#27627 = EDGE_CURVE ( 'NONE', #21618, #30015, #28973, .T. ) ;
#27628 = FACE_OUTER_BOUND ( 'NONE', #25564, .T. ) ;
#27629 = CARTESIAN_POINT ( 'NONE',  ( -3.458129700889219116, 0.5397582531354577773, -88.52261276322501260 ) ) ;
#27630 = FACE_OUTER_BOUND ( 'NONE', #29686, .T. ) ;
#27631 = DIRECTION ( 'NONE',  ( 0.000000000000000000, 0.000000000000000000, -1.000000000000000000 ) ) ;
#27632 = B_SPLINE_CURVE_WITH_KNOTS ( 'NONE', 3,
 ( #123, #2477, #2327, #26087, #11909, #21826 ),
 .UNSPECIFIED., .F., .F.,
 ( 4, 2, 4 ),
 ( 0.000000000000000000, 0.5000000000000000000, 1.000000000000000000 ),
 .UNSPECIFIED. ) ;
#27633 = CARTESIAN_POINT ( 'NONE',  ( -8.881784197000000993E-16, 2.220446049249999755E-16, 227.6412452699999847 ) ) ;
#27634 = LINE ( 'NONE', #6079, #3973 ) ;
#27635 = ORIENTED_EDGE ( 'NONE', *, *, #7956, .F. ) ;
#27636 = CARTESIAN_POINT ( 'NONE',  ( 20.77600629932058851, 21.68409807857665683, 8.000000000000007105 ) ) ;
#27637 = DIRECTION ( 'NONE',  ( 1.000000000000000000, -1.224606353819999829E-16, 0.000000000000000000 ) ) ;
#27638 = EDGE_CURVE ( 'NONE', #5034, #3507, #9542, .T. ) ;
#27639 = CARTESIAN_POINT ( 'NONE',  ( -6.771817672307487435, -16.24036849850417141, -74.78934027593398071 ) ) ;
#27640 = VECTOR ( 'NONE', #21247, 1000.000000000000000 ) ;
#27641 = CARTESIAN_POINT ( 'NONE',  ( -8.699999999715885224, -26.99999999997790923, -28.40000000002690683 ) ) ;
#27642 = LINE ( 'NONE', #8917, #28732 ) ;
#27643 = LINE ( 'NONE', #20249, #27069 ) ;
#27644 = CARTESIAN_POINT ( 'NONE',  ( 9.999999999971771913, -24.07808197008955631, -29.18524365354899075 ) ) ;
#27645 = CARTESIAN_POINT ( 'NONE',  ( -17.92947097108555354, 10.82847174396546741, -1.400000000000001910 ) ) ;
#27646 = CARTESIAN_POINT ( 'NONE',  ( 4.416651415012724513, -2.079980245798425109, -51.54872167392500870 ) ) ;
#27647 = DIRECTION ( 'NONE',  ( 1.000000000000000000, 0.000000000000000000, 0.000000000000000000 ) ) ;
#27648 = PRODUCT_DEFINITION_SHAPE ( 'NONE', 'NONE',  #26933 ) ;
#27649 = CARTESIAN_POINT ( 'NONE',  ( 2.220446049249999755E-16, 2.100000000000000089, 226.6412452697800006 ) ) ;
#27650 = LINE ( 'NONE', #2016, #9287 ) ;
#27651 = FACE_OUTER_BOUND ( 'NONE', #28599, .T. ) ;
#27652 = CARTESIAN_POINT ( 'NONE',  ( -1.583312407113587339, 1.386473476258559545, 226.6412452697800006 ) ) ;
#27653 = VERTEX_POINT ( 'NONE', #21044 ) ;
#27654 = CARTESIAN_POINT ( 'NONE',  ( 2.561732861602287858, -4.873875974281082435, -34.20721934060000535 ) ) ;
#27655 = ORIENTED_EDGE ( 'NONE', *, *, #15676, .T. ) ;
#27656 = ADVANCED_FACE ( 'NONE', ( #18665 ), #9373, .F. ) ;
#27657 = DIRECTION ( 'NONE',  ( 5.962915006522623408E-16, 0.4383711467890811231, 0.8987940462991652613 ) ) ;
#27658 = CARTESIAN_POINT ( 'NONE',  ( 1.423503787547387933, 4.651298240777052229, -52.21125421252499876 ) ) ;
#27659 = ORIENTED_EDGE ( 'NONE', *, *, #24428, .F. ) ;
#27660 = B_SPLINE_CURVE_WITH_KNOTS ( 'NONE', 1,
 ( #1611, #23170 ),
 .UNSPECIFIED., .F., .F.,
 ( 2, 2 ),
 ( -0.7000000000009999335, 0.002002273571169999045 ),
 .UNSPECIFIED. ) ;
#27661 = VERTEX_POINT ( 'NONE', #30644 ) ;
#27662 =( REPRESENTATION_RELATIONSHIP ('NONE','NONE', #2712, #22833 ) REPRESENTATION_RELATIONSHIP_WITH_TRANSFORMATION ( #22955 )SHAPE_REPRESENTATION_RELATIONSHIP( ) );
#27663 = VERTEX_POINT ( 'NONE', #30948 ) ;
#27664 = FACE_OUTER_BOUND ( 'NONE', #14048, .T. ) ;
#27665 = CARTESIAN_POINT ( 'NONE',  ( -0.3176897050407275214, -27.79840873693312631, 5.732747703400294270 ) ) ;
#27666 = CARTESIAN_POINT ( 'NONE',  ( -9.707106781189999367, -130.0000000000000000, -43.10710678118599759 ) ) ;
#27667 = CIRCLE ( 'NONE', #9600, 26.80000000000000071 ) ;
#27668 = CARTESIAN_POINT ( 'NONE',  ( -27.79539923781770483, -0.5057481688778130424, 0.8585786439999909536 ) ) ;
#27669 = DIRECTION ( 'NONE',  ( 2.256480420250000087E-12, -0.000000000000000000, -1.000000000000000000 ) ) ;
#27670 = CARTESIAN_POINT ( 'NONE',  ( -3.754118416966668814, 2.080634641777292071, -0.6999999999999992895 ) ) ;
#27671 = CARTESIAN_POINT ( 'NONE',  ( 3.691964249065762260, -4.599677940684276933, -2.105321867100004685 ) ) ;
#27672 = CARTESIAN_POINT ( 'NONE',  ( -10.00000000057842087, -30.00000000000020606, -28.79269908169879955 ) ) ;
#27673 = DIRECTION ( 'NONE',  ( -0.8329895880221872551, 0.5532886644841250590, 0.000000000000000000 ) ) ;
#27674 = EDGE_CURVE ( 'NONE', #17360, #10417, #5342, .T. ) ;
#27675 = CARTESIAN_POINT ( 'NONE',  ( -1.657635364023947400, -6.345118362804027079, -13.15022317840000632 ) ) ;
#27676 = CARTESIAN_POINT ( 'NONE',  ( 4.198532171030673332, 1.238783022246746413, -35.53159726780000227 ) ) ;
#27677 = CARTESIAN_POINT ( 'NONE',  ( 1.094484693600000114, -5.799375430310000468, 226.6412452697800006 ) ) ;
#27678 = PLANE ( 'NONE',  #29300 ) ;
#27679 = CARTESIAN_POINT ( 'NONE',  ( -26.57440607989999748, -3.469982107200002108, -1.399999999999998579 ) ) ;
#27680 = FACE_OUTER_BOUND ( 'NONE', #9165, .T. ) ;
#27681 = CARTESIAN_POINT ( 'NONE',  ( -17.30852986267844429, -27.88015086496476158, -33.66534735328443873 ) ) ;
#27682 = CARTESIAN_POINT ( 'NONE',  ( 22.44263053747149783, 18.11531079112418752, 0.5017677510000262409 ) ) ;
#27683 = CARTESIAN_POINT ( 'NONE',  ( 8.903108651239925564, -22.82508830966962421, 90.00000000000000000 ) ) ;
#27684 = CARTESIAN_POINT ( 'NONE',  ( 21.02336020643863179, 19.26966202639587067, 4.000000000000003553 ) ) ;
#27685 = ORIENTED_EDGE ( 'NONE', *, *, #11367, .F. ) ;
#27686 = EDGE_CURVE ( 'NONE', #6309, #1290, #2005, .T. ) ;
#27687 = EDGE_CURVE ( 'NONE', #19467, #27946, #8331, .T. ) ;
#27688 = FACE_OUTER_BOUND ( 'NONE', #2863, .T. ) ;
#27689 =( GEOMETRIC_REPRESENTATION_CONTEXT ( 3 ) GLOBAL_UNCERTAINTY_ASSIGNED_CONTEXT ( ( #15034 ) ) GLOBAL_UNIT_ASSIGNED_CONTEXT ( ( #5971, #656, #15720 ) ) REPRESENTATION_CONTEXT ( 'NONE', 'WORKASPACE' ) );
#27690 = ORIENTED_EDGE ( 'NONE', *, *, #12377, .T. ) ;
#27691 = DIRECTION ( 'NONE',  ( -5.962915006522622422E-16, -0.4383711467890810676, -0.8987940462991651502 ) ) ;
#27692 = CARTESIAN_POINT ( 'NONE',  ( 3.763816007347946968, -0.7100252077446855825, -37.13286673860216069 ) ) ;
#27693 = CARTESIAN_POINT ( 'NONE',  ( 0.4946794151854280730, -26.79522481891638108, 4.006804116327493226 ) ) ;
#27694 = ORIENTED_EDGE ( 'NONE', *, *, #30349, .T. ) ;
#27695 = CARTESIAN_POINT ( 'NONE',  ( 27.23548387180000319, -3.335274659869999873E-15, 91.66046017409999536 ) ) ;
#27696 = EDGE_LOOP ( 'NONE', ( #9157, #2995, #13036, #22373, #14887 ) ) ;
#27697 = ORIENTED_EDGE ( 'NONE', *, *, #24207, .T. ) ;
#27698 = EDGE_CURVE ( 'NONE', #25870, #24116, #20294, .T. ) ;
#27699 = ORIENTED_EDGE ( 'NONE', *, *, #11880, .T. ) ;
#27700 = CARTESIAN_POINT ( 'NONE',  ( -1.015151870899999809, -28.48229306780000059, 224.4935097720000101 ) ) ;
#27701 = ORIENTED_EDGE ( 'NONE', *, *, #27753, .T. ) ;
#27702 = CARTESIAN_POINT ( 'NONE',  ( -24.39524108160000182, -13.33235248870000156, 225.9014032059999977 ) ) ;
#27703 = ORIENTED_EDGE ( 'NONE', *, *, #8777, .T. ) ;
#27704 = CARTESIAN_POINT ( 'NONE',  ( -24.34138990045594042, 13.42981243766085164, 6.099998581000020792 ) ) ;
#27705 = CARTESIAN_POINT ( 'NONE',  ( -5.415640807596865614, 6.430466356693489871, -40.61551717295832731 ) ) ;
#27706 = EDGE_CURVE ( 'NONE', #27907, #23432, #28799, .T. ) ;
#27707 = CARTESIAN_POINT ( 'NONE',  ( -7.291979204152452709, -5.587697461206379224, -27.06041739756416931 ) ) ;
#27708 = CARTESIAN_POINT ( 'NONE',  ( 2.020725942159999899, -3.500000000000000000, 227.9588918784999976 ) ) ;
#27709 = CARTESIAN_POINT ( 'NONE',  ( 3.550686850769999806E-05, -28.50022181210000127, 226.1000014189999945 ) ) ;
#27710 = VERTEX_POINT ( 'NONE', #11442 ) ;
#27711 = VECTOR ( 'NONE', #2320, 1000.000000000000000 ) ;
#27712 = CARTESIAN_POINT ( 'NONE',  ( -1.949381390262891589, -5.750991590113663676, -0.5756305127000010957 ) ) ;
#27713 = CARTESIAN_POINT ( 'NONE',  ( -2.258375515291465963, 5.046176096958239654, -21.73780126170000671 ) ) ;
#27714 = CARTESIAN_POINT ( 'NONE',  ( -7.379546049855178147, -26.49401563815923666, 208.0614364002278478 ) ) ;
#27715 = CARTESIAN_POINT ( 'NONE',  ( 25.22625794089999829, -13.26224522399999906, 225.0000014190000002 ) ) ;
#27716 = VECTOR ( 'NONE', #16711, 1000.000000000000000 ) ;
#27717 = B_SPLINE_CURVE_WITH_KNOTS ( 'NONE', 5,
 ( #30328, #1847, #16314, #18667, #9222, #18981, #2159, #21194, #4663, #9693, #26225, #28731 ),
 .UNSPECIFIED., .F., .F.,
 ( 6, 3, 3, 6 ),
 ( 1.224410044450000123, 1.456395030499999965, 2.184590855310000190, 2.448622034100000011 ),
 .UNSPECIFIED. ) ;
#27718 = CARTESIAN_POINT ( 'NONE',  ( -27.76135143710000008, 3.399672736049999681E-15, 137.6614141009999912 ) ) ;
#27719 = CARTESIAN_POINT ( 'NONE',  ( -27.56257419730000180, 4.647474305650000304, 230.5592437530000041 ) ) ;
#27720 = CIRCLE ( 'NONE', #18171, 2.000000000000000000 ) ;
#27721 = DIRECTION ( 'NONE',  ( 1.000000000000000000, 0.000000000000000000, 0.000000000000000000 ) ) ;
#27722 = CARTESIAN_POINT ( 'NONE',  ( -24.05864279069999867, -13.92996648929999992, 226.1000014189999945 ) ) ;
#27723 = ADVANCED_FACE ( 'NONE', ( #16311 ), #4358, .F. ) ;
#27724 = CARTESIAN_POINT ( 'NONE',  ( 20.64716981389999972, -20.77933506589999979, 222.0000000000000000 ) ) ;
#27725 = CARTESIAN_POINT ( 'NONE',  ( 18.02779606829999892, 3.032253802040000057, 230.6999999999999886 ) ) ;
#27726 = CARTESIAN_POINT ( 'NONE',  ( 3.938868613454878709, -1.397147637169312340, -40.13554055886279315 ) ) ;
#27727 = ORIENTED_EDGE ( 'NONE', *, *, #15174, .F. ) ;
#27728 = CARTESIAN_POINT ( 'NONE',  ( -4.178199994060140199, -1.098053884355548737, -56.45102360502500005 ) ) ;
#27729 = PLANE ( 'NONE',  #1758 ) ;
#27730 = VERTEX_POINT ( 'NONE', #29185 ) ;
#27731 = CARTESIAN_POINT ( 'NONE',  ( 0.5074138422395748638, -6.503547975687064664, -9.393384211799999051 ) ) ;
#27732 = ORIENTED_EDGE ( 'NONE', *, *, #133, .F. ) ;
#27733 = CARTESIAN_POINT ( 'NONE',  ( -25.20890834729999952, -13.29605215849999844, 225.3106485179999936 ) ) ;
#27734 = CARTESIAN_POINT ( 'NONE',  ( 133283.2115610000037, 454258.9661130000022, -160669.8390839999774 ) ) ;
#27736 = ORIENTED_EDGE ( 'NONE', *, *, #5, .T. ) ;
#27735 = VECTOR ( 'NONE', #6288, 1000.000000000000000 ) ;
#27737 = LINE ( 'NONE', #9593, #3925 ) ;
#27738 = ORIENTED_EDGE ( 'NONE', *, *, #4885, .F. ) ;
#27739 = ORIENTED_EDGE ( 'NONE', *, *, #3987, .F. ) ;
#27740 = CARTESIAN_POINT ( 'NONE',  ( 3.458129700887829561, -0.5397582531443678722, -88.52261276240527366 ) ) ;
#27741 =( NAMED_UNIT ( * ) PLANE_ANGLE_UNIT ( ) SI_UNIT ( $, .RADIAN. ) );
#27742 = B_SPLINE_CURVE_WITH_KNOTS ( 'NONE', 3,
 ( #20088, #20393, #20547, #6223, #25439, #18963, #11727, #23550, #26208, #28097, #16135, #6538, #4342, #28247, #13461, #18803, #25907, #13779 ),
 .UNSPECIFIED., .F., .F.,
 ( 4, 2, 2, 2, 2, 2, 2, 2, 4 ),
 ( 0.000000000000000000, 0.1249999999999999722, 0.2500000000000000000, 0.3750000000000000000, 0.5000000000000001110, 0.6250000000000001110, 0.7500000000000000000, 0.8750000000000000000, 1.000000000000000000 ),
 .UNSPECIFIED. ) ;
#27743 = ORIENTED_EDGE ( 'NONE', *, *, #30631, .F. ) ;
#27744 = CARTESIAN_POINT ( 'NONE',  ( 24.90302311548996883, -13.86047864964742793, 6.098655051000018368 ) ) ;
#27745 = CARTESIAN_POINT ( 'NONE',  ( 2.107992564109752998, -27.41908764619381245, 210.0000000000000284 ) ) ;
#27746 = CARTESIAN_POINT ( 'NONE',  ( 4.883349601227576997, 0.1168011502185872796, -64.06686508972499894 ) ) ;
#27747 = FACE_OUTER_BOUND ( 'NONE', #30340, .T. ) ;
#27748 = CARTESIAN_POINT ( 'NONE',  ( -0.1474953975175301857, -26.80000000000002203, 223.9000000000000057 ) ) ;
#27749 = EDGE_CURVE ( 'NONE', #28706, #11915, #2343, .T. ) ;
#27750 = CARTESIAN_POINT ( 'NONE',  ( 10.67300410500000041, 19.99999999999999645, -42.78321928043000355 ) ) ;
#27751 = DIRECTION ( 'NONE',  ( 1.000000000000000000, 0.000000000000000000, 0.000000000000000000 ) ) ;
#27752 = CARTESIAN_POINT ( 'NONE',  ( -25.44662322720032677, 12.83524168051548564, 4.689351480999998323 ) ) ;
#27753 = EDGE_CURVE ( 'NONE', #5262, #30396, #15789, .T. ) ;
#27754 = CARTESIAN_POINT ( 'NONE',  ( -3.950034095761355335, 2.484763540022569384, -10.44547590280000371 ) ) ;
#27755 = CARTESIAN_POINT ( 'NONE',  ( 0.000000000000000000, 0.000000000000000000, 90.00000000000000000 ) ) ;
#27756 = ADVANCED_FACE ( 'NONE', ( #3067 ), #4972, .T. ) ;
#27757 = B_SPLINE_CURVE_WITH_KNOTS ( 'NONE', 5,
 ( #11685, #23810, #9477, #21750, #9158, #200, #31040, #14369, #23967, #19231, #28815, #9792, #19392, #28981, #7424 ),
 .UNSPECIFIED., .F., .F.,
 ( 6, 3, 3, 3, 6 ),
 ( 0.000000000000000000, 0.2999999999999999889, 0.6000000000034357850, 0.8999999999965643260, 1.000000000000000000 ),
 .UNSPECIFIED. ) ;
#27758 = DIRECTION ( 'NONE',  ( -2.764840495839172918E-12, -0.9128796883888953273, 0.4082287037029531107 ) ) ;
#27759 = CIRCLE ( 'NONE', #3140, 27.92857142860000152 ) ;
#27760 = ORIENTED_EDGE ( 'NONE', *, *, #1163, .T. ) ;
#27761 = CYLINDRICAL_SURFACE ( 'NONE', #7152, 3.000000000000000444 ) ;
#27762 = PLANE ( 'NONE',  #26839 ) ;
#27763 = CARTESIAN_POINT ( 'NONE',  ( -23.69427943501400691, -14.54081806258934861, 6.079851352000009257 ) ) ;
#27764 = CARTESIAN_POINT ( 'NONE',  ( 21.85863980187338740, 17.64392717939186284, 0.5514269750000189152 ) ) ;
#27765 = DIRECTION ( 'NONE',  ( 0.7071067811865475727, 0.7071067811865475727, 0.000000000000000000 ) ) ;
#27766 = CARTESIAN_POINT ( 'NONE',  ( -3.362912017748242999, 4.936852587875802278, -48.05391720702499470 ) ) ;
#27767 = CARTESIAN_POINT ( 'NONE',  ( -10.40384843829999895, -24.69832375660000423, -1.291913792900001301 ) ) ;
#27768 = LINE ( 'NONE', #6055, #208 ) ;
#27769 = EDGE_LOOP ( 'NONE', ( #29521, #13465, #12925, #22982 ) ) ;
#27770 = CARTESIAN_POINT ( 'NONE',  ( 24.81746042554890863, -14.01353061607344053, 3.920132063000014710 ) ) ;
#27771 = CARTESIAN_POINT ( 'NONE',  ( 22.83442928010000017, 16.43389279790000046, 229.0000000000000000 ) ) ;
#27772 = CARTESIAN_POINT ( 'NONE',  ( 2.746170412676653072, -3.444806756781638502, -68.10000000002500542 ) ) ;
#27773 = CARTESIAN_POINT ( 'NONE',  ( 3.607555131306940499, 0.2156355436844743512, -68.79984462960774749 ) ) ;
#27774 = CARTESIAN_POINT ( 'NONE',  ( -23.77307140041805411, 14.41181874028064591, 4.999998581000003384 ) ) ;
#27775 = SHAPE_REPRESENTATION_RELATIONSHIP ( 'NONE' , 'NONE' ,  #20820, #15531 ) ;
#27776 = CYLINDRICAL_SURFACE ( 'NONE', #16209, 3.000000000000002220 ) ;
#27777 = CARTESIAN_POINT ( 'NONE',  ( -23.35349119075231172, 13.32552209464216553, -0.6999999999999992895 ) ) ;
#27778 = VECTOR ( 'NONE', #12897, 1000.000000000000114 ) ;
#27779 = B_SPLINE_CURVE_WITH_KNOTS ( 'NONE', 5,
 ( #13246, #25064, #22701, #5855, #13407, #17654, #30094, #3497, #6170, #10590, #8520, #11059, #22863, #11209, #3821, #15770, #1307, #27568, #13093, #18122, #10901, #23022, #1468, #3339 ),
 .UNSPECIFIED., .F., .F.,
 ( 6, 3, 3, 3, 3, 3, 3, 6 ),
 ( 0.000000000000000000, 18.45572787860000119, 36.93774665009999580, 55.41656326359999696, 72.02514973920000330, 90.47575867250000670, 108.9324419860000006, 122.5879169570000045 ),
 .UNSPECIFIED. ) ;
#27780 = CARTESIAN_POINT ( 'NONE',  ( -2.911316102860717070, -3.927725552502972839, -65.53409070562500460 ) ) ;
#27781 = ORIENTED_EDGE ( 'NONE', *, *, #29279, .T. ) ;
#27782 = CARTESIAN_POINT ( 'NONE',  ( 18.40063513716208377, 20.00005172663331976, 230.6578942932893597 ) ) ;
#27783 = ORIENTED_EDGE ( 'NONE', *, *, #18799, .T. ) ;
#27784 = CARTESIAN_POINT ( 'NONE',  ( -18.62349881349999947, 19.80369232029999793, 229.9327143820000003 ) ) ;
#27785 = ORIENTED_EDGE ( 'NONE', *, *, #1198, .T. ) ;
#27786 = CARTESIAN_POINT ( 'NONE',  ( 24.04107748419999879, -13.95955969929999974, 226.0986569330000293 ) ) ;
#27787 = CARTESIAN_POINT ( 'NONE',  ( -11.83960380690999870, -27.00000000000000000, -28.40000000000771863 ) ) ;
#27788 = CARTESIAN_POINT ( 'NONE',  ( -16.83342759559999635, -9.000000000000001776, -1.399999999999998579 ) ) ;
#27789 = DIRECTION ( 'NONE',  ( 0.000000000000000000, 0.000000000000000000, 1.000000000000000000 ) ) ;
#27790 = ADVANCED_FACE ( 'NONE', ( #26531 ), #2770, .F. ) ;
#27791 =( BOUNDED_SURFACE ( )  B_SPLINE_SURFACE ( 5, 5, ( 
 ( #29460, #27106, #22393, #3639, #8197, #1135 ),
 ( #3330, #3180, #15760, #30237, #8509, #13234 ),
 ( #24905, #837, #10727, #20641, #17947, #27558 ),
 ( #27712, #15451, #29765, #27879, #3485, #6003 ),
 ( #22850, #17798, #25053, #15602, #20175, #27409 ),
 ( #20327, #12937, #20483, #18268, #30084, #12784 ),
 ( #25205, #13081, #20021, #22547, #23009, #1298 ),
 ( #6324, #10581, #29926, #15919, #10892, #29618 ),
 ( #22692, #18110, #8050, #990, #17645, #10429 ),
 ( #5847, #8352, #27257, #6158, #25372, #3811 ),
 ( #13398, #5694, #1457, #11050, #8670, #15301 ),
 ( #28654, #28498, #30407, #25843, #21116, #30562 ),
 ( #28030, #8990, #13877, #25688, #13716, #16076 ),
 ( #25527, #6943, #4119, #7101, #13561, #1769 ),
 ( #23484, #11359, #23324, #1922, #2076, #9139 ),
 ( #23168, #20956, #18590, #18742, #16228, #28186 ),
 ( #30870, #11827, #11514, #6475, #4279, #30712 ),
 ( #2236, #3963, #6629, #18901, #28343, #6789 ),
 ( #1609, #11198, #20800, #8828, #4433, #18433 ),
 ( #16385, #25993, #14037, #23639, #11668, #21266 ),
 ( #31019, #26148, #9299, #21428, #16539, #23790 ),
 ( #4580, #14188, #9455, #19059, #345, #16687 ),
 ( #2537, #16849, #24405, #14809, #14502, #4746 ),
 ( #21731, #14655, #22194, #14959, #26757, #29422 ),
 ( #19374, #9771, #7560, #9927, #26298, #23953 ),
 ( #12432, #24099, #26917, #19840, #10086, #19528 ),
 ( #28964, #7406, #22050, #12125, #2837, #5193 ),
 ( #21898, #10238, #29116, #183, #19214, #17005 ),
 ( #500, #2388, #17151, #19680, #26607, #24558 ),
 ( #14352, #5047, #29265, #24243, #7259, #2685 ),
 ( #11973, #21585, #32, #7705, #9614, #28796 ),
 ( #12285, #26455, #4898, #17311, #5354, #2996 ),
 ( #12586, #651, #18070, #8316, #25013, #5815 ),
 ( #10691, #3446, #17911, #22655, #7856, #20141 ),
 ( #8013, #15560, #5965, #5660, #27066, #27519 ),
 ( #15413, #13362, #6121, #25169, #20601, #22509 ),
 ( #956, #29888, #1098, #17460, #15111, #13048 ),
 ( #15259, #27675, #11010, #1261, #20285, #17756 ),
 ( #29732, #13196, #24869, #3601, #22808, #3297 ),
 ( #10858, #5504, #24705, #20443, #30041, #3143 ),
 ( #15715, #8474, #12741, #22354, #25328, #10546 ),
 ( #3771, #801, #1417, #12901, #22970, #10391 ),
 ( #8160, #27376, #17611, #27219, #29577, #19982 ),
 ( #2041, #20759, #11786, #18226, #6438, #16037 ),
 ( #25653, #27993, #6594, #6749, #13841, #3927 ),
 ( #13521, #30364, #15886, #30198, #8629, #14151 ),
 ( #27834, #13680, #8793, #23451, #6286, #16500 ),
 ( #16191, #16348, #11326, #25489, #18396, #4083 ),
 ( #20923, #23284, #1727, #4393, #26111, #25807 ),
 ( #30525, #28154, #8953, #6898, #23134, #18552 ),
 ( #4239, #1881, #11480, #1576, #11162, #2197 ),
 ( #11630, #21081, #30829, #21228, #30678, #9105 ),
 ( #18705, #28304, #25957, #13999, #23605, #9256 ),
 ( #18865, #28462, #4549, #23756, #24208, #16964 ),
 ( #5010, #21392, #2502, #7218, #21544, #29079 ),
 ( #19177, #9414, #21859, #26421, #19336, #26879 ),
 ( #30983, #2807, #17271, #26718, #310, #7667 ),
 ( #19020, #28927, #5320, #14618, #2648, #7372 ),
 ( #12090, #16807, #14924, #21698, #12242, #14312 ),
 ( #4863, #147, #9888, #14464, #24064, #24521 ),
 ( #12299, #7523, #2958, #17118, #28621, #5155 ),
 ( #14767, #9728, #12399, #7061, #24366, #26262 ),
 ( #26570, #19491, #22010, #23917, #467, #10048 ),
 ( #16651, #19644, #29228, #4701, #2352, #11936 ),
 ( #9580, #28764, #3412, #29541, #10656, #13163 ),
 ( #29386, #27183, #22469, #19948, #919, #27031 ),
 ( #15222, #15074, #12702, #24672, #20109, #12552 ),
 ( #3106, #22159, #19800, #10357, #7976, #3260 ),
 ( #764, #10510, #13014, #29698, #5468, #22312 ),
 ( #22771, #8123, #17576, #5622, #24828, #17425 ),
 ( #17720, #12865, #27338, #5778, #15378, #15528 ),
 ( #27481, #7825, #616, #24976, #22625, #20247 ),
 ( #8282, #1066, #17877, #29848, #5928, #25133 ),
 ( #3569, #10201, #28718, #21957, #2757, #7471 ),
 ( #14568, #19747, #9993, #26666, #17067, #10150 ),
 ( #5108, #19592, #24308, #9527, #21798, #26516 ),
 ( #17216, #7621, #7324, #7166, #29173, #24158 ),
 ( #15026, #7774, #26822, #22259, #2599, #12186 ),
 ( #410, #12351, #19124, #16753, #14717, #5267 ),
 ( #29330, #12650, #2905, #14878, #19434, #253 ),
 ( #24470, #16909, #12497, #22108, #4957, #9838 ),
 ( #24620, #26370, #29025, #566, #17372, #26978 ),
 ( #4816, #14411, #5417, #3054, #24012, #2452 ),
 ( #12043, #21650, #98, #9677, #19280, #28871 ),
 ( #24535, #2820, #17288, #12566, #7992, #29556 ),
 ( #24384, #2516, #5483, #24685, #12411, #26434 ),
 ( #22172, #19506, #7836, #4874, #29400, #161 ),
 ( #22029, #322, #480, #28942, #9904, #14784 ),
 ( #14632, #16980, #29243, #14478, #17439, #26585 ),
 ( #24077, #2664, #12260, #10062, #21876, #24222 ),
 ( #2976, #19658, #9745, #19350, #7681, #19962 ),
 ( #17131, #5025, #29093, #632, #12717, #26894 ),
 ( #26732, #5333, #7539, #3120, #12102, #5170 ),
 ( #14937, #10214, #19817, #21711, #7384, #27046 ),
 ( #15091, #22329, #779, #10371, #22483, #18048 ),
 ( #22636, #24990, #11144, #23116, #18208, #15392 ),
 ( #20123, #15868, #1240, #932, #17590, #25308 ),
 ( #10837, #27199, #29863, #3425, #17735, #3750 ),
 ( #13027, #5638, #27654, #1079, #15541, #1556 ),
 ( #6096, #20741, #25471, #15694, #30341, #10670 ),
 ( #20265, #8451, #20423, #15235, #24845, #22787 ),
 ( #30016, #3581, #10990, #8295, #17890, #3274 ),
 ( #13344, #10525, #22950, #27496, #29711, #5942 ),
 ( #25146, #12879, #13176, #27352, #1394, #8139 ),
 ( #5794, #20582, #30178, #8608, #27815, #6266 ),
 ( #3905, #13499, #2332, #16170, #25935, #23896 ),
 ( #25634, #23431, #9085, #23736, #13659, #30504 ),
 ( #8773, #21520, #11916, #1858, #18379, #11458 ) ),
 .UNSPECIFIED., .F., .F., .T. ) 
 B_SPLINE_SURFACE_WITH_KNOTS ( ( 6, 3, 3, 3, 3, 3, 3, 3, 3, 3, 3, 3, 3, 3, 3, 3, 3, 3, 3, 3, 3, 3, 3, 3, 3, 3, 3, 3, 3, 3, 3, 3, 3, 3, 3, 6 ),
 ( 6, 6 ),
 ( 0.000000000000000000, 11.38862009670000042, 23.17260734259999921, 34.79167593860000096, 46.25425528950000142, 57.87229377410000097, 69.67120816000000616, 81.20502170430000888, 92.80704244429999505, 104.1208912059999960, 115.9269080290000034, 127.3307717769999954, 139.1306782750000082, 150.7654282180000109, 162.2434640489999822, 173.6637378899999931, 185.2020570420000070, 194.1769840820000184, 203.3038760180000111, 212.5853790139999830, 224.1393301889999918, 235.6932813650000185, 246.8715721779999797, 258.4996770380000157, 270.1277818960000445, 281.7035649139999691, 293.2822232819999613, 304.6732510989999696, 316.1434960830000023, 327.6894369340000139, 339.2353777880000507, 350.7813186390000055, 362.5843219139999860, 374.0573691039999744, 385.8560256170000002, 397.5961180479999939 ),
 ( 8.337129679329999377, 16.67425935869999876 ),
 .UNSPECIFIED. ) 
 GEOMETRIC_REPRESENTATION_ITEM ( )  RATIONAL_B_SPLINE_SURFACE ( (
 ( 0.2500000000000000000, 0.2500000000000000000, 0.2999999999999999889, 0.4000000000000000222, 0.5999999999999999778, 1.000000000000000000),
 ( 0.2500000000000000000, 0.2500000000000000000, 0.2999999999999999889, 0.4000000000000000222, 0.5999999999999999778, 1.000000000000000000),
 ( 0.2500000000000000000, 0.2500000000000000000, 0.2999999999999999889, 0.4000000000000000222, 0.5999999999999999778, 1.000000000000000000),
 ( 0.2500000000000000000, 0.2500000000000000000, 0.2999999999999999889, 0.4000000000000000222, 0.5999999999999999778, 1.000000000000000000),
 ( 0.2500000000000000000, 0.2500000000000000000, 0.2999999999999999889, 0.4000000000000000222, 0.5999999999999999778, 1.000000000000000000),
 ( 0.2500000000000000000, 0.2500000000000000000, 0.2999999999999999889, 0.4000000000000000222, 0.5999999999999999778, 1.000000000000000000),
 ( 0.2500000000000000000, 0.2500000000000000000, 0.2999999999999999889, 0.4000000000000000222, 0.5999999999999999778, 1.000000000000000000),
 ( 0.2500000000000000000, 0.2500000000000000000, 0.2999999999999999889, 0.4000000000000000222, 0.5999999999999999778, 1.000000000000000000),
 ( 0.2500000000000000000, 0.2500000000000000000, 0.2999999999999999889, 0.4000000000000000222, 0.5999999999999999778, 1.000000000000000000),
 ( 0.2500000000000000000, 0.2500000000000000000, 0.2999999999999999889, 0.4000000000000000222, 0.5999999999999999778, 1.000000000000000000),
 ( 0.2500000000000000000, 0.2500000000000000000, 0.2999999999999999889, 0.4000000000000000222, 0.5999999999999999778, 1.000000000000000000),
 ( 0.2500000000000000000, 0.2500000000000000000, 0.2999999999999999889, 0.4000000000000000222, 0.5999999999999999778, 1.000000000000000000),
 ( 0.2500000000000000000, 0.2500000000000000000, 0.2999999999999999889, 0.4000000000000000222, 0.5999999999999999778, 1.000000000000000000),
 ( 0.2500000000000000000, 0.2500000000000000000, 0.2999999999999999889, 0.4000000000000000222, 0.5999999999999999778, 1.000000000000000000),
 ( 0.2500000000000000000, 0.2500000000000000000, 0.2999999999999999889, 0.4000000000000000222, 0.5999999999999999778, 1.000000000000000000),
 ( 0.2500000000000000000, 0.2500000000000000000, 0.2999999999999999889, 0.4000000000000000222, 0.5999999999999999778, 1.000000000000000000),
 ( 0.2500000000000000000, 0.2500000000000000000, 0.2999999999999999889, 0.4000000000000000222, 0.5999999999999999778, 1.000000000000000000),
 ( 0.2500000000000000000, 0.2500000000000000000, 0.2999999999999999889, 0.4000000000000000222, 0.5999999999999999778, 1.000000000000000000),
 ( 0.2500000000000000000, 0.2500000000000000000, 0.2999999999999999889, 0.4000000000000000222, 0.5999999999999999778, 1.000000000000000000),
 ( 0.2500000000000000000, 0.2500000000000000000, 0.2999999999999999889, 0.4000000000000000222, 0.5999999999999999778, 1.000000000000000000),
 ( 0.2500000000000000000, 0.2500000000000000000, 0.2999999999999999889, 0.4000000000000000222, 0.5999999999999999778, 1.000000000000000000),
 ( 0.2500000000000000000, 0.2500000000000000000, 0.2999999999999999889, 0.4000000000000000222, 0.5999999999999999778, 1.000000000000000000),
 ( 0.2500000000000000000, 0.2500000000000000000, 0.2999999999999999889, 0.4000000000000000222, 0.5999999999999999778, 1.000000000000000000),
 ( 0.2500000000000000000, 0.2500000000000000000, 0.2999999999999999889, 0.4000000000000000222, 0.5999999999999999778, 1.000000000000000000),
 ( 0.2500000000000000000, 0.2500000000000000000, 0.2999999999999999889, 0.4000000000000000222, 0.5999999999999999778, 1.000000000000000000),
 ( 0.2500000000000000000, 0.2500000000000000000, 0.2999999999999999889, 0.4000000000000000222, 0.5999999999999999778, 1.000000000000000000),
 ( 0.2500000000000000000, 0.2500000000000000000, 0.2999999999999999889, 0.4000000000000000222, 0.5999999999999999778, 1.000000000000000000),
 ( 0.2500000000000000000, 0.2500000000000000000, 0.2999999999999999889, 0.4000000000000000222, 0.5999999999999999778, 1.000000000000000000),
 ( 0.2500000000000000000, 0.2500000000000000000, 0.2999999999999999889, 0.4000000000000000222, 0.5999999999999999778, 1.000000000000000000),
 ( 0.2500000000000000000, 0.2500000000000000000, 0.2999999999999999889, 0.4000000000000000222, 0.5999999999999999778, 1.000000000000000000),
 ( 0.2500000000000000000, 0.2500000000000000000, 0.2999999999999999889, 0.4000000000000000222, 0.5999999999999999778, 1.000000000000000000),
 ( 0.2500000000000000000, 0.2500000000000000000, 0.2999999999999999889, 0.4000000000000000222, 0.5999999999999999778, 1.000000000000000000),
 ( 0.2500000000000000000, 0.2500000000000000000, 0.2999999999999999889, 0.4000000000000000222, 0.5999999999999999778, 1.000000000000000000),
 ( 0.2500000000000000000, 0.2500000000000000000, 0.2999999999999999889, 0.4000000000000000222, 0.5999999999999999778, 1.000000000000000000),
 ( 0.2500000000000000000, 0.2500000000000000000, 0.2999999999999999889, 0.4000000000000000222, 0.5999999999999999778, 1.000000000000000000),
 ( 0.2500000000000000000, 0.2500000000000000000, 0.2999999999999999889, 0.4000000000000000222, 0.5999999999999999778, 1.000000000000000000),
 ( 0.2500000000000000000, 0.2500000000000000000, 0.2999999999999999889, 0.4000000000000000222, 0.5999999999999999778, 1.000000000000000000),
 ( 0.2500000000000000000, 0.2500000000000000000, 0.2999999999999999889, 0.4000000000000000222, 0.5999999999999999778, 1.000000000000000000),
 ( 0.2500000000000000000, 0.2500000000000000000, 0.2999999999999999889, 0.4000000000000000222, 0.5999999999999999778, 1.000000000000000000),
 ( 0.2500000000000000000, 0.2500000000000000000, 0.2999999999999999889, 0.4000000000000000222, 0.5999999999999999778, 1.000000000000000000),
 ( 0.2500000000000000000, 0.2500000000000000000, 0.2999999999999999889, 0.4000000000000000222, 0.5999999999999999778, 1.000000000000000000),
 ( 0.2500000000000000000, 0.2500000000000000000, 0.2999999999999999889, 0.4000000000000000222, 0.5999999999999999778, 1.000000000000000000),
 ( 0.2500000000000000000, 0.2500000000000000000, 0.2999999999999999889, 0.4000000000000000222, 0.5999999999999999778, 1.000000000000000000),
 ( 0.2500000000000000000, 0.2500000000000000000, 0.2999999999999999889, 0.4000000000000000222, 0.5999999999999999778, 1.000000000000000000),
 ( 0.2500000000000000000, 0.2500000000000000000, 0.2999999999999999889, 0.4000000000000000222, 0.5999999999999999778, 1.000000000000000000),
 ( 0.2500000000000000000, 0.2500000000000000000, 0.2999999999999999889, 0.4000000000000000222, 0.5999999999999999778, 1.000000000000000000),
 ( 0.2500000000000000000, 0.2500000000000000000, 0.2999999999999999889, 0.4000000000000000222, 0.5999999999999999778, 1.000000000000000000),
 ( 0.2500000000000000000, 0.2500000000000000000, 0.2999999999999999889, 0.4000000000000000222, 0.5999999999999999778, 1.000000000000000000),
 ( 0.2500000000000000000, 0.2500000000000000000, 0.2999999999999999889, 0.4000000000000000222, 0.5999999999999999778, 1.000000000000000000),
 ( 0.2500000000000000000, 0.2500000000000000000, 0.2999999999999999889, 0.4000000000000000222, 0.5999999999999999778, 1.000000000000000000),
 ( 0.2500000000000000000, 0.2500000000000000000, 0.2999999999999999889, 0.4000000000000000222, 0.5999999999999999778, 1.000000000000000000),
 ( 0.2500000000000000000, 0.2500000000000000000, 0.2999999999999999889, 0.4000000000000000222, 0.5999999999999999778, 1.000000000000000000),
 ( 0.2500000000000000000, 0.2500000000000000000, 0.2999999999999999889, 0.4000000000000000222, 0.5999999999999999778, 1.000000000000000000),
 ( 0.2500000000000000000, 0.2500000000000000000, 0.2999999999999999889, 0.4000000000000000222, 0.5999999999999999778, 1.000000000000000000),
 ( 0.2500000000000000000, 0.2500000000000000000, 0.2999999999999999889, 0.4000000000000000222, 0.5999999999999999778, 1.000000000000000000),
 ( 0.2500000000000000000, 0.2500000000000000000, 0.2999999999999999889, 0.4000000000000000222, 0.5999999999999999778, 1.000000000000000000),
 ( 0.2500000000000000000, 0.2500000000000000000, 0.2999999999999999889, 0.4000000000000000222, 0.5999999999999999778, 1.000000000000000000),
 ( 0.2500000000000000000, 0.2500000000000000000, 0.2999999999999999889, 0.4000000000000000222, 0.5999999999999999778, 1.000000000000000000),
 ( 0.2500000000000000000, 0.2500000000000000000, 0.2999999999999999889, 0.4000000000000000222, 0.5999999999999999778, 1.000000000000000000),
 ( 0.2500000000000000000, 0.2500000000000000000, 0.2999999999999999889, 0.4000000000000000222, 0.5999999999999999778, 1.000000000000000000),
 ( 0.2500000000000000000, 0.2500000000000000000, 0.2999999999999999889, 0.4000000000000000222, 0.5999999999999999778, 1.000000000000000000),
 ( 0.2500000000000000000, 0.2500000000000000000, 0.2999999999999999889, 0.4000000000000000222, 0.5999999999999999778, 1.000000000000000000),
 ( 0.2500000000000000000, 0.2500000000000000000, 0.2999999999999999889, 0.4000000000000000222, 0.5999999999999999778, 1.000000000000000000),
 ( 0.2500000000000000000, 0.2500000000000000000, 0.2999999999999999889, 0.4000000000000000222, 0.5999999999999999778, 1.000000000000000000),
 ( 0.2500000000000000000, 0.2500000000000000000, 0.2999999999999999889, 0.4000000000000000222, 0.5999999999999999778, 1.000000000000000000),
 ( 0.2500000000000000000, 0.2500000000000000000, 0.2999999999999999889, 0.4000000000000000222, 0.5999999999999999778, 1.000000000000000000),
 ( 0.2500000000000000000, 0.2500000000000000000, 0.2999999999999999889, 0.4000000000000000222, 0.5999999999999999778, 1.000000000000000000),
 ( 0.2500000000000000000, 0.2500000000000000000, 0.2999999999999999889, 0.4000000000000000222, 0.5999999999999999778, 1.000000000000000000),
 ( 0.2500000000000000000, 0.2500000000000000000, 0.2999999999999999889, 0.4000000000000000222, 0.5999999999999999778, 1.000000000000000000),
 ( 0.2500000000000000000, 0.2500000000000000000, 0.2999999999999999889, 0.4000000000000000222, 0.5999999999999999778, 1.000000000000000000),
 ( 0.2500000000000000000, 0.2500000000000000000, 0.2999999999999999889, 0.4000000000000000222, 0.5999999999999999778, 1.000000000000000000),
 ( 0.2500000000000000000, 0.2500000000000000000, 0.2999999999999999889, 0.4000000000000000222, 0.5999999999999999778, 1.000000000000000000),
 ( 0.2500000000000000000, 0.2500000000000000000, 0.2999999999999999889, 0.4000000000000000222, 0.5999999999999999778, 1.000000000000000000),
 ( 0.2500000000000000000, 0.2500000000000000000, 0.2999999999999999889, 0.4000000000000000222, 0.5999999999999999778, 1.000000000000000000),
 ( 0.2500000000000000000, 0.2500000000000000000, 0.2999999999999999889, 0.4000000000000000222, 0.5999999999999999778, 1.000000000000000000),
 ( 0.2500000000000000000, 0.2500000000000000000, 0.2999999999999999889, 0.4000000000000000222, 0.5999999999999999778, 1.000000000000000000),
 ( 0.2500000000000000000, 0.2500000000000000000, 0.2999999999999999889, 0.4000000000000000222, 0.5999999999999999778, 1.000000000000000000),
 ( 0.2500000000000000000, 0.2500000000000000000, 0.2999999999999999889, 0.4000000000000000222, 0.5999999999999999778, 1.000000000000000000),
 ( 0.2500000000000000000, 0.2500000000000000000, 0.2999999999999999889, 0.4000000000000000222, 0.5999999999999999778, 1.000000000000000000),
 ( 0.2500000000000000000, 0.2500000000000000000, 0.2999999999999999889, 0.4000000000000000222, 0.5999999999999999778, 1.000000000000000000),
 ( 0.2500000000000000000, 0.2500000000000000000, 0.2999999999999999889, 0.4000000000000000222, 0.5999999999999999778, 1.000000000000000000),
 ( 0.2500000000000000000, 0.2500000000000000000, 0.2999999999999999889, 0.4000000000000000222, 0.5999999999999999778, 1.000000000000000000),
 ( 0.2500000000000000000, 0.2500000000000000000, 0.2999999999999999889, 0.4000000000000000222, 0.5999999999999999778, 1.000000000000000000),
 ( 0.2500000000000000000, 0.2500000000000000000, 0.2999999999999999889, 0.4000000000000000222, 0.5999999999999999778, 1.000000000000000000),
 ( 0.2500000000000000000, 0.2500000000000000000, 0.2999999999999999889, 0.4000000000000000222, 0.5999999999999999778, 1.000000000000000000),
 ( 0.2500000000000000000, 0.2500000000000000000, 0.2999999999999999889, 0.4000000000000000222, 0.5999999999999999778, 1.000000000000000000),
 ( 0.2500000000000000000, 0.2500000000000000000, 0.2999999999999999889, 0.4000000000000000222, 0.5999999999999999778, 1.000000000000000000),
 ( 0.2500000000000000000, 0.2500000000000000000, 0.2999999999999999889, 0.4000000000000000222, 0.5999999999999999778, 1.000000000000000000),
 ( 0.2500000000000000000, 0.2500000000000000000, 0.2999999999999999889, 0.4000000000000000222, 0.5999999999999999778, 1.000000000000000000),
 ( 0.2500000000000000000, 0.2500000000000000000, 0.2999999999999999889, 0.4000000000000000222, 0.5999999999999999778, 1.000000000000000000),
 ( 0.2500000000000000000, 0.2500000000000000000, 0.2999999999999999889, 0.4000000000000000222, 0.5999999999999999778, 1.000000000000000000),
 ( 0.2500000000000000000, 0.2500000000000000000, 0.2999999999999999889, 0.4000000000000000222, 0.5999999999999999778, 1.000000000000000000),
 ( 0.2500000000000000000, 0.2500000000000000000, 0.2999999999999999889, 0.4000000000000000222, 0.5999999999999999778, 1.000000000000000000),
 ( 0.2500000000000000000, 0.2500000000000000000, 0.2999999999999999889, 0.4000000000000000222, 0.5999999999999999778, 1.000000000000000000),
 ( 0.2500000000000000000, 0.2500000000000000000, 0.2999999999999999889, 0.4000000000000000222, 0.5999999999999999778, 1.000000000000000000),
 ( 0.2500000000000000000, 0.2500000000000000000, 0.2999999999999999889, 0.4000000000000000222, 0.5999999999999999778, 1.000000000000000000),
 ( 0.2500000000000000000, 0.2500000000000000000, 0.2999999999999999889, 0.4000000000000000222, 0.5999999999999999778, 1.000000000000000000),
 ( 0.2500000000000000000, 0.2500000000000000000, 0.2999999999999999889, 0.4000000000000000222, 0.5999999999999999778, 1.000000000000000000),
 ( 0.2500000000000000000, 0.2500000000000000000, 0.2999999999999999889, 0.4000000000000000222, 0.5999999999999999778, 1.000000000000000000),
 ( 0.2500000000000000000, 0.2500000000000000000, 0.2999999999999999889, 0.4000000000000000222, 0.5999999999999999778, 1.000000000000000000),
 ( 0.2500000000000000000, 0.2500000000000000000, 0.2999999999999999889, 0.4000000000000000222, 0.5999999999999999778, 1.000000000000000000),
 ( 0.2500000000000000000, 0.2500000000000000000, 0.2999999999999999889, 0.4000000000000000222, 0.5999999999999999778, 1.000000000000000000),
 ( 0.2500000000000000000, 0.2500000000000000000, 0.2999999999999999889, 0.4000000000000000222, 0.5999999999999999778, 1.000000000000000000),
 ( 0.2500000000000000000, 0.2500000000000000000, 0.2999999999999999889, 0.4000000000000000222, 0.5999999999999999778, 1.000000000000000000),
 ( 0.2500000000000000000, 0.2500000000000000000, 0.2999999999999999889, 0.4000000000000000222, 0.5999999999999999778, 1.000000000000000000),
 ( 0.2500000000000000000, 0.2500000000000000000, 0.2999999999999999889, 0.4000000000000000222, 0.5999999999999999778, 1.000000000000000000),
 ( 0.2500000000000000000, 0.2500000000000000000, 0.2999999999999999889, 0.4000000000000000222, 0.5999999999999999778, 1.000000000000000000),
 ( 0.2500000000000000000, 0.2500000000000000000, 0.2999999999999999889, 0.4000000000000000222, 0.5999999999999999778, 1.000000000000000000) ) ) 
 REPRESENTATION_ITEM ( '' )  SURFACE ( )  );
#27792 = CARTESIAN_POINT ( 'NONE',  ( 18.13191322229999969, 10.47263190749999495, -1.399999999599998990 ) ) ;
#27793 = DIRECTION ( 'NONE',  ( 1.000000000000000000, 0.000000000000000000, 0.000000000000000000 ) ) ;
#27794 = EDGE_CURVE ( 'NONE', #17040, #4771, #15295, .T. ) ;
#27795 = DIRECTION ( 'NONE',  ( 0.000000000000000000, 0.000000000000000000, -1.000000000000000000 ) ) ;
#27796 = ORIENTED_EDGE ( 'NONE', *, *, #19072, .F. ) ;
#27797 = CARTESIAN_POINT ( 'NONE',  ( -0.8022125085872947592, -3.843042093354096078, -44.10000000002498410 ) ) ;
#27798 = CIRCLE ( 'NONE', #18239, 3.200000000000002398 ) ;
#27799 = CARTESIAN_POINT ( 'NONE',  ( 27.07818553041514065, 6.807801137122736712, 8.000000000000007105 ) ) ;
#27800 = VECTOR ( 'NONE', #4631, 1000.000000000000000 ) ;
#27801 = CARTESIAN_POINT ( 'NONE',  ( 1.063741597852546183, -27.77980805031950240, 225.2880308456763885 ) ) ;
#27802 = CARTESIAN_POINT ( 'NONE',  ( -2.605017075328921017, -2.487964477322084811, 230.7771899713821426 ) ) ;
#27803 = CARTESIAN_POINT ( 'NONE',  ( -24.62906106470000012, -14.34164290000000008, 226.0959707279999975 ) ) ;
#27804 = TOROIDAL_SURFACE ( 'NONE', #7691, 24.50000000000000000, 4.000000000000000000 ) ;
#27805 = CARTESIAN_POINT ( 'NONE',  ( -16.85343921394901301, 12.09981795542885585, -1.000005633855494125E-09 ) ) ;
#27806 = AXIS2_PLACEMENT_3D ( 'NONE', #21804, #17453, #22503 ) ;
#27807 = PLANE ( 'NONE',  #26834 ) ;
#27808 = FACE_OUTER_BOUND ( 'NONE', #22521, .T. ) ;
#27809 = CARTESIAN_POINT ( 'NONE',  ( 3.389692407805913632, 3.523397910813151679, -48.69426496242499525 ) ) ;
#27810 = CARTESIAN_POINT ( 'NONE',  ( 14.56598578705916225, -22.49203128606118440, -25.22917425849270501 ) ) ;
#27811 = CARTESIAN_POINT ( 'NONE',  ( -27.79539923781770483, -0.5057481688778011630, 1.000000000000000888 ) ) ;
#27812 = DIRECTION ( 'NONE',  ( 1.000000000000000000, -0.000000000000000000, 0.000000000000000000 ) ) ;
#27813 = DIRECTION ( 'NONE',  ( -1.000000000000000000, 0.000000000000000000, 0.000000000000000000 ) ) ;
#27814 = ORIENTED_EDGE ( 'NONE', *, *, #27913, .F. ) ;
#27815 = CARTESIAN_POINT ( 'NONE',  ( 3.155489075140835542, 3.034105443485036968, -35.82341724620001600 ) ) ;
#27816 = EDGE_LOOP ( 'NONE', ( #6265, #5132, #21748, #18806, #9910 ) ) ;
#27817 = CARTESIAN_POINT ( 'NONE',  ( -0.9606962270921419744, -4.447130805931738706, -56.33033560642500248 ) ) ;
#27818 = CIRCLE ( 'NONE', #1193, 1.999999999999999112 ) ;
#27819 = EDGE_LOOP ( 'NONE', ( #8, #14212, #2401, #21758 ) ) ;
#27821 = EDGE_CURVE ( 'NONE', #24850, #15988, #27457, .T. ) ;
#27820 = VECTOR ( 'NONE', #13372, 1000.000000000000114 ) ;
#27822 = CIRCLE ( 'NONE', #26817, 2.999999999999999556 ) ;
#27823 = VERTEX_POINT ( 'NONE', #12665 ) ;
#27824 = ORIENTED_EDGE ( 'NONE', *, *, #10530, .T. ) ;
#27825 = FILL_AREA_STYLE ('',( #23440 ) ) ;
#27826 = CARTESIAN_POINT ( 'NONE',  ( -12.29999999969999891, -27.00000000000000000, -28.40000000020000215 ) ) ;
#27827 = CARTESIAN_POINT ( 'NONE',  ( -17.41915764888113216, -30.48863279055043662, -24.64066038902905831 ) ) ;
#27828 = CARTESIAN_POINT ( 'NONE',  ( 0.000000000000000000, 0.000000000000000000, 90.00000000000000000 ) ) ;
#27829 = PLANE ( 'NONE',  #12076 ) ;
#27830 = PLANE ( 'NONE',  #29020 ) ;
#27831 = CARTESIAN_POINT ( 'NONE',  ( -3.324062773583611907, -4.387625903868788591, -2.728945369300002977 ) ) ;
#27832 = CARTESIAN_POINT ( 'NONE',  ( 1.746002136800675508, 1.009759976939816672, 230.8412452700000017 ) ) ;
#27833 = CARTESIAN_POINT ( 'NONE',  ( -10.69999999999999929, -27.00000000000000000, -25.39999999999999858 ) ) ;
#27834 = CARTESIAN_POINT ( 'NONE',  ( -3.283272085064022239, -5.616145207998583189, -15.68182079290000175 ) ) ;
#27835 = CARTESIAN_POINT ( 'NONE',  ( 5.672553144689285176, -0.9485505809898806540, -35.74517599850000948 ) ) ;
#27836 = AXIS2_PLACEMENT_3D ( 'NONE', #11901, #14116, #30793 ) ;
#27837 = CARTESIAN_POINT ( 'NONE',  ( 2.862882362280000148, -5.240471012860000499, 226.6412452697800006 ) ) ;
#27838 = CARTESIAN_POINT ( 'NONE',  ( 26.79556473285982321, 0.4875557887250580036, -0.6999999999999784173 ) ) ;
#27839 = CARTESIAN_POINT ( 'NONE',  ( 0.6686231747119999458, -28.49266848160000265, 224.0990955869999937 ) ) ;
#27840 = TOROIDAL_SURFACE ( 'NONE', #11276, 5.792819795519999815, 2.000000000000000000 ) ;
#27841 = CARTESIAN_POINT ( 'NONE',  ( 13.21383179760920967, -25.42848403399915469, 8.000000000000007105 ) ) ;
#27842 = FACE_OUTER_BOUND ( 'NONE', #19624, .T. ) ;
#27843 = AXIS2_PLACEMENT_3D ( 'NONE', #26316, #11377, #14366 ) ;
#27844 = VECTOR ( 'NONE', #2430, 1000.000000000000000 ) ;
#27845 = VECTOR ( 'NONE', #5466, 1000.000000000000000 ) ;
#27846 = DIRECTION ( 'NONE',  ( 0.000000000000000000, 0.000000000000000000, -1.000000000000000000 ) ) ;
#27847 = FACE_OUTER_BOUND ( 'NONE', #11534, .T. ) ;
#27848 = CARTESIAN_POINT ( 'NONE',  ( -0.1464386043128553250, -27.80011885101413682, 4.099092748999999536 ) ) ;
#27849 = ORIENTED_EDGE ( 'NONE', *, *, #18694, .T. ) ;
#27850 = ADVANCED_FACE ( 'NONE', ( #19294 ), #14583, .T. ) ;
#27851 = B_SPLINE_CURVE_WITH_KNOTS ( 'NONE', 3,
 ( #10382, #3591, #19973, #24697, #20276, #17452 ),
 .UNSPECIFIED., .F., .F.,
 ( 4, 2, 4 ),
 ( 0.000000000000000000, 0.5000000000000000000, 1.000000000000000000 ),
 .UNSPECIFIED. ) ;
#27852 = CARTESIAN_POINT ( 'NONE',  ( 23.62421573330318836, 14.65442405561991634, 6.042470792000015578 ) ) ;
#27853 = CARTESIAN_POINT ( 'NONE',  ( -3.061185584113674807, -2.905325888027505687, -69.93578169304477399 ) ) ;
#27854 = EDGE_LOOP ( 'NONE', ( #2410, #16486, #23970, #2252 ) ) ;
#27855 = LINE ( 'NONE', #8809, #23400 ) ;
#27856 = CARTESIAN_POINT ( 'NONE',  ( 4.006286404973145032, 0.3445522835526793060, -37.64721854827592296 ) ) ;
#27857 = CARTESIAN_POINT ( 'NONE',  ( -8.699999998944143442, -13.61360970150653316, -34.64062719139432289 ) ) ;
#27858 = VERTEX_POINT ( 'NONE', #21811 ) ;
#27859 = CARTESIAN_POINT ( 'NONE',  ( -2.107992564109736566, -27.41908764619380889, 20.00000000000000355 ) ) ;
#27860 = ORIENTED_EDGE ( 'NONE', *, *, #14934, .F. ) ;
#27861 = EDGE_CURVE ( 'NONE', #26129, #26103, #15041, .T. ) ;
#27862 = ORIENTED_EDGE ( 'NONE', *, *, #11036, .F. ) ;
#27863 = VERTEX_POINT ( 'NONE', #21971 ) ;
#27864 = CARTESIAN_POINT ( 'NONE',  ( 22.54750148980000191, 18.07861229659999935, 229.2404163060000144 ) ) ;
#27865 = AXIS2_PLACEMENT_3D ( 'NONE', #25341, #15273, #3782 ) ;
#27866 = VERTEX_POINT ( 'NONE', #26833 ) ;
#27868 = CARTESIAN_POINT ( 'NONE',  ( 10.69999999999999929, -30.00000000000000000, -28.40000000000000213 ) ) ;
#27867 = AXIS2_PLACEMENT_3D ( 'NONE', #29633, #9982, #26810 ) ;
#27869 = ORIENTED_EDGE ( 'NONE', *, *, #29999, .F. ) ;
#27870 = CARTESIAN_POINT ( 'NONE',  ( 2.653975030832389059, 2.820913939037494433, -35.69999999999999574 ) ) ;
#27871 = CIRCLE ( 'NONE', #5256, 4.000000000000001776 ) ;
#27872 = CARTESIAN_POINT ( 'NONE',  ( 0.000000000000000000, 0.000000000000000000, 115.0000000000000000 ) ) ;
#27873 = CARTESIAN_POINT ( 'NONE',  ( -26.84464185210000053, 3.287411897809999814E-15, 137.4375040469999760 ) ) ;
#27874 = DIRECTION ( 'NONE',  ( -1.000000000000000000, 5.063197467948052462E-16, -2.257212216284997029E-12 ) ) ;
#27875 = CARTESIAN_POINT ( 'NONE',  ( 23.88966196158443367, -14.21810147650477596, 4.317391451927520940 ) ) ;
#27876 = ADVANCED_FACE ( 'NONE', ( #19914 ), #14572, .F. ) ;
#27877 = EDGE_LOOP ( 'NONE', ( #30935, #29658, #11763, #24082 ) ) ;
#27878 = EDGE_CURVE ( 'NONE', #8194, #24363, #12868, .T. ) ;
#27879 = CARTESIAN_POINT ( 'NONE',  ( -1.531656806707240248, -4.518636249346831946, -1.513130512700005426 ) ) ;
#27880 = CARTESIAN_POINT ( 'NONE',  ( -4.217400109093552452, 2.917745507991547971, -24.53029765530000006 ) ) ;
#27881 = CARTESIAN_POINT ( 'NONE',  ( -6.984668861240823645, -26.60192251835760757, 208.3914686747987162 ) ) ;
#27882 = AXIS2_PLACEMENT_3D ( 'NONE', #21805, #264, #10002 ) ;
#27883 = CARTESIAN_POINT ( 'NONE',  ( 24.37450210455010335, -13.36961646745188759, 6.095967861000000987 ) ) ;
#27884 = CARTESIAN_POINT ( 'NONE',  ( -27.54391550559999757, 3.373045393730000103E-15, 137.0437466829999948 ) ) ;
#27885 = CARTESIAN_POINT ( 'NONE',  ( -27.04041630560000087, 4.559430447050000446, 230.6999999999999886 ) ) ;
#27886 = CARTESIAN_POINT ( 'NONE',  ( -1.861312627829582400, -21.81692582113286960, -30.17614928725744150 ) ) ;
#27887 = CARTESIAN_POINT ( 'NONE',  ( 9.999999999989825028, -129.7569854622061882, -38.71642352353225647 ) ) ;
#27888 = CARTESIAN_POINT ( 'NONE',  ( 24.14619884819310158, -13.16136950074017875, 224.1195089971002972 ) ) ;
#27889 = CARTESIAN_POINT ( 'NONE',  ( 13.76031882590000066, 12.03543611500000132, 230.6999999999999886 ) ) ;
#27890 = CARTESIAN_POINT ( 'NONE',  ( -17.80313299384375370, 11.53824530455753283, -0.6999999999999785283 ) ) ;
#27891 = ORIENTED_EDGE ( 'NONE', *, *, #5949, .F. ) ;
#27892 = CARTESIAN_POINT ( 'NONE',  ( 4.009291712408942665, -2.091746824018185347, -60.91790713612499530 ) ) ;
#27893 = CARTESIAN_POINT ( 'NONE',  ( -11.45957740435848926, -24.29669185712474899, 36.78285841129289224 ) ) ;
#27894 = VERTEX_POINT ( 'NONE', #10620 ) ;
#27895 = CIRCLE ( 'NONE', #16839, 10.00564797610000056 ) ;
#27896 = CARTESIAN_POINT ( 'NONE',  ( 1.403799475828179766, 5.569137675590418723, -17.05080441500000177 ) ) ;
#27897 = EDGE_LOOP ( 'NONE', ( #13939, #15741, #12337, #17488 ) ) ;
#27898 = CARTESIAN_POINT ( 'NONE',  ( -25.17394274020000111, -13.36230406159999973, 225.5071265450000055 ) ) ;
#27899 = EDGE_CURVE ( 'NONE', #20193, #4001, #27446, .T. ) ;
#27900 = CARTESIAN_POINT ( 'NONE',  ( -3.957406504849845241, -0.8124326615230210713, -68.10000000002500542 ) ) ;
#27901 = ORIENTED_EDGE ( 'NONE', *, *, #29615, .F. ) ;
#27902 = ORIENTED_EDGE ( 'NONE', *, *, #19217, .T. ) ;
#27903 = EDGE_LOOP ( 'NONE', ( #2177, #22677, #5007, #3552, #2313, #2561 ) ) ;
#27904 = CARTESIAN_POINT ( 'NONE',  ( 10.69999999999999929, -29.30501631380000305, -26.47986985000000004 ) ) ;
#27905 = B_SPLINE_CURVE_WITH_KNOTS ( 'NONE', 5,
 ( #29003, #2426, #14855, #28841, #21623, #26797 ),
 .UNSPECIFIED., .F., .F.,
 ( 6, 6 ),
 ( 0.000000000000000000, 2.300779637660000265 ),
 .UNSPECIFIED. ) ;
#27906 = APPLICATION_PROTOCOL_DEFINITION ( 'draft international standard', 'automotive_design', 1998, #30060 ) ;
#27907 = VERTEX_POINT ( 'NONE', #15343 ) ;
#27908 = CARTESIAN_POINT ( 'NONE',  ( -10.00000000012699886, 8.682826176890005243, 14.90608581627787110 ) ) ;
#27909 = VECTOR ( 'NONE', #30086, 1000.000000000000000 ) ;
#27910 =( GEOMETRIC_REPRESENTATION_CONTEXT ( 3 ) GLOBAL_UNCERTAINTY_ASSIGNED_CONTEXT ( ( #17225 ) ) GLOBAL_UNIT_ASSIGNED_CONTEXT ( ( #15586, #1753, #15744 ) ) REPRESENTATION_CONTEXT ( 'NONE', 'WORKASPACE' ) );
#27911 = CARTESIAN_POINT ( 'NONE',  ( 0.000000000000000000, -1.776356839399999804E-15, 227.6412452697800006 ) ) ;
#27912 = CARTESIAN_POINT ( 'NONE',  ( 1.353924481083393028, -4.675650134241364775, -66.95367649362499662 ) ) ;
#27913 = EDGE_CURVE ( 'NONE', #16428, #24430, #25338, .T. ) ;
#27914 = CARTESIAN_POINT ( 'NONE',  ( 27.24857305709999977, -7.138312704079999627, 229.9172022069999741 ) ) ;
#27915 = CARTESIAN_POINT ( 'NONE',  ( -18.97090238747512458, 21.26865671932805313, 0.7595836940000044724 ) ) ;
#27916 = CARTESIAN_POINT ( 'NONE',  ( 10.70000000070000112, 19.99999999999999645, -42.59161006100999458 ) ) ;
#27917 = EDGE_CURVE ( 'NONE', #30789, #17667, #6048, .T. ) ;
#27918 = CARTESIAN_POINT ( 'NONE',  ( -23.81776757772072983, -15.65134804123479917, 4.999998581000003384 ) ) ;
#27919 = VERTEX_POINT ( 'NONE', #22898 ) ;
#27920 = DIRECTION ( 'NONE',  ( 0.000000000000000000, 0.000000000000000000, -1.000000000000000000 ) ) ;
#27921 = CARTESIAN_POINT ( 'NONE',  ( -3.941349475653407985, -1.876729865818548282, -12.47655742010000068 ) ) ;
#27922 = CARTESIAN_POINT ( 'NONE',  ( -27.15000000039999861, 3.324806250669999651E-15, 230.0000000000000000 ) ) ;
#27923 = EDGE_CURVE ( 'NONE', #21696, #19663, #21850, .T. ) ;
#27924 = CARTESIAN_POINT ( 'NONE',  ( -0.2818134472887923181, -12.32633712609394294, 232.6627637456880677 ) ) ;
#27925 = EDGE_LOOP ( 'NONE', ( #28907, #15985, #27699, #14690, #30732, #17959 ) ) ;
#27926 = LINE ( 'NONE', #20852, #21729 ) ;
#27927 = CARTESIAN_POINT ( 'NONE',  ( 0.000000000000000000, 20.99999999999999645, -44.10000000017154065 ) ) ;
#27928 = PRODUCT_RELATED_PRODUCT_CATEGORY ( 'part', '', ( #30511 ) ) ;
#27929 = CARTESIAN_POINT ( 'NONE',  ( -8.699999999685100960, -16.20661859040315989, -33.02459860127090252 ) ) ;
#27930 = CARTESIAN_POINT ( 'NONE',  ( 26.68292649568627084, 9.659560297568411613, 1.000000000000000888 ) ) ;
#27931 = CARTESIAN_POINT ( 'NONE',  ( -23.67167941903505479, -13.99714051993850461, 3.928090679417475695 ) ) ;
#27932 = CARTESIAN_POINT ( 'NONE',  ( -17.62526623054365871, -8.236462051082252600, 0.000000000000000000 ) ) ;
#27933 = CARTESIAN_POINT ( 'NONE',  ( -11.57608395609999974, -24.17108566160000294, -0.7028182529999968953 ) ) ;
#27934 = DIRECTION ( 'NONE',  ( -0.8660254037843289066, -0.5000000000001899592, 0.000000000000000000 ) ) ;
#27935 = VERTEX_POINT ( 'NONE', #10773 ) ;
#27936 = CARTESIAN_POINT ( 'NONE',  ( 23.92481352790954929, -14.15879618172946408, 4.239732040000027347 ) ) ;
#27937 = CARTESIAN_POINT ( 'NONE',  ( 18.26639035964474900, 11.02001161816309072, -1.000005633855494125E-09 ) ) ;
#27938 = CARTESIAN_POINT ( 'NONE',  ( 1.858630010972899704, -3.718756527810015644, -68.10000000002501963 ) ) ;
#27939 = ADVANCED_FACE ( 'NONE', ( #20374 ), #1502, .F. ) ;
#27940 = DIRECTION ( 'NONE',  ( -1.000000000000000000, 3.981000000000000101E-12, -1.940999999999999908E-12 ) ) ;
#27941 = CARTESIAN_POINT ( 'NONE',  ( -3.694857771750023279, -1.477660183791897008, -44.10000000002497700 ) ) ;
#27942 = EDGE_CURVE ( 'NONE', #13120, #6070, #13793, .T. ) ;
#27943 = CARTESIAN_POINT ( 'NONE',  ( 7.707106781468556100, -5.692566302608600637, -27.29492475672613594 ) ) ;
#27944 = CARTESIAN_POINT ( 'NONE',  ( 10.93831327714496204, 21.69999999997515516, -55.10899305193176900 ) ) ;
#27945 = CARTESIAN_POINT ( 'NONE',  ( 3.705709820302785396, 4.685590126413917034, -64.11768011632500475 ) ) ;
#27946 = VERTEX_POINT ( 'NONE', #18157 ) ;
#27947 = ADVANCED_FACE ( 'NONE', ( #20528 ), #27762, .T. ) ;
#27948 = CARTESIAN_POINT ( 'NONE',  ( -1.100000000000000089, -27.47799119230000287, 5.000000000000000000 ) ) ;
#27949 = VERTEX_POINT ( 'NONE', #4009 ) ;
#27950 = CARTESIAN_POINT ( 'NONE',  ( -17.99591469510000152, 19.96082041680000074, 229.9999991770000065 ) ) ;
#27951 = ORIENTED_EDGE ( 'NONE', *, *, #15559, .F. ) ;
#27952 = DIRECTION ( 'NONE',  ( 0.000000000000000000, -0.9128796883888953273, 0.4082287037029528332 ) ) ;
#27953 = CARTESIAN_POINT ( 'NONE',  ( -26.80000000069999899, 3.281945028329999726E-15, 165.0000000000000000 ) ) ;
#27954 = CARTESIAN_POINT ( 'NONE',  ( -12.68067472840826682, 21.69999999999972218, -56.02822601348136544 ) ) ;
#27955 = CARTESIAN_POINT ( 'NONE',  ( -3.145769537975008578, -1.551367331319410514, 230.8336439985933453 ) ) ;
#27956 = CARTESIAN_POINT ( 'NONE',  ( -0.5968465743326634154, -28.49391676915515603, 4.791896188000022150 ) ) ;
#27957 = CARTESIAN_POINT ( 'NONE',  ( -16.34545256226243382, -9.995493785995851255, 0.000000000000000000 ) ) ;
#27958 = CARTESIAN_POINT ( 'NONE',  ( -17.19097361924276868, -22.00024499056281613, -26.04210681964482887 ) ) ;
#27959 = EDGE_LOOP ( 'NONE', ( #28449, #23306 ) ) ;
#27960 = CARTESIAN_POINT ( 'NONE',  ( -4.000000000000000000, -29.96004123392021157, -79.78289277550334191 ) ) ;
#27961 = CARTESIAN_POINT ( 'NONE',  ( 27.75695160390876737, 2.618790587933454983, 8.000000000000007105 ) ) ;
#27962 = DIRECTION ( 'NONE',  ( -0.7071067811870476172, 0.000000000000000000, 0.7071067811860475283 ) ) ;
#27963 = DIRECTION ( 'NONE',  ( -1.000000000000000000, 9.219999999999999084E-13, -4.710999999999999616E-12 ) ) ;
#27964 = CARTESIAN_POINT ( 'NONE',  ( 18.63941909573550859, 10.97998838177520931, -1.972246272986471594 ) ) ;
#27965 = CARTESIAN_POINT ( 'NONE',  ( -17.49999999969999820, -27.00000000000000355, -34.17350269210000135 ) ) ;
#27966 = CARTESIAN_POINT ( 'NONE',  ( 23.35349940196098828, 15.08195766973940266, 4.323494425288421539 ) ) ;
#27967 = FACE_OUTER_BOUND ( 'NONE', #334, .T. ) ;
#27968 = CARTESIAN_POINT ( 'NONE',  ( -3.108138112192390778, -3.359256988581870385, -50.19612412472499585 ) ) ;
#27969 = CARTESIAN_POINT ( 'NONE',  ( -23.76736455408141069, -13.83371703036772615, 6.100000000001124079 ) ) ;
#27970 = CARTESIAN_POINT ( 'NONE',  ( 7.635581859131290727, 4.027124264807724785, -39.44332891327358226 ) ) ;
#27971 = CARTESIAN_POINT ( 'NONE',  ( 2.557450677934476779, -2.570068162742275231, 230.7636321640558208 ) ) ;
#27972 = ADVANCED_FACE ( 'NONE', ( #13923 ), #28229, .T. ) ;
#27973 = CARTESIAN_POINT ( 'NONE',  ( -0.6425564543738772061, -27.49266737062499999, 224.0869147246957027 ) ) ;
#27974 = ORIENTED_EDGE ( 'NONE', *, *, #23844, .T. ) ;
#27975 = ADVANCED_FACE ( 'NONE', ( #13759 ), #21841, .T. ) ;
#27976 = LINE ( 'NONE', #23585, #1896 ) ;
#27977 = EDGE_CURVE ( 'NONE', #14134, #669, #22236, .T. ) ;
#27978 = EDGE_LOOP ( 'NONE', ( #29830, #23675, #22532, #20349 ) ) ;
#27979 = CARTESIAN_POINT ( 'NONE',  ( -5.939015604524707115, -0.1501891088408410790, -54.03673954922499689 ) ) ;
#27980 = VERTEX_POINT ( 'NONE', #31065 ) ;
#27981 = PRODUCT_CONTEXT ( 'NONE', #12183, 'mechanical' ) ;
#27982 = EDGE_LOOP ( 'NONE', ( #9348, #29985, #14223, #9126 ) ) ;
#27983 = VERTEX_POINT ( 'NONE', #4325 ) ;
#27984 = DIRECTION ( 'NONE',  ( -2.764840495839172918E-12, -0.9128796883888953273, 0.4082287037029530552 ) ) ;
#27985 = DIRECTION ( 'NONE',  ( -0.8090169943751909232, 0.5877852522921378498, 0.000000000000000000 ) ) ;
#27986 = AXIS2_PLACEMENT_3D ( 'NONE', #29026, #17068, #12498 ) ;
#27987 = DIRECTION ( 'NONE',  ( 0.3633921898465291567, 0.9316362575375349842, 5.551115123125783333E-14 ) ) ;
#27988 = DIRECTION ( 'NONE',  ( -1.000000000000000000, 0.000000000000000000, 0.000000000000000000 ) ) ;
#27989 = CARTESIAN_POINT ( 'NONE',  ( -4.757675747652303500, -1.918655839533711660, -0.05969743450000113139 ) ) ;
#27990 = PRESENTATION_LAYER_ASSIGNMENT (  '', '', ( #19464 ) ) ;
#27991 = CARTESIAN_POINT ( 'NONE',  ( -9.999999999969999109, -29.12127062080000073, -30.52127062269999769 ) ) ;
#27992 = DIRECTION ( 'NONE',  ( 0.000000000000000000, 0.000000000000000000, -1.000000000000000000 ) ) ;
#27993 = CARTESIAN_POINT ( 'NONE',  ( 4.315341029122434335, -4.279276102762477940, -15.66112212870000242 ) ) ;
#27994 = CARTESIAN_POINT ( 'NONE',  ( -0.3609073012553025150, 5.149274899367955349, -33.95768930509999706 ) ) ;
#27995 = CARTESIAN_POINT ( 'NONE',  ( -12.77820031409999935, 21.69999999929999390, -56.09999999999999432 ) ) ;
#27996 = EDGE_CURVE ( 'NONE', #9398, #13706, #28545, .T. ) ;
#27997 = CARTESIAN_POINT ( 'NONE',  ( 28.54410101353736806, -9.901582551596423087, 0.2374258030000131470 ) ) ;
#27998 = LINE ( 'NONE', #1421, #13646 ) ;
#27999 = CARTESIAN_POINT ( 'NONE',  ( -7.974365406319376071, -26.79131034418178814, 8.000000000000007105 ) ) ;
#28000 = DIRECTION ( 'NONE',  ( -0.000000000000000000, -0.000000000000000000, 1.000000000000000000 ) ) ;
#28001 = ADVANCED_FACE ( 'NONE', ( #9504 ), #25730, .F. ) ;
#28002 = B_SPLINE_CURVE_WITH_KNOTS ( 'NONE', 3,
 ( #3491, #15609, #10436, #13242, #20028, #29467, #7903, #29932, #27565, #22698 ),
 .UNSPECIFIED., .F., .F.,
 ( 4, 2, 2, 2, 4 ),
 ( 0.000000000000000000, 0.2500000000000000000, 0.5000000000000000000, 0.7500000000000000000, 1.000000000000000000 ),
 .UNSPECIFIED. ) ;
#28003 = CARTESIAN_POINT ( 'NONE',  ( 27.21178567695783812, 4.999345137307622089, -0.6577119969999878357 ) ) ;
#28004 = CARTESIAN_POINT ( 'NONE',  ( -0.9931698613850974411, -3.387288372825724814, 226.6412452697749984 ) ) ;
#28005 = CARTESIAN_POINT ( 'NONE',  ( -22.97593529893700648, 15.65128280014837081, 8.000000000000007105 ) ) ;
#28006 = PRESENTATION_LAYER_ASSIGNMENT (  '', '', ( #5899 ) ) ;
#28007 = CARTESIAN_POINT ( 'NONE',  ( -10.69999999999999929, -77.50000000000000000, -29.00566191750000300 ) ) ;
#28008 = EDGE_LOOP ( 'NONE', ( #13727, #23739, #29402, #14491 ) ) ;
#28009 = AXIS2_PLACEMENT_3D ( 'NONE', #25127, #22462, #10194 ) ;
#28010 = DIRECTION ( 'NONE',  ( 0.000000000000000000, 0.000000000000000000, -1.000000000000000000 ) ) ;
#28011 = CARTESIAN_POINT ( 'NONE',  ( -24.60699806910000120, -12.93667933180000063, 224.8957833819999621 ) ) ;
#28012 = CARTESIAN_POINT ( 'NONE',  ( 9.999999999952072116, -31.36353147791090379, -21.95991608839452880 ) ) ;
#28013 = ORIENTED_EDGE ( 'NONE', *, *, #25408, .F. ) ;
#28014 = CARTESIAN_POINT ( 'NONE',  ( 10.00000000000000000, 22.40709319595134730, -62.85117013414870257 ) ) ;
#28015 = EDGE_LOOP ( 'NONE', ( #3800, #707, #16527 ) ) ;
#28016 = ORIENTED_EDGE ( 'NONE', *, *, #1596, .F. ) ;
#28017 = VERTEX_POINT ( 'NONE', #30453 ) ;
#28018 = CARTESIAN_POINT ( 'NONE',  ( 2.131628207279999844E-14, -1.704192342799999938E-14, 230.0904314459999966 ) ) ;
#28019 = ORIENTED_EDGE ( 'NONE', *, *, #8610, .F. ) ;
#28020 = CARTESIAN_POINT ( 'NONE',  ( -22.83911234509999844, 16.42879871570000105, 229.0000000010000178 ) ) ;
#28021 = CARTESIAN_POINT ( 'NONE',  ( 8.700000000276082446, -16.84110654130126150, -33.19737377701691372 ) ) ;
#28022 = DIRECTION ( 'NONE',  ( 0.000000000000000000, 0.000000000000000000, 1.000000000000000000 ) ) ;
#28023 = CARTESIAN_POINT ( 'NONE',  ( -6.835848593969952702, 5.804179925720610811, -40.31005687079623812 ) ) ;
#28024 = CARTESIAN_POINT ( 'NONE',  ( 14.48117849943559499, -22.00000000000000000, -25.78761638283549118 ) ) ;
#28025 = CARTESIAN_POINT ( 'NONE',  ( 23.72659782635170700, -12.46160334561661109, 5.288095983042272685 ) ) ;
#28026 = CARTESIAN_POINT ( 'NONE',  ( 24.32472724076343695, -13.45989056521276872, 3.899998581000013509 ) ) ;
#28027 = ADVANCED_FACE ( 'NONE', ( #30609 ), #30914, .F. ) ;
#28028 = EDGE_LOOP ( 'NONE', ( #5489, #11497 ) ) ;
#28029 = AXIS2_PLACEMENT_3D ( 'NONE', #8500, #28329, #4106 ) ;
#28030 = CARTESIAN_POINT ( 'NONE',  ( -3.673964118181757943, -4.849481262180703744, -3.728945369300004753 ) ) ;
#28031 = CARTESIAN_POINT ( 'NONE',  ( 0.2925910193319765096, 5.520737601085913937, -21.94418644580000688 ) ) ;
#28032 = CARTESIAN_POINT ( 'NONE',  ( -9.594426947539474781, -25.77213547066687127, 204.5919004740421485 ) ) ;
#28033 = VECTOR ( 'NONE', #25834, 1000.000000000000000 ) ;
#28034 = CARTESIAN_POINT ( 'NONE',  ( -3.528982507896216703, 0.08581763272074406645, -91.06246442329681656 ) ) ;
#28035 = CYLINDRICAL_SURFACE ( 'NONE', #7687, 1.700000000000000178 ) ;
#28036 = CARTESIAN_POINT ( 'NONE',  ( 0.000000000000000000, 0.000000000000000000, 140.0000000000000000 ) ) ;
#28037 = CARTESIAN_POINT ( 'NONE',  ( -24.09883371379999772, -15.21565466309999870, 225.1042187089999800 ) ) ;
#28038 = EDGE_CURVE ( 'NONE', #23898, #11807, #9466, .T. ) ;
#28039 = CARTESIAN_POINT ( 'NONE',  ( -7.999999999691694619, -25.92947359974649046, -31.20249410826873415 ) ) ;
#28040 = DIRECTION ( 'NONE',  ( -1.000000000000000000, 0.000000000000000000, 0.000000000000000000 ) ) ;
#28041 = CARTESIAN_POINT ( 'NONE',  ( -13.65679423271931903, -23.08581637699097655, -1.399999999999998579 ) ) ;
#28042 = EDGE_LOOP ( 'NONE', ( #10411, #24126, #14553, #27544, #10342 ) ) ;
#28043 = CARTESIAN_POINT ( 'NONE',  ( 5.242919931573567283, -2.735361231296036699, -61.31790713612500099 ) ) ;
#28044 = CARTESIAN_POINT ( 'NONE',  ( -12.29999999974999803, -27.00000000000000000, -28.40000000020000215 ) ) ;
#28045 = ORIENTED_EDGE ( 'NONE', *, *, #7194, .T. ) ;
#28046 = AXIS2_PLACEMENT_3D ( 'NONE', #4229, #6582, #14299 ) ;
#28047 = ORIENTED_EDGE ( 'NONE', *, *, #5548, .F. ) ;
#28048 = CARTESIAN_POINT ( 'NONE',  ( -26.80000000000000071, 1.065814103639999922E-14, 86.78285841159998881 ) ) ;
#28049 = CARTESIAN_POINT ( 'NONE',  ( 6.118976883090258667, 2.212479739890888197, -26.51249766020000109 ) ) ;
#28050 = ORIENTED_EDGE ( 'NONE', *, *, #795, .F. ) ;
#28051 = CARTESIAN_POINT ( 'NONE',  ( -24.91946588839999777, -13.83134141909999926, 226.0028092389999870 ) ) ;
#28052 = CARTESIAN_POINT ( 'NONE',  ( 18.95046173579999760, -18.95046173579999760, 186.7828584120000244 ) ) ;
#28053 = ORIENTED_EDGE ( 'NONE', *, *, #13491, .F. ) ;
#28054 = EDGE_CURVE ( 'NONE', #24719, #1905, #28699, .T. ) ;
#28055 = ORIENTED_EDGE ( 'NONE', *, *, #25806, .T. ) ;
#28056 = ORIENTED_EDGE ( 'NONE', *, *, #19079, .F. ) ;
#28057 = DIRECTION ( 'NONE',  ( -1.553791817432425509E-12, 0.7253743710120286181, -0.6883545756940269156 ) ) ;
#28058 = ORIENTED_EDGE ( 'NONE', *, *, #11751, .T. ) ;
#28059 = CARTESIAN_POINT ( 'NONE',  ( -12.30000000031408725, -29.79611644273363424, -30.01158073719770414 ) ) ;
#28060 = VECTOR ( 'NONE', #12740, 1000.000000000000227 ) ;
#28061 = ADVANCED_FACE ( 'NONE', ( #6673 ), #257, .F. ) ;
#28062 = DIRECTION ( 'NONE',  ( 0.3633921898465291567, 0.9316362575375348731, -0.000000000000000000 ) ) ;
#28063 = CARTESIAN_POINT ( 'NONE',  ( -1.084269253894827534, -5.810518403417324507, -67.90745670422499813 ) ) ;
#28064 = CARTESIAN_POINT ( 'NONE',  ( 24.91104292519999674, -14.27662681390000010, 229.9172020129999794 ) ) ;
#28065 = LINE ( 'NONE', #3998, #22210 ) ;
#28066 = CARTESIAN_POINT ( 'NONE',  ( 8.460443391580000139, -26.64180382800000046, 222.0000000000000000 ) ) ;
#28067 = CARTESIAN_POINT ( 'NONE',  ( -23.31845629847328993, -13.20933888637554254, 6.087620939417903720 ) ) ;
#28068 = EDGE_LOOP ( 'NONE', ( #2194, #3953, #2331 ) ) ;
#28069 = CARTESIAN_POINT ( 'NONE',  ( -20.30403093151401706, 20.00000000001585221, 0.8732882910316148717 ) ) ;
#28070 = VECTOR ( 'NONE', #24356, 1000.000000000000114 ) ;
#28071 = CARTESIAN_POINT ( 'NONE',  ( 5.466312515054250198, -2.792605348973308477, -11.31474735219999772 ) ) ;
#28072 = CARTESIAN_POINT ( 'NONE',  ( 26.80000000069999899, -3.281945028320000125E-15, 136.7828584130000138 ) ) ;
#28073 = CARTESIAN_POINT ( 'NONE',  ( 6.422810853499230532, 10.52452000602716708, 232.6627635423665481 ) ) ;
#28074 = VERTEX_POINT ( 'NONE', #2734 ) ;
#28075 = FACE_OUTER_BOUND ( 'NONE', #4918, .T. ) ;
#28076 = CARTESIAN_POINT ( 'NONE',  ( 0.9758793680739014098, -27.78334643823060546, 3.997481721999984750 ) ) ;
#28077 = CARTESIAN_POINT ( 'NONE',  ( 18.26375984408715425, 11.16458205341174192, -0.6999999999999783062 ) ) ;
#28078 = EDGE_CURVE ( 'NONE', #27427, #25385, #30896, .T. ) ;
#28079 = CARTESIAN_POINT ( 'NONE',  ( 27.52676963214412353, 0.5008603480660110963, 0.2686740700000300741 ) ) ;
#28080 = CARTESIAN_POINT ( 'NONE',  ( 22.75778669649943353, -14.15360906249806128, 4.333923913290392171 ) ) ;
#28081 = CARTESIAN_POINT ( 'NONE',  ( 1.169850847344618083, -6.301966510834352775, -58.74125695792500323 ) ) ;
#28082 = AXIS2_PLACEMENT_3D ( 'NONE', #29543, #9730, #27033 ) ;
#28083 = CARTESIAN_POINT ( 'NONE',  ( -23.25311087912443853, -15.23597700045676895, 5.310552105000033052 ) ) ;
#28084 = DIRECTION ( 'NONE',  ( 0.000000000000000000, 0.3420201433259318913, -0.9396926207858126157 ) ) ;
#28085 = VERTEX_POINT ( 'NONE', #7451 ) ;
#28086 = CARTESIAN_POINT ( 'NONE',  ( 24.30808045080437907, -13.48997717272881047, 3.899998581000013509 ) ) ;
#28087 = CARTESIAN_POINT ( 'NONE',  ( -8.700000000014243895, -117.3672015282731280, 16.33620429947759334 ) ) ;
#28088 =( REPRESENTATION_RELATIONSHIP ('NONE','NONE', #2712, #527 ) REPRESENTATION_RELATIONSHIP_WITH_TRANSFORMATION ( #7808 )SHAPE_REPRESENTATION_RELATIONSHIP( ) );
#28089 = CARTESIAN_POINT ( 'NONE',  ( 2.132677846510928177, -3.629065541562336961, -68.10000000002500542 ) ) ;
#28090 = EDGE_CURVE ( 'NONE', #7936, #25188, #4952, .T. ) ;
#28091 = AXIS2_PLACEMENT_3D ( 'NONE', #21497, #22117, #29339 ) ;
#28092 = EDGE_CURVE ( 'NONE', #28151, #19704, #14857, .T. ) ;
#28093 = CARTESIAN_POINT ( 'NONE',  ( 2.063649162913283597, 2.140644056835441233, -68.09919883011119168 ) ) ;
#28094 = CARTESIAN_POINT ( 'NONE',  ( -3.753535784774050921, -1.349497875818973291, -44.10000000002498410 ) ) ;
#28095 = VERTEX_POINT ( 'NONE', #7902 ) ;
#28097 = CARTESIAN_POINT ( 'NONE',  ( -11.28020519024417823, 4.977446647725678019, 232.6627637660202765 ) ) ;
#28096 = B_SPLINE_CURVE_WITH_KNOTS ( 'NONE', 3,
 ( #3074, #12672, #5439, #7946, #276, #19768, #12369, #26999, #29047, #7796, #22279, #26843 ),
 .UNSPECIFIED., .F., .F.,
 ( 4, 2, 2, 2, 2, 4 ),
 ( 0.000000000000000000, 0.2500000000000012768, 0.3750000000000011657, 0.5000000000000011102, 0.7500000000000005551, 1.000000000000000000 ),
 .UNSPECIFIED. ) ;
#28098 = CARTESIAN_POINT ( 'NONE',  ( 2.708949881112997282, 3.684664522020660193, -66.64226422532500749 ) ) ;
#28099 = ORIENTED_EDGE ( 'NONE', *, *, #26296, .T. ) ;
#28100 = CARTESIAN_POINT ( 'NONE',  ( -24.49999999589999788, 3.000285566369999841E-15, 190.0000000000000000 ) ) ;
#28101 = ADVANCED_FACE ( 'NONE', ( #19259 ), #9791, .F. ) ;
#28102 = AXIS2_PLACEMENT_3D ( 'NONE', #4276, #23480, #28336 ) ;
#28103 = ORIENTED_EDGE ( 'NONE', *, *, #18072, .T. ) ;
#28104 = CARTESIAN_POINT ( 'NONE',  ( -26.66783967069105898, -7.507193849635574345, 0.000000000000000000 ) ) ;
#28105 = ORIENTED_EDGE ( 'NONE', *, *, #17146, .T. ) ;
#28106 = LINE ( 'NONE', #21033, #10026 ) ;
#28107 = AXIS2_PLACEMENT_3D ( 'NONE', #12780, #13077, #22079 ) ;
#28108 = LINE ( 'NONE', #27953, #23106 ) ;
#28109 = DIRECTION ( 'NONE',  ( -1.224606353819999829E-16, -1.000000000000000000, 0.000000000000000000 ) ) ;
#28110 = CARTESIAN_POINT ( 'NONE',  ( -3.448453739143383601, 0.7497105383095263864, 0.000000000000000000 ) ) ;
#28111 = CARTESIAN_POINT ( 'NONE',  ( 0.4125558677724673329, -28.49726274111925761, 3.904047916000019658 ) ) ;
#28112 = EDGE_CURVE ( 'NONE', #8534, #27661, #13208, .T. ) ;
#28113 = DIRECTION ( 'NONE',  ( 1.000000000000000000, -3.981005269678786617E-12, 1.941197879946729322E-12 ) ) ;
#28114 = DIRECTION ( 'NONE',  ( 0.000000000000000000, 1.000000000000000000, 0.000000000000000000 ) ) ;
#28115 = VERTEX_POINT ( 'NONE', #14546 ) ;
#28116 = CARTESIAN_POINT ( 'NONE',  ( 0.000000000000000000, 0.000000000000000000, -0.6999999999999784173 ) ) ;
#28117 = CARTESIAN_POINT ( 'NONE',  ( 24.64642659020000082, -14.31106159850000026, 226.0986569330000293 ) ) ;
#28118 = CARTESIAN_POINT ( 'NONE',  ( 19.18299057799999829, 20.00000421109999849, 230.4461458050000147 ) ) ;
#28119 = DIRECTION ( 'NONE',  ( -1.000000000000000000, 5.687697913155423197E-16, -6.771501495041734442E-12 ) ) ;
#28120 = CARTESIAN_POINT ( 'NONE',  ( 3.510330246760000161, 1.917702155199998870, -44.10000000000000142 ) ) ;
#28121 = CARTESIAN_POINT ( 'NONE',  ( 12.09065967409999942, -0.9322763432880000201, 230.6412452697800006 ) ) ;
#28122 = B_SPLINE_CURVE_WITH_KNOTS ( 'NONE', 3,
 ( #27649, #10832, #24680, #22631, #20576, #15084, #19956, #15385 ),
 .UNSPECIFIED., .F., .F.,
 ( 4, 2, 2, 4 ),
 ( 0.000000000000000000, 0.2500000000000000000, 0.5000000000000000000, 1.000000000000000000 ),
 .UNSPECIFIED. ) ;
#28123 = CARTESIAN_POINT ( 'NONE',  ( 23.23277120357798964, 15.26692725135965745, 4.999998581000003384 ) ) ;
#28124 = CARTESIAN_POINT ( 'NONE',  ( -17.79876841479999783, 11.52736809289999620, -1.399999999999998579 ) ) ;
#28125 = CARTESIAN_POINT ( 'NONE',  ( 5.329043336022200705, 2.363500563244980590, -51.07998794302500301 ) ) ;
#28126 = EDGE_CURVE ( 'NONE', #4970, #12999, #5395, .T. ) ;
#28127 = AXIS2_PLACEMENT_3D ( 'NONE', #27209, #25603, #27952 ) ;
#28128 = CARTESIAN_POINT ( 'NONE',  ( 25.46368747440213198, -12.80129684534102807, 4.999998581000003384 ) ) ;
#28129 = CARTESIAN_POINT ( 'NONE',  ( 14.73935963153661532, -28.29773402607040467, -33.42426426252703919 ) ) ;
#28130 = CARTESIAN_POINT ( 'NONE',  ( -17.49164322995629917, 10.10662636424719807, 0.000000000000000000 ) ) ;
#28131 = DIRECTION ( 'NONE',  ( 0.000000000000000000, 0.000000000000000000, -1.000000000000000000 ) ) ;
#28132 = ORIENTED_EDGE ( 'NONE', *, *, #21946, .F. ) ;
#28133 = CARTESIAN_POINT ( 'NONE',  ( -24.48873108240000107, -14.58042505439999914, 223.9574921880000034 ) ) ;
#28134 = EDGE_LOOP ( 'NONE', ( #13731, #27655, #30549, #10915 ) ) ;
#28135 = CARTESIAN_POINT ( 'NONE',  ( -4.292339292658051697, -2.347882601813513492, -54.09982952342500084 ) ) ;
#28136 = ORIENTED_EDGE ( 'NONE', *, *, #13851, .T. ) ;
#28137 = PRODUCT_CONTEXT ( 'NONE', #18620, 'mechanical' ) ;
#28138 = B_SPLINE_CURVE_WITH_KNOTS ( 'NONE', 5,
 ( #13142, #1202, #3870, #17558, #10796, #18013 ),
 .UNSPECIFIED., .F., .F.,
 ( 6, 6 ),
 ( 0.000000000000000000, 1.000000000000000000 ),
 .UNSPECIFIED. ) ;
#28139 = ORIENTED_EDGE ( 'NONE', *, *, #12770, .F. ) ;
#28140 = FACE_OUTER_BOUND ( 'NONE', #30868, .T. ) ;
#28141 = ORIENTED_EDGE ( 'NONE', *, *, #9395, .F. ) ;
#28142 = CARTESIAN_POINT ( 'NONE',  ( 14.73716614372425049, -28.28456744824856628, -23.36843029042086428 ) ) ;
#28143 = CARTESIAN_POINT ( 'NONE',  ( 24.49999999470000134, -3.000285566199999922E-15, 90.00000000069999828 ) ) ;
#28144 = DIRECTION ( 'NONE',  ( -1.000000000000000000, 0.000000000000000000, 0.000000000000000000 ) ) ;
#28145 = CARTESIAN_POINT ( 'NONE',  ( -21.70990266010000269, 18.50700188859999784, 225.0000000000000000 ) ) ;
#28146 = CARTESIAN_POINT ( 'NONE',  ( 8.000000000285856672, -13.61361098174325868, -34.64062768040190576 ) ) ;
#28147 = ADVANCED_FACE ( 'NONE', ( #12330 ), #17506, .T. ) ;
#28148 = CARTESIAN_POINT ( 'NONE',  ( -17.52531973950389244, 11.86718987797331160, -4.336808689942017736E-16 ) ) ;
#28149 = CARTESIAN_POINT ( 'NONE',  ( -4.646804529178800713, -0.2974863596997128767, -3.648838774900006854 ) ) ;
#28150 = CARTESIAN_POINT ( 'NONE',  ( -13.25572673970000004, -26.61578565920000017, 230.6999999999999886 ) ) ;
#28151 = VERTEX_POINT ( 'NONE', #12167 ) ;
#28152 = CARTESIAN_POINT ( 'NONE',  ( 27.30137319059999967, 6.660265673030000499, 222.0000000000000000 ) ) ;
#28153 = EDGE_CURVE ( 'NONE', #20047, #3589, #22239, .T. ) ;
#28154 = CARTESIAN_POINT ( 'NONE',  ( -3.057389860650357338, 5.459897439232808125, -17.27761783620000102 ) ) ;
#28155 = CARTESIAN_POINT ( 'NONE',  ( 5.647879864692651353, 6.332564579978557262, -40.56776728597595394 ) ) ;
#28156 = ADVANCED_FACE ( 'NONE', ( #24601 ), #3034, .T. ) ;
#28157 = CARTESIAN_POINT ( 'NONE',  ( 26.97469346668950152, -9.357175201752722771, -0.6999999999999784173 ) ) ;
#28158 = CARTESIAN_POINT ( 'NONE',  ( -19.76607646299421361, 19.51851687837242366, 0.7753390690000139251 ) ) ;
#28159 = CARTESIAN_POINT ( 'NONE',  ( -28.49530731802708061, -0.5184832703812680688, 8.000000000000007105 ) ) ;
#28160 = CARTESIAN_POINT ( 'NONE',  ( -17.40937546593514895, -28.45014632087456619, -33.33626032337789269 ) ) ;
#28161 = CARTESIAN_POINT ( 'NONE',  ( 27.35479945376024347, 9.902747534584010580, 1.000000000000000888 ) ) ;
#28162 = CARTESIAN_POINT ( 'NONE',  ( -23.35305511486607344, -13.14889042309849465, 3.928509483819665249 ) ) ;
#28163 = CARTESIAN_POINT ( 'NONE',  ( -0.3000709590666145732, -27.79870762326800104, 4.240370246000018994 ) ) ;
#28164 = B_SPLINE_CURVE_WITH_KNOTS ( 'NONE', 3,
 ( #20843, #30447, #13914, #16423, #1808, #11860, #4160, #2112, #11398, #13753 ),
 .UNSPECIFIED., .F., .F.,
 ( 4, 2, 2, 2, 4 ),
 ( 0.000000000000000000, 0.2500000000000000000, 0.5000000000000000000, 0.7500000000000000000, 1.000000000000000000 ),
 .UNSPECIFIED. ) ;
#28165 = CARTESIAN_POINT ( 'NONE',  ( 27.50000000000000000, -3.367667472999999580E-15, 186.7190980919999959 ) ) ;
#28166 = ORIENTED_EDGE ( 'NONE', *, *, #14593, .F. ) ;
#28167 = LINE ( 'NONE', #13695, #11255 ) ;
#28168 = LINE ( 'NONE', #3620, #10707 ) ;
#28169 = CARTESIAN_POINT ( 'NONE',  ( 9.999999999961115549, -37.77593666300375475, -25.96758248523643786 ) ) ;
#28170 = ORIENTED_EDGE ( 'NONE', *, *, #1741, .F. ) ;
#28171 = CARTESIAN_POINT ( 'NONE',  ( -6.005838698572866008, -2.164963525412170853, -44.41497819512499490 ) ) ;
#28172 = ORIENTED_EDGE ( 'NONE', *, *, #25765, .F. ) ;
#28173 = ORIENTED_EDGE ( 'NONE', *, *, #25272, .F. ) ;
#28174 = ORIENTED_EDGE ( 'NONE', *, *, #7753, .F. ) ;
#28175 = CARTESIAN_POINT ( 'NONE',  ( 3.162069896769252431, -2.100311282821142100, -35.69999999999999574 ) ) ;
#28176 = EDGE_LOOP ( 'NONE', ( #5371, #11681, #19397, #22675 ) ) ;
#28177 = B_SPLINE_CURVE_WITH_KNOTS ( 'NONE', 5,
 ( #22868, #8841, #23026, #18126, #18446, #4132 ),
 .UNSPECIFIED., .F., .F.,
 ( 6, 6 ),
 ( -7.000000000120000010, -4.999999893120000038 ),
 .UNSPECIFIED. ) ;
#28178 = CARTESIAN_POINT ( 'NONE',  ( -27.79999999980000069, 4.328052719890000510, 229.0000000000000000 ) ) ;
#28179 = CARTESIAN_POINT ( 'NONE',  ( -24.36375418918093061, -14.78716628874576244, 3.904032100999987875 ) ) ;
#28180 = CARTESIAN_POINT ( 'NONE',  ( 3.363928025720356985, 1.758349587396049296, -35.70000000000000284 ) ) ;
#28181 = CARTESIAN_POINT ( 'NONE',  ( 17.82645929464983681, -8.108213974639840060, -4.336808689942018722E-16 ) ) ;
#28182 = CARTESIAN_POINT ( 'NONE',  ( 25.32376197130138706, -8.841464498151523799, -1.399999999999998357 ) ) ;
#28183 = CARTESIAN_POINT ( 'NONE',  ( -25.43319852990947183, -8.630493912089182373, 0.000000000000000000 ) ) ;
#28184 = DIRECTION ( 'NONE',  ( -0.8923938138917432150, 1.018860921557045171E-12, 0.4512574441798702374 ) ) ;
#28185 = VERTEX_POINT ( 'NONE', #29466 ) ;
#28186 = CARTESIAN_POINT ( 'NONE',  ( -1.295942751353772238, 4.166547562507297187, -4.774955258300003891 ) ) ;
#28187 = CARTESIAN_POINT ( 'NONE',  ( 0.1047326596782457986, -5.131546142535936994, -23.48138333260000010 ) ) ;
#28188 = CARTESIAN_POINT ( 'NONE',  ( -2.107992564109736122, -27.41908764619381245, 210.0000000000000284 ) ) ;
#28189 = EDGE_CURVE ( 'NONE', #7467, #20783, #27111, .T. ) ;
#28190 = CARTESIAN_POINT ( 'NONE',  ( 23.20948082139999968, -13.40000000000000036, 226.0999999999999943 ) ) ;
#28191 = CARTESIAN_POINT ( 'NONE',  ( -7.505215711015759794, -115.1705934733524543, 21.84354220833749949 ) ) ;
#28192 = DIRECTION ( 'NONE',  ( -0.2665630446479613780, -0.9085064176298685013, -0.3218077568259533061 ) ) ;
#28193 = CARTESIAN_POINT ( 'NONE',  ( -24.64674669160000064, -14.31123007319999907, 226.0986578890000089 ) ) ;
#28194 = VECTOR ( 'NONE', #7402, 1000.000000000000000 ) ;
#28195 = FACE_OUTER_BOUND ( 'NONE', #12107, .T. ) ;
#28196 = CARTESIAN_POINT ( 'NONE',  ( 1.632956991020356519, -28.45346066249067007, 5.208113774000016960 ) ) ;
#28197 = CARTESIAN_POINT ( 'NONE',  ( -10.00000000000468603, -29.62149368164926955, -20.12419128111021749 ) ) ;
#28198 = VERTEX_POINT ( 'NONE', #22398 ) ;
#28199 = CARTESIAN_POINT ( 'NONE',  ( -4.566814987872939824, -1.843056667269423743, -58.63491726642500623 ) ) ;
#28200 = CARTESIAN_POINT ( 'NONE',  ( -21.99953312579999931, 17.62920693399999905, 229.1414213380000149 ) ) ;
#28201 = ORIENTED_EDGE ( 'NONE', *, *, #5449, .F. ) ;
#28202 = VERTEX_POINT ( 'NONE', #29931 ) ;
#28203 = CARTESIAN_POINT ( 'NONE',  ( 0.5890437901233029905, -28.49417040867363227, 3.901346086000012647 ) ) ;
#28204 = FACE_OUTER_BOUND ( 'NONE', #14907, .T. ) ;
#28205 = ORIENTED_EDGE ( 'NONE', *, *, #19659, .T. ) ;
#28206 = DIRECTION ( 'NONE',  ( 0.000000000000000000, 0.000000000000000000, -1.000000000000000000 ) ) ;
#28207 = CARTESIAN_POINT ( 'NONE',  ( 25.43121960300669215, -8.635379644106567554, 186.7828584119999960 ) ) ;
#28208 = ORIENTED_EDGE ( 'NONE', *, *, #8710, .T. ) ;
#28209 = ORIENTED_EDGE ( 'NONE', *, *, #2152, .F. ) ;
#28210 = ORIENTED_EDGE ( 'NONE', *, *, #133, .T. ) ;
#28211 = FILL_AREA_STYLE ('',( #16251 ) ) ;
#28212 = VERTEX_POINT ( 'NONE', #22552 ) ;
#28213 = CARTESIAN_POINT ( 'NONE',  ( -12.29999999972841351, -23.79999999999999716, -28.81887902048947936 ) ) ;
#28214 = CARTESIAN_POINT ( 'NONE',  ( -8.699999999629611125, -16.25267700569241569, -40.75987951459011782 ) ) ;
#28215 = CARTESIAN_POINT ( 'NONE',  ( -5.606848515966891711, 1.848691355091094835, -68.26019511502499881 ) ) ;
#28216 = EDGE_CURVE ( 'NONE', #6144, #22030, #3335, .T. ) ;
#28217 = CARTESIAN_POINT ( 'NONE',  ( 5.229687933670000177, -30.84198039099999633, 228.9999999970000317 ) ) ;
#28218 = AXIS2_PLACEMENT_3D ( 'NONE', #2506, #19648, #14318 ) ;
#28219 = CARTESIAN_POINT ( 'NONE',  ( -8.699999999715885224, -26.99999999997790923, -28.40000000002690683 ) ) ;
#28220 = CARTESIAN_POINT ( 'NONE',  ( 28.39965777970000005, -2.618405453069999833, 222.0000000000000000 ) ) ;
#28221 = CARTESIAN_POINT ( 'NONE',  ( -17.49355845095121609, -24.50295271566449529, -24.06816823009259210 ) ) ;
#28222 = ORIENTED_EDGE ( 'NONE', *, *, #3307, .T. ) ;
#28223 = CARTESIAN_POINT ( 'NONE',  ( -19.20306644830689891, 20.00029701457494369, -0.4291057264425030549 ) ) ;
#28224 = CARTESIAN_POINT ( 'NONE',  ( -3.941349475653395551, -1.876729865818549392, -12.97655742010000246 ) ) ;
#28225 = PLANE ( 'NONE',  #1248 ) ;
#28226 = CARTESIAN_POINT ( 'NONE',  ( -10.69999999968106863, -28.61220480028889668, -31.19591645512378975 ) ) ;
#28227 = ORIENTED_EDGE ( 'NONE', *, *, #9449, .T. ) ;
#28228 = CARTESIAN_POINT ( 'NONE',  ( -11.08346179031915568, -28.41490585489481902, 136.3944487250000179 ) ) ;
#28229 = CYLINDRICAL_SURFACE ( 'NONE', #8245, 6.000000000000001776 ) ;
#28230 = CARTESIAN_POINT ( 'NONE',  ( 18.11692203337192097, 11.57288288306469148, -0.6999999999999784173 ) ) ;
#28231 = FACE_OUTER_BOUND ( 'NONE', #19084, .T. ) ;
#28232 = CARTESIAN_POINT ( 'NONE',  ( -23.81776757772072983, -15.65134804123479917, 4.999998581000003384 ) ) ;
#28233 = CARTESIAN_POINT ( 'NONE',  ( -11.08346179031915568, -28.41490585489481902, 186.3944487249999895 ) ) ;
#28234 = DIRECTION ( 'NONE',  ( 0.8366600265317032381, -0.4922897737126532003, 0.2401057656573751253 ) ) ;
#28235 = CARTESIAN_POINT ( 'NONE',  ( 10.69999999997493134, -121.1571612431100817, -31.29363678846695862 ) ) ;
#28236 = ORIENTED_EDGE ( 'NONE', *, *, #24709, .F. ) ;
#28237 = ADVANCED_FACE ( 'NONE', ( #17804 ), #19339, .F. ) ;
#28238 = DIRECTION ( 'NONE',  ( 0.000000000000000000, 0.000000000000000000, -1.000000000000000000 ) ) ;
#28239 = CARTESIAN_POINT ( 'NONE',  ( 19.80538173169999894, 19.50875421069999760, 224.8000000000000114 ) ) ;
#28240 = CARTESIAN_POINT ( 'NONE',  ( 2.408015917153201180, -3.534003425642091578, -68.10000000002500542 ) ) ;
#28241 = PRODUCT ( 'Release Lever', 'Release Lever', '', ( #639 ) ) ;
#28242 = CARTESIAN_POINT ( 'NONE',  ( 3.686970300939999667, -0.1862064327014488485, -68.94610314789109395 ) ) ;
#28243 = CARTESIAN_POINT ( 'NONE',  ( -2.098672137722010334, -3.287437779826620776, -44.10000000002499121 ) ) ;
#28244 =( LENGTH_UNIT ( ) NAMED_UNIT ( * ) SI_UNIT ( .MILLI., .METRE. ) );
#28245 = B_SPLINE_CURVE_WITH_KNOTS ( 'NONE', 1,
 ( #10053, #16811 ),
 .UNSPECIFIED., .F., .F.,
 ( 2, 2 ),
 ( -2.557301831960000071E-06, 0.7000000000009999335 ),
 .UNSPECIFIED. ) ;
#28246 = VERTEX_POINT ( 'NONE', #20333 ) ;
#28247 = CARTESIAN_POINT ( 'NONE',  ( -4.456723305595252427, 11.49589586079882686, 232.6627637660202765 ) ) ;
#28248 = CARTESIAN_POINT ( 'NONE',  ( 1.082264403401723474, -4.420062499635215580, -65.10397119102499630 ) ) ;
#28249 = ORIENTED_EDGE ( 'NONE', *, *, #22973, .T. ) ;
#28250 = EDGE_CURVE ( 'NONE', #5951, #29211, #3748, .T. ) ;
#28251 = CARTESIAN_POINT ( 'NONE',  ( -17.83930458849792089, 19.99999999999597478, -1.000005633855494125E-09 ) ) ;
#28252 = SHAPE_REPRESENTATION ( 'Pivot Pin', ( #17722 ), #24361 ) ;
#28253 = CARTESIAN_POINT ( 'NONE',  ( 2.127246859547380353, -2.914123423641564070, -88.52261276302716908 ) ) ;
#28254 = ORIENTED_EDGE ( 'NONE', *, *, #6721, .F. ) ;
#28255 = DIRECTION ( 'NONE',  ( -1.000000000000000000, 0.000000000000000000, 0.000000000000000000 ) ) ;
#28256 = VECTOR ( 'NONE', #29305, 1000.000000000000000 ) ;
#28257 = CYLINDRICAL_SURFACE ( 'NONE', #16062, 3.000000000000003997 ) ;
#28258 = CARTESIAN_POINT ( 'NONE',  ( 9.734589334720000764, 19.99999999999999645, -43.07962306035999944 ) ) ;
#28259 = CYLINDRICAL_SURFACE ( 'NONE', #21482, 4.440000000000003055 ) ;
#28260 = B_SPLINE_SURFACE_WITH_KNOTS ( 'NONE', 5, 5, ( 
 ( #17340, #10111, #19709, #15588, #17634, #29292, #27243, #10266, #29755 ),
 ( #27550, #8186, #5683, #17785, #25042, #26944, #19869, #5530, #3473 ),
 ( #29450, #22680, #1125, #5993, #10716, #17489, #5380, #20313, #29915 ),
 ( #8340, #14987, #25194, #3627, #22221, #24584, #3018, #12611, #16066 ),
 ( #1906, #6313, #18255, #23471, #13865, #23308, #3951, #27864, #30224 ),
 ( #15746, #22835, #6776, #25357, #23157, #15908, #8977, #25674, #25516 ) ),
 .UNSPECIFIED., .F., .F., .F.,
 ( 6, 6 ),
 ( 6, 3, 6 ),
 ( 0.000000000000000000, 23.80447727570000183 ),
 ( 8.011061266649999624, 9.372204729519999944, 10.73334819239999938 ),
 .UNSPECIFIED. ) ;
#28261 = CARTESIAN_POINT ( 'NONE',  ( -17.20468998641224800, -22.47541256591814474, -31.56123091905952549 ) ) ;
#28262 = CARTESIAN_POINT ( 'NONE',  ( -12.40011512277526862, -21.99999999999999289, -29.68241223786358773 ) ) ;
#28263 = CARTESIAN_POINT ( 'NONE',  ( -8.699999999662093586, -15.94902145834643115, -35.53273252493492862 ) ) ;
#28264 = ORIENTED_EDGE ( 'NONE', *, *, #16214, .T. ) ;
#28265 = CARTESIAN_POINT ( 'NONE',  ( -26.93395386830000149, 3.298349104069999855E-15, 192.2432411359999946 ) ) ;
#28266 = ADVANCED_FACE ( 'NONE', ( #25692 ), #18594, .T. ) ;
#28267 = CARTESIAN_POINT ( 'NONE',  ( 1.099927927706055852, -26.77741881808358215, 225.1458785545408716 ) ) ;
#28268 = DIRECTION ( 'NONE',  ( 0.000000000000000000, 1.000000000000000000, 0.000000000000000000 ) ) ;
#28269 = EDGE_CURVE ( 'NONE', #18020, #23553, #20322, .T. ) ;
#28270 = CARTESIAN_POINT ( 'NONE',  ( -2.582101660013529365, 2.527668734551885787, 230.7711489403428970 ) ) ;
#28271 = LINE ( 'NONE', #26080, #22203 ) ;
#28272 = CARTESIAN_POINT ( 'NONE',  ( 10.21223621230000056, 6.545646588569999480, 230.6412452697800006 ) ) ;
#28273 = CARTESIAN_POINT ( 'NONE',  ( 23.67037533738476540, 14.57986020592288234, 3.928017074518106888 ) ) ;
#28274 = DIRECTION ( 'NONE',  ( 0.000000000000000000, 1.000000000000000000, 0.000000000000000000 ) ) ;
#28275 = CARTESIAN_POINT ( 'NONE',  ( 3.357378826392681592, -2.722208303785305539, -55.00923804942500084 ) ) ;
#28276 = EDGE_CURVE ( 'NONE', #5864, #19664, #30716, .T. ) ;
#28277 = DIRECTION ( 'NONE',  ( -0.9880370573969197157, 0.1542166437529879364, 0.000000000000000000 ) ) ;
#28278 = CARTESIAN_POINT ( 'NONE',  ( -20.30396346383280104, 20.00000000000023803, 229.1317800523452775 ) ) ;
#28279 = CARTESIAN_POINT ( 'NONE',  ( 2.551353244962082822, -2.580622056418603094, 230.7617868067710276 ) ) ;
#28280 = CIRCLE ( 'NONE', #14721, 27.50000000000000000 ) ;
#28281 = CARTESIAN_POINT ( 'NONE',  ( -13.99999999969999820, 20.99999999999999645, -58.51619611000000276 ) ) ;
#28282 = CARTESIAN_POINT ( 'NONE',  ( -23.83777999500000178, -14.30502388280000048, 223.9971937000000253 ) ) ;
#28283 = ADVANCED_FACE ( 'NONE', ( #11672 ), #28035, .T. ) ;
#28284 = ORIENTED_EDGE ( 'NONE', *, *, #25859, .T. ) ;
#28285 = CARTESIAN_POINT ( 'NONE',  ( 2.259239758627727745, -4.069767828330737913, -56.33172062782499978 ) ) ;
#28286 = ORIENTED_EDGE ( 'NONE', *, *, #12985, .T. ) ;
#28287 = CONTEXT_DEPENDENT_SHAPE_REPRESENTATION ( #23880, #3376 ) ;
#28288 = ORIENTED_EDGE ( 'NONE', *, *, #24440, .T. ) ;
#28289 = CARTESIAN_POINT ( 'NONE',  ( -10.99999999969999998, 20.99999999999999645, -58.51619611000000276 ) ) ;
#28290 = ORIENTED_EDGE ( 'NONE', *, *, #5748, .T. ) ;
#28291 = DIRECTION ( 'NONE',  ( 0.000000000000000000, 0.000000000000000000, 1.000000000000000000 ) ) ;
#28292 = EDGE_CURVE ( 'NONE', #8812, #27653, #16305, .T. ) ;
#28293 = VECTOR ( 'NONE', #24910, 1000.000000000000114 ) ;
#28294 = LINE ( 'NONE', #8784, #21006 ) ;
#28295 = LINE ( 'NONE', #23275, #18958 ) ;
#28296 = CARTESIAN_POINT ( 'NONE',  ( 0.000000000000000000, 0.000000000000000000, 40.00000000000000000 ) ) ;
#28297 = CARTESIAN_POINT ( 'NONE',  ( 27.98121187870611593, -9.706323496128696604, 8.000000000000007105 ) ) ;
#28298 = DIRECTION ( 'NONE',  ( 1.000000000000000000, 0.000000000000000000, 0.000000000000000000 ) ) ;
#28299 = CARTESIAN_POINT ( 'NONE',  ( 2.521631941452528558, 3.946033397249446573, -4.700967428500005596 ) ) ;
#28300 = AXIS2_PLACEMENT_3D ( 'NONE', #27077, #5515, #15118 ) ;
#28301 = CARTESIAN_POINT ( 'NONE',  ( 5.185037338370000803, -30.57858919520000285, 230.5592437530000041 ) ) ;
#28302 = ORIENTED_EDGE ( 'NONE', *, *, #9715, .F. ) ;
#28303 = CARTESIAN_POINT ( 'NONE',  ( 25.46368747440213198, -12.80129684534102807, 4.999998581000003384 ) ) ;
#28304 = CARTESIAN_POINT ( 'NONE',  ( 5.782996427689181651, 1.709881257618839356, -18.14190840230000390 ) ) ;
#28305 = CARTESIAN_POINT ( 'NONE',  ( 4.051823674760409943, -0.6775361292690254000, -35.74517599850000948 ) ) ;
#28306 = EDGE_CURVE ( 'NONE', #16100, #11991, #13990, .T. ) ;
#28307 = CARTESIAN_POINT ( 'NONE',  ( 28.03861306157277866, 0.5101735396241827702, -0.2432540810000105580 ) ) ;
#28308 = CARTESIAN_POINT ( 'NONE',  ( 0.4702670923129999569, -27.79645255899999867, 223.9974824469999817 ) ) ;
#28309 = CARTESIAN_POINT ( 'NONE',  ( -25.43411672857565264, -11.59571042436485655, 8.000000000000007105 ) ) ;
#28310 = CARTESIAN_POINT ( 'NONE',  ( -2.660719428328687020, 2.391127420732980013, 227.6907824390136170 ) ) ;
#28311 = CARTESIAN_POINT ( 'NONE',  ( -1.861312627829580402, -20.50181238076562096, -27.47976714835994727 ) ) ;
#28312 = CARTESIAN_POINT ( 'NONE',  ( 8.700000000289357160, -13.80041476817676127, -36.85204346332353254 ) ) ;
#28313 = LINE ( 'NONE', #16051, #25358 ) ;
#28314 = VECTOR ( 'NONE', #5023, 1000.000000000000000 ) ;
#28315 = AXIS2_PLACEMENT_3D ( 'NONE', #9468, #7111, #16695 ) ;
#28316 = LINE ( 'NONE', #23296, #6216 ) ;
#28317 = VERTEX_POINT ( 'NONE', #30413 ) ;
#28318 = VECTOR ( 'NONE', #14286, 1000.000000000000000 ) ;
#28319 = CARTESIAN_POINT ( 'NONE',  ( 4.132574650175937059, -31.83942647549183746, -80.46693306215520636 ) ) ;
#28320 = CARTESIAN_POINT ( 'NONE',  ( -24.68204616399999907, -14.25020164319999871, 223.9000014189999774 ) ) ;
#28321 = EDGE_CURVE ( 'NONE', #15258, #29368, #23363, .T. ) ;
#28322 = CARTESIAN_POINT ( 'NONE',  ( -1.354272418126746702, -5.070319514866119981, -0.7001538049033677602 ) ) ;
#28323 = ORIENTED_EDGE ( 'NONE', *, *, #12082, .T. ) ;
#28324 = CARTESIAN_POINT ( 'NONE',  ( -3.948109860491266776, 2.321589337205137937, -45.24354844312500745 ) ) ;
#28325 = ORIENTED_EDGE ( 'NONE', *, *, #20743, .T. ) ;
#28326 = ORIENTED_EDGE ( 'NONE', *, *, #4372, .T. ) ;
#28327 = ADVANCED_FACE ( 'NONE', ( #1927 ), #5014, .F. ) ;
#28328 = ORIENTED_EDGE ( 'NONE', *, *, #15423, .F. ) ;
#28329 = DIRECTION ( 'NONE',  ( 5.962915006522623408E-16, 0.4383711467890810676, 0.8987940462991651502 ) ) ;
#28330 = VERTEX_POINT ( 'NONE', #26303 ) ;
#28331 = CARTESIAN_POINT ( 'NONE',  ( -25.11765555659999904, -13.46780168200000105, 225.6808342349999918 ) ) ;
#28332 = FACE_OUTER_BOUND ( 'NONE', #25710, .T. ) ;
#28333 = CARTESIAN_POINT ( 'NONE',  ( -23.81776757772072983, -15.65134804123479917, 4.895813258999987205 ) ) ;
#28334 = CARTESIAN_POINT ( 'NONE',  ( 10.35667741062603397, -26.55163333981976592, 40.00000000000000000 ) ) ;
#28335 = CARTESIAN_POINT ( 'NONE',  ( 17.87667150816518102, 20.00000000000230926, -0.6999999999999783062 ) ) ;
#28336 = DIRECTION ( 'NONE',  ( 0.000000000000000000, -1.000000000000000000, 0.000000000000000000 ) ) ;
#28337 = CARTESIAN_POINT ( 'NONE',  ( 3.480076166481417488, -0.9723312654487008544, 227.7113415996591925 ) ) ;
#28338 = CIRCLE ( 'NONE', #17281, 3.000000000000001332 ) ;
#28339 = CARTESIAN_POINT ( 'NONE',  ( -19.80526744909999692, 19.50877353739999975, 229.0000000010000178 ) ) ;
#28340 = VECTOR ( 'NONE', #15050, 1000.000000000000000 ) ;
#28341 = ORIENTED_EDGE ( 'NONE', *, *, #30113, .T. ) ;
#28342 = VECTOR ( 'NONE', #2444, 1000.000000000000000 ) ;
#28343 = CARTESIAN_POINT ( 'NONE',  ( 4.347198243976411192, 0.5700341643805815206, -6.126979598399997506 ) ) ;
#28344 = CARTESIAN_POINT ( 'NONE',  ( -5.367600138795724618, 3.713494282866228069, -24.86779765530000574 ) ) ;
#28345 = AXIS2_PLACEMENT_3D ( 'NONE', #24632, #5583, #14889 ) ;
#28346 = CARTESIAN_POINT ( 'NONE',  ( -8.090238276950914909, -26.28358643434116004, 207.3140698626388314 ) ) ;
#28347 = CIRCLE ( 'NONE', #8222, 3.200000004570001888 ) ;
#28348 = FACE_BOUND ( 'NONE', #27468, .T. ) ;
#28349 = CARTESIAN_POINT ( 'NONE',  ( -7.000000000054375171, -115.1185614904109542, 21.95989595794997129 ) ) ;
#28350 = CARTESIAN_POINT ( 'NONE',  ( -2.255103148512942468, -21.81692582113129575, -30.17614928725820533 ) ) ;
#28351 = CARTESIAN_POINT ( 'NONE',  ( -24.11911872370000154, -15.18353100999999938, 225.3106464589999973 ) ) ;
#28352 = LINE ( 'NONE', #30878, #1147 ) ;
#28353 = FACE_BOUND ( 'NONE', #22244, .T. ) ;
#28354 = LINE ( 'NONE', #9000, #22348 ) ;
#28355 = ORIENTED_EDGE ( 'NONE', *, *, #1132, .T. ) ;
#28356 = CARTESIAN_POINT ( 'NONE',  ( -5.545418199629476241, -2.237997381628727300, -58.90491726642499515 ) ) ;
#28357 = MECHANICAL_DESIGN_GEOMETRIC_PRESENTATION_REPRESENTATION (  '', ( #15305 ), #19331 ) ;
#28358 = CARTESIAN_POINT ( 'NONE',  ( -24.76252940850000073, 13.73644554549999874, 229.4485733019999998 ) ) ;
#28359 = CARTESIAN_POINT ( 'NONE',  ( 11.20000000009999930, -32.00000000000000000, -25.51324865394999719 ) ) ;
#28360 = CARTESIAN_POINT ( 'NONE',  ( -0.6320852424383932577, 6.069672320066970883, -25.88903409330001182 ) ) ;
#28361 = ORIENTED_EDGE ( 'NONE', *, *, #27923, .F. ) ;
#28362 = DIRECTION ( 'NONE',  ( 0.000000000000000000, 0.000000000000000000, -1.000000000000000000 ) ) ;
#28363 = CARTESIAN_POINT ( 'NONE',  ( 19.80538173680000114, 19.50875419940000199, 226.9999998930000231 ) ) ;
#28364 = EDGE_CURVE ( 'NONE', #10669, #565, #25291, .T. ) ;
#28365 = CIRCLE ( 'NONE', #237, 4.000000000000000888 ) ;
#28366 = ORIENTED_EDGE ( 'NONE', *, *, #23117, .T. ) ;
#28367 = VECTOR ( 'NONE', #8683, 1000.000000000000114 ) ;
#28368 = ORIENTED_EDGE ( 'NONE', *, *, #3291, .T. ) ;
#28369 = EDGE_LOOP ( 'NONE', ( #28417, #29244, #19899, #21438 ) ) ;
#28370 = TOROIDAL_SURFACE ( 'NONE', #6263, 30.50000000000000000, 3.000000000000000000 ) ;
#28371 = SURFACE_STYLE_USAGE ( .BOTH. , #4460 ) ;
#28372 = VECTOR ( 'NONE', #29269, 1000.000000000000000 ) ;
#28373 = ORIENTED_EDGE ( 'NONE', *, *, #14412, .T. ) ;
#28375 = CARTESIAN_POINT ( 'NONE',  ( 10.00000000020000002, 19.99999999999999645, -2.400000000399998612 ) ) ;
#28374 = B_SPLINE_CURVE_WITH_KNOTS ( 'NONE', 5,
 ( #25467, #9082, #3901, #20736, #18677, #8766, #18375, #27970, #16780, #28439, #16936, #19307 ),
 .UNSPECIFIED., .F., .F.,
 ( 6, 3, 3, 6 ),
 ( 3.339306056889999930, 4.810258468999999870, 6.613963840320000287, 6.678484285959999767 ),
 .UNSPECIFIED. ) ;
#28376 = ADVANCED_FACE ( 'NONE', ( #12129 ), #7764, .T. ) ;
#28377 = ADVANCED_FACE ( 'NONE', ( #24411 ), #19536, .T. ) ;
#28378 = CARTESIAN_POINT ( 'NONE',  ( -8.699999999654229654, -13.99314194387733323, -37.12415143712361498 ) ) ;
#28379 = CARTESIAN_POINT ( 'NONE',  ( -3.857468353316018117, 3.836780423039637178, -68.14322600472499403 ) ) ;
#28380 = CARTESIAN_POINT ( 'NONE',  ( 20.00949237780000090, -20.13757562109999810, 230.0000000000000000 ) ) ;
#28381 = DIRECTION ( 'NONE',  ( 1.000000000000000000, -9.224647189900200933E-13, 4.710284450064084831E-12 ) ) ;
#28382 = DIRECTION ( 'NONE',  ( 0.000000000000000000, 0.000000000000000000, -1.000000000000000000 ) ) ;
#28383 = CIRCLE ( 'NONE', #27882, 27.50000000000000000 ) ;
#28384 = PRESENTATION_LAYER_ASSIGNMENT (  '', '', ( #29380 ) ) ;
#28385 = CARTESIAN_POINT ( 'NONE',  ( 0.4821455018050000429, -28.49635764770000179, 226.0025203910000187 ) ) ;
#28386 = VERTEX_POINT ( 'NONE', #23957 ) ;
#28387 = CARTESIAN_POINT ( 'NONE',  ( -18.77172700302876507, 19.99998314052377069, -0.5795685437816225916 ) ) ;
#28388 = CARTESIAN_POINT ( 'NONE',  ( 6.482330152203070739, 0.4632910120546396282, -14.04454535870000598 ) ) ;
#28389 = CARTESIAN_POINT ( 'NONE',  ( 26.80000000000000071, 7.105427357599999217E-15, 0.000000000000000000 ) ) ;
#28390 = AXIS2_PLACEMENT_3D ( 'NONE', #11454, #30337, #11607 ) ;
#28391 = CARTESIAN_POINT ( 'NONE',  ( 11.28020549271892570, -4.977446785437388499, 232.6627636541932702 ) ) ;
#28392 = ORIENTED_EDGE ( 'NONE', *, *, #15174, .T. ) ;
#28393 = CYLINDRICAL_SURFACE ( 'NONE', #129, 3.749999999999999556 ) ;
#28394 = CARTESIAN_POINT ( 'NONE',  ( 1.495522319887057749, -27.76012052182125345, 4.493506933999996455 ) ) ;
#28395 = VECTOR ( 'NONE', #929, 1000.000000000000000 ) ;
#28396 = CARTESIAN_POINT ( 'NONE',  ( -27.79999999169999825, 0.8519339693649999878, 222.0000000000000000 ) ) ;
#28397 = DIRECTION ( 'NONE',  ( 0.000000000000000000, 0.3420201433259318358, -0.9396926207858125046 ) ) ;
#28398 = CARTESIAN_POINT ( 'NONE',  ( 22.86188831120908560, -13.98516151523984341, 4.123351189131411410 ) ) ;
#28399 = CARTESIAN_POINT ( 'NONE',  ( 3.542472921321142110, 4.818407451951889797, -66.64226422552501106 ) ) ;
#28400 = CARTESIAN_POINT ( 'NONE',  ( 10.69999999997629914, -123.6108562392817731, -31.89970902356391136 ) ) ;
#28401 = ORIENTED_EDGE ( 'NONE', *, *, #26245, .T. ) ;
#28402 = CARTESIAN_POINT ( 'NONE',  ( -2.947640775130000104E-14, -27.50000000000000000, 223.8999999999999773 ) ) ;
#28403 = CYLINDRICAL_SURFACE ( 'NONE', #20156, 0.9999999999999988898 ) ;
#28404 = EDGE_CURVE ( 'NONE', #24784, #6473, #6452, .T. ) ;
#28405 =( GEOMETRIC_REPRESENTATION_CONTEXT ( 3 ) GLOBAL_UNCERTAINTY_ASSIGNED_CONTEXT ( ( #24818 ) ) GLOBAL_UNIT_ASSIGNED_CONTEXT ( ( #13550, #14027, #9130 ) ) REPRESENTATION_CONTEXT ( 'NONE', 'WORKASPACE' ) );
#28406 = CARTESIAN_POINT ( 'NONE',  ( 2.495111619170718775, -4.070681774061544189, -68.10000000002501963 ) ) ;
#28407 = CIRCLE ( 'NONE', #8781, 4.987531172950001590 ) ;
#28408 = CARTESIAN_POINT ( 'NONE',  ( 10.69999999997255991, -24.59987423426687059, -30.24240556170614269 ) ) ;
#28409 = DIRECTION ( 'NONE',  ( -1.224606353819999829E-16, -1.000000000000000000, 0.000000000000000000 ) ) ;
#28410 = SURFACE_STYLE_USAGE ( .BOTH. , #30770 ) ;
#28411 = ORIENTED_EDGE ( 'NONE', *, *, #23886, .T. ) ;
#28412 = CARTESIAN_POINT ( 'NONE',  ( -9.999999999959999997, -24.87868334570000073, -26.27868334529999927 ) ) ;
#28413 = CARTESIAN_POINT ( 'NONE',  ( 3.542472921321142110, 4.818407451951889797, -67.12226422552500082 ) ) ;
#28414 = ORIENTED_EDGE ( 'NONE', *, *, #21395, .T. ) ;
#28415 = CARTESIAN_POINT ( 'NONE',  ( -2.070461221339999991, -7.056594471000000368, 228.3912452697800006 ) ) ;
#28416 = CARTESIAN_POINT ( 'NONE',  ( -19.80526744929999694, 19.50877353739999975, 229.0739196179999908 ) ) ;
#28417 = ORIENTED_EDGE ( 'NONE', *, *, #12082, .F. ) ;
#28418 = CARTESIAN_POINT ( 'NONE',  ( -5.729936103060000008, 1.681209052119999825, 226.6412452697800006 ) ) ;
#28419 = LINE ( 'NONE', #6700, #22044 ) ;
#28420 = CARTESIAN_POINT ( 'NONE',  ( -0.3000709590666145732, -27.79870762326800104, 4.240370246000018994 ) ) ;
#28421 = DIRECTION ( 'NONE',  ( 0.000000000000000000, 0.000000000000000000, 1.000000000000000000 ) ) ;
#28422 = ORIENTED_EDGE ( 'NONE', *, *, #2934, .T. ) ;
#28423 = CARTESIAN_POINT ( 'NONE',  ( -23.55444264242456498, 16.04540112444970390, 8.000000000000007105 ) ) ;
#28424 = EDGE_LOOP ( 'NONE', ( #2941, #22071, #12423, #26772 ) ) ;
#28425 = CARTESIAN_POINT ( 'NONE',  ( -1.776062861149290062E-14, -3.231615895114969171E-16, -0.5999999999999894307 ) ) ;
#28426 = EDGE_CURVE ( 'NONE', #27863, #368, #188, .T. ) ;
#28427 = CARTESIAN_POINT ( 'NONE',  ( 24.62873585949999722, -14.34148440729999940, 226.0959678990000157 ) ) ;
#28428 = LINE ( 'NONE', #4359, #19321 ) ;
#28429 = ADVANCED_FACE ( 'NONE', ( #7710 ), #24369, .T. ) ;
#28430 = CARTESIAN_POINT ( 'NONE',  ( -25.27355175290000133, 12.75978488059999805, 229.0000000000000000 ) ) ;
#28431 = CARTESIAN_POINT ( 'NONE',  ( 17.18658402241074867, -10.09981795543446736, -0.6999999999999784173 ) ) ;
#28432 = CARTESIAN_POINT ( 'NONE',  ( 11.34419785409999903, -4.447397018089999321, 230.6412452697800006 ) ) ;
#28433 = B_SPLINE_CURVE_WITH_KNOTS ( 'NONE', 5,
 ( #22206, #25179, #20454, #6132, #1270, #27079, #10870, #30051, #15725, #5517, #15120, #24718, #12754, #22366, #10401 ),
 .UNSPECIFIED., .F., .F.,
 ( 6, 3, 3, 3, 6 ),
 ( 0.000000000000000000, 0.09999999999828219910, 0.3999999999988547716, 0.6999999999999999556, 1.000000000000000000 ),
 .UNSPECIFIED. ) ;
#28434 = CARTESIAN_POINT ( 'NONE',  ( -24.37450209798932477, 13.36961646417070249, 3.904029301000005781 ) ) ;
#28435 = CARTESIAN_POINT ( 'NONE',  ( 1.229093439949830335, 1.599333684796359956, 227.6412452700770928 ) ) ;
#28436 = CARTESIAN_POINT ( 'NONE',  ( -4.213298386699523945, 4.800796338101376293, -53.50587006832499526 ) ) ;
#28437 = EDGE_CURVE ( 'NONE', #13159, #20501, #3450, .T. ) ;
#28438 = CARTESIAN_POINT ( 'NONE',  ( 9.631068058028711576, 20.99999999999431211, -53.61809490185450500 ) ) ;
#28439 = CARTESIAN_POINT ( 'NONE',  ( 7.638652831670083465, 3.781993549609147465, -39.32377067501277423 ) ) ;
#28440 = CARTESIAN_POINT ( 'NONE',  ( 2.205637557623687073, -3.179374645688476164, 230.6249086619264688 ) ) ;
#28441 = ORIENTED_EDGE ( 'NONE', *, *, #3459, .T. ) ;
#28442 = LINE ( 'NONE', #25469, #5199 ) ;
#28443 = CARTESIAN_POINT ( 'NONE',  ( -24.04140365350000152, -13.95971772459999904, 223.9013449489999914 ) ) ;
#28444 = EDGE_CURVE ( 'NONE', #30538, #14782, #14811, .T. ) ;
#28445 = CARTESIAN_POINT ( 'NONE',  ( -1.034595936873321076, -4.789217790999566127, -56.68033560642500390 ) ) ;
#28446 = ORIENTED_EDGE ( 'NONE', *, *, #29847, .F. ) ;
#28447 = ORIENTED_EDGE ( 'NONE', *, *, #13209, .T. ) ;
#28448 = CARTESIAN_POINT ( 'NONE',  ( -17.48633009204728239, -29.79399746876627120, -32.56041429237782125 ) ) ;
#28449 = ORIENTED_EDGE ( 'NONE', *, *, #26909, .T. ) ;
#28450 = CARTESIAN_POINT ( 'NONE',  ( 14.81448010921228509, -28.73192765248866110, -23.62653622451373892 ) ) ;
#28451 = DIRECTION ( 'NONE',  ( 0.000000000000000000, 0.000000000000000000, 1.000000000000000000 ) ) ;
#28452 = CARTESIAN_POINT ( 'NONE',  ( -27.79539923781684863, -0.5057481689249068157, 5.200000000000009948 ) ) ;
#28453 = B_SPLINE_CURVE_WITH_KNOTS ( 'NONE', 3,
 ( #2459, #14725, #12505, #26218, #12052, #26675 ),
 .UNSPECIFIED., .F., .F.,
 ( 4, 2, 4 ),
 ( 0.000000000000000000, 0.5000000000000000000, 1.000000000000000000 ),
 .UNSPECIFIED. ) ;
#28454 = LINE ( 'NONE', #6586, #4784 ) ;
#28455 = CARTESIAN_POINT ( 'NONE',  ( 7.105427357599999217E-15, 3.552713678799999608E-15, 193.6055512750000105 ) ) ;
#28456 = APPLICATION_CONTEXT ( 'automotive_design' ) ;
#28457 = CARTESIAN_POINT ( 'NONE',  ( -2.486939662212004354, -18.42307621383944749, -106.6672263875570650 ) ) ;
#28458 = CARTESIAN_POINT ( 'NONE',  ( 0.1708583496781435063, 4.358252033550405358, -7.937690181100000686 ) ) ;
#28459 = CARTESIAN_POINT ( 'NONE',  ( -14.07565872370000015, -28.26210308950000183, 229.4982322489999831 ) ) ;
#28460 = EDGE_LOOP ( 'NONE', ( #31006, #27052, #5560, #3369 ) ) ;
#28461 = CARTESIAN_POINT ( 'NONE',  ( -24.64674669169999888, -14.31123007319999907, 223.9013449489999914 ) ) ;
#28462 = CARTESIAN_POINT ( 'NONE',  ( 5.320018516182488000, -2.211191048809329374, -18.47122516809999837 ) ) ;
#28463 = CARTESIAN_POINT ( 'NONE',  ( 26.07698513492398718, 11.88166128046557546, 8.000000000000007105 ) ) ;
#28464 = CARTESIAN_POINT ( 'NONE',  ( -10.14136574519999989, -25.00000000000000000, -1.689351118899999671 ) ) ;
#28465 = CARTESIAN_POINT ( 'NONE',  ( 28.68577476828162531, -9.950727360111285336, 1.000000000000000888 ) ) ;
#28466 = CARTESIAN_POINT ( 'NONE',  ( 1.089891362619999970, -28.47934442809999922, 224.6898179359999972 ) ) ;
#28467 = CARTESIAN_POINT ( 'NONE',  ( 0.000000000000000000, 0.000000000000000000, 140.0000000000000000 ) ) ;
#28468 = CARTESIAN_POINT ( 'NONE',  ( -5.534792526179823646, -1.995162464570431782, -43.61497819512499774 ) ) ;
#28469 = ADVANCED_FACE ( 'NONE', ( #25173 ), #687, .F. ) ;
#28470 = FACE_OUTER_BOUND ( 'NONE', #22107, .T. ) ;
#28471 = CARTESIAN_POINT ( 'NONE',  ( 2.434303047052905011, -2.556415643317960562, 226.6412452697750552 ) ) ;
#28472 = CARTESIAN_POINT ( 'NONE',  ( 8.700000000234771491, -29.98808444042839838, -27.92350772035144857 ) ) ;
#28473 = CARTESIAN_POINT ( 'NONE',  ( 0.000000000000000000, 0.000000000000000000, 140.0000000000000000 ) ) ;
#28474 = EDGE_LOOP ( 'NONE', ( #23468, #1895, #16864, #25703, #23154, #20549 ) ) ;
#28475 = CARTESIAN_POINT ( 'NONE',  ( -10.02699808790000091, 19.99999999999999645, -2.016765154599996279 ) ) ;
#28476 = CYLINDRICAL_SURFACE ( 'NONE', #11456, 3.000000000000002220 ) ;
#28477 = CARTESIAN_POINT ( 'NONE',  ( 14.40197535836999876, -26.99999999999984368, -34.17350269180000311 ) ) ;
#28478 = VERTEX_POINT ( 'NONE', #3300 ) ;
#28479 = ADVANCED_FACE ( 'NONE', ( #3604 ), #13200, .T. ) ;
#28480 = CARTESIAN_POINT ( 'NONE',  ( -3.130203125555106158, 5.106303518385050033, -45.05531229042499319 ) ) ;
#28481 = VERTEX_POINT ( 'NONE', #8163 ) ;
#28482 = ORIENTED_EDGE ( 'NONE', *, *, #28269, .T. ) ;
#28483 = EDGE_CURVE ( 'NONE', #55, #15092, #16205, .T. ) ;
#28484 = DIRECTION ( 'NONE',  ( 0.000000000000000000, 0.000000000000000000, 1.000000000000000000 ) ) ;
#28485 = ORIENTED_EDGE ( 'NONE', *, *, #11756, .T. ) ;
#28486 = CARTESIAN_POINT ( 'NONE',  ( 0.000000000000000000, 26.42151601322854759, -59.26168417594741555 ) ) ;
#28487 = ADVANCED_FACE ( 'NONE', ( #8478 ), #22513, .T. ) ;
#28488 = VERTEX_POINT ( 'NONE', #29735 ) ;
#28489 = CARTESIAN_POINT ( 'NONE',  ( 17.29283780772782819, 12.10247952218883682, -0.6999999999999784173 ) ) ;
#28490 = CARTESIAN_POINT ( 'NONE',  ( 23.39354070784786543, 15.01969649483752001, 4.239862992999999136 ) ) ;
#28491 = CARTESIAN_POINT ( 'NONE',  ( -1.243449787579999883E-14, 0.000000000000000000, -0.6999999999999992895 ) ) ;
#28492 = CARTESIAN_POINT ( 'NONE',  ( 0.7056244670274119946, 4.148270963307473913, -35.69999999999998153 ) ) ;
#28493 = EDGE_CURVE ( 'NONE', #5911, #26442, #22812, .T. ) ;
#28494 = CARTESIAN_POINT ( 'NONE',  ( 19.40803489293128692, 20.00003047048157256, -0.3219712011826995068 ) ) ;
#28495 = FACE_OUTER_BOUND ( 'NONE', #5559, .T. ) ;
#28496 = DIRECTION ( 'NONE',  ( 1.000000000000000000, 0.000000000000000000, 0.000000000000000000 ) ) ;
#28497 = CARTESIAN_POINT ( 'NONE',  ( -18.03086237940000203, 20.00000062619999852, 230.7000111870000012 ) ) ;
#28498 = CARTESIAN_POINT ( 'NONE',  ( -1.102325287918849650, -5.983340188646091740, -4.125234013000008915 ) ) ;
#28499 = CARTESIAN_POINT ( 'NONE',  ( 0.6138679561251692007, 4.311712124478116692, -28.50600711720001001 ) ) ;
#28500 = PLANE ( 'NONE',  #12284 ) ;
#28501 = EDGE_CURVE ( 'NONE', #3582, #9397, #26863, .T. ) ;
#28502 = CARTESIAN_POINT ( 'NONE',  ( -23.28210887531993123, -13.27420452059575062, 223.8999999999999773 ) ) ;
#28503 = CARTESIAN_POINT ( 'NONE',  ( 0.3123980048345580962, 3.499890163171272661, 227.6523062920452958 ) ) ;
#28504 = DIRECTION ( 'NONE',  ( 0.000000000000000000, 0.000000000000000000, 1.000000000000000000 ) ) ;
#28505 = CARTESIAN_POINT ( 'NONE',  ( -3.630162863991669209, -2.403661707492378508, -6.889929326000000742 ) ) ;
#28506 = PRESENTATION_LAYER_ASSIGNMENT (  '', '', ( #29487 ) ) ;
#28507 = CIRCLE ( 'NONE', #18961, 2.999999999999999112 ) ;
#28508 = CARTESIAN_POINT ( 'NONE',  ( 27.79999999999999716, 2.355323124549999985E-11, 229.1414213560000235 ) ) ;
#28509 = FACE_OUTER_BOUND ( 'NONE', #15587, .T. ) ;
#28510 = CARTESIAN_POINT ( 'NONE',  ( -24.50943110104372380, -10.89728548205058623, -1.399999999999998579 ) ) ;
#28511 = ORIENTED_EDGE ( 'NONE', *, *, #6621, .F. ) ;
#28512 = B_SPLINE_CURVE_WITH_KNOTS ( 'NONE', 1,
 ( #6718, #16322 ),
 .UNSPECIFIED., .F., .F.,
 ( 2, 2 ),
 ( -3.500000000000000000, 3.500000000000000000 ),
 .UNSPECIFIED. ) ;
#28513 = CARTESIAN_POINT ( 'NONE',  ( -17.83931601680000156, 20.00000000000000000, 230.0000000000000000 ) ) ;
#28514 = ADVANCED_FACE ( 'NONE', ( #25018 ), #27678, .F. ) ;
#28515 = CARTESIAN_POINT ( 'NONE',  ( 18.24300304067004674, 10.73161574555001607, -4.336808689942017243E-16 ) ) ;
#28516 = CARTESIAN_POINT ( 'NONE',  ( 3.499930668447871707, 4.992711500626898058, -29.21106724380000230 ) ) ;
#28517 = EDGE_LOOP ( 'NONE', ( #1789, #824, #597, #19476 ) ) ;
#28518 = CARTESIAN_POINT ( 'NONE',  ( -2.486939662212006130, -15.93335509046202247, -109.1271631200378494 ) ) ;
#28519 = DIRECTION ( 'NONE',  ( 1.000000000000000000, -1.843431230200657634E-12, 2.650498504950726461E-12 ) ) ;
#28520 = ORIENTED_EDGE ( 'NONE', *, *, #5979, .F. ) ;
#28521 = ORIENTED_EDGE ( 'NONE', *, *, #24628, .T. ) ;
#28522 = ORIENTED_EDGE ( 'NONE', *, *, #8074, .T. ) ;
#28523 = PRODUCT_CONTEXT ( 'NONE', #26848, 'mechanical' ) ;
#28524 = EDGE_LOOP ( 'NONE', ( #6226, #916, #16060, #19138 ) ) ;
#28525 = CARTESIAN_POINT ( 'NONE',  ( -17.49999999969999820, -24.59808825516011410, -30.23948587685871559 ) ) ;
#28526 = AXIS2_PLACEMENT_3D ( 'NONE', #1874, #2188, #11473 ) ;
#28527 = DIRECTION ( 'NONE',  ( 0.6941258031311203780, 0.7198537139083029945, 0.000000000000000000 ) ) ;
#28528 = CARTESIAN_POINT ( 'NONE',  ( 5.352151167820474953, -2.399090168605950701, -66.47841551492498979 ) ) ;
#28529 = LINE ( 'NONE', #16258, #1354 ) ;
#28530 = TOROIDAL_SURFACE ( 'NONE', #24997, 30.50000000000000000, 3.000000000000000000 ) ;
#28531 = B_SPLINE_CURVE_WITH_KNOTS ( 'NONE', 3,
 ( #30556, #21111, #23635, #25522, #28182, #25684, #23317, #6624, #21262, #1765, #18738, #11046, #18898, #20637, #16224, #25837 ),
 .UNSPECIFIED., .F., .F.,
 ( 4, 2, 2, 2, 2, 2, 2, 4 ),
 ( 0.000000000000000000, 0.1249999999999999445, 0.2499999999999998890, 0.4999999999999997780, 0.6249999999999997780, 0.7499999999999996669, 0.8749999999999997780, 1.000000000000000000 ),
 .UNSPECIFIED. ) ;
#28532 = AXIS2_PLACEMENT_3D ( 'NONE', #8262, #5756, #15663 ) ;
#28533 = CARTESIAN_POINT ( 'NONE',  ( 0.6731456008920000400, -3.434453875705480108, -72.25672407562892374 ) ) ;
#28534 = TOROIDAL_SURFACE ( 'NONE', #1403, 30.50000000000000000, 3.000000000000000000 ) ;
#28535 = CARTESIAN_POINT ( 'NONE',  ( -21.68201525099999927, -17.64200409929999935, 222.0000000000000000 ) ) ;
#28536 = CARTESIAN_POINT ( 'NONE',  ( 0.3832430167449999980, -28.49789927060000139, 226.0423291289999952 ) ) ;
#28537 = EDGE_LOOP ( 'NONE', ( #20208, #28619, #17895, #5705 ) ) ;
#28538 = CARTESIAN_POINT ( 'NONE',  ( -19.58511357176576340, 20.00016057457926522, -0.2119832659756666626 ) ) ;
#28539 = CARTESIAN_POINT ( 'NONE',  ( 1.942707423728255778, -5.758494596869851989, -15.26414732020000464 ) ) ;
#28540 = CARTESIAN_POINT ( 'NONE',  ( 18.26905192694325208, -9.126265403884737282, -0.6999999999999784173 ) ) ;
#28541 = ADVANCED_FACE ( 'NONE', ( #17914 ), #10863, .F. ) ;
#28542 = CARTESIAN_POINT ( 'NONE',  ( 7.265485053589353370, -9.961462563069886755, 232.6627636948576878 ) ) ;
#28543 = ORIENTED_EDGE ( 'NONE', *, *, #26577, .T. ) ;
#28544 = CARTESIAN_POINT ( 'NONE',  ( -9.738910687886976447, -24.96785170200593384, 43.21714158840000408 ) ) ;
#28545 = LINE ( 'NONE', #6993, #12287 ) ;
#28546 = LINE ( 'NONE', #1503, #7763 ) ;
#28547 = CIRCLE ( 'NONE', #16971, 27.23548387100000312 ) ;
#28548 = EDGE_CURVE ( 'NONE', #2785, #3623, #25970, .T. ) ;
#28549 = CARTESIAN_POINT ( 'NONE',  ( 11.37440860439999923, -24.37257236010000128, -1.450121496399996213 ) ) ;
#28550 = B_SPLINE_CURVE_WITH_KNOTS ( 'NONE', 5,
 ( #18664, #24168, #28265, #2463, #12202, #23716 ),
 .UNSPECIFIED., .F., .F.,
 ( 6, 6 ),
 ( -2.319815200069999861, 0.000000000000000000 ),
 .UNSPECIFIED. ) ;
#28551 = EDGE_CURVE ( 'NONE', #25281, #30700, #7567, .T. ) ;
#28552 = CARTESIAN_POINT ( 'NONE',  ( 17.16657240420000008, 10.97998838177520931, -1.452769935612311825 ) ) ;
#28553 = DIRECTION ( 'NONE',  ( 5.962915006522623408E-16, 0.4383711467890811231, 0.8987940462991652613 ) ) ;
#28555 = EDGE_CURVE ( 'NONE', #29870, #3695, #25492, .T. ) ;
#28554 = CARTESIAN_POINT ( 'NONE',  ( 2.660567502109009752E-10, -9.320059656530233383, -25.35190844155029311 ) ) ;
#28556 = ORIENTED_EDGE ( 'NONE', *, *, #30368, .T. ) ;
#28557 = CARTESIAN_POINT ( 'NONE',  ( 28.50000000000000000, 1.065814103639999922E-14, 229.0000000000000000 ) ) ;
#28558 = CYLINDRICAL_SURFACE ( 'NONE', #6065, 26.80000000000002203 ) ;
#28559 = AXIS2_PLACEMENT_3D ( 'NONE', #14874, #24467, #2901 ) ;
#28560 = CARTESIAN_POINT ( 'NONE',  ( -27.79539923781684863, -0.5057481689248934931, 1.000000000000000888 ) ) ;
#28561 = AXIS2_PLACEMENT_3D ( 'NONE', #1174, #27920, #15336 ) ;
#28562 = B_SPLINE_CURVE_WITH_KNOTS ( 'NONE', 5,
 ( #8550, #6038, #13119, #15958, #20520, #30120, #18148, #1494, #10765, #25089, #29798, #27752, #6200, #8232, #3847 ),
 .UNSPECIFIED., .F., .F.,
 ( 6, 3, 3, 3, 6 ),
 ( 0.000000000000000000, 0.1000000000028631597, 0.3999999999999999667, 0.7000000000005724976, 1.000000000000000000 ),
 .UNSPECIFIED. ) ;
#28563 = CARTESIAN_POINT ( 'NONE',  ( -3.519556364420927785, -3.690466755798151866, -68.10000000002500542 ) ) ;
#28564 = DIRECTION ( 'NONE',  ( 1.000000000000000000, 0.000000000000000000, 0.000000000000000000 ) ) ;
#28565 = CARTESIAN_POINT ( 'NONE',  ( -4.850149637780369893, 0.09109815604563743785, -44.10000000002497700 ) ) ;
#28566 = PRODUCT_DEFINITION_SHAPE ( 'NONE', 'NONE',  #31135 ) ;
#28567 = ORIENTED_EDGE ( 'NONE', *, *, #4671, .T. ) ;
#28568 = CARTESIAN_POINT ( 'NONE',  ( -8.903108651239966420, -22.82508830966961000, 140.0000000000000000 ) ) ;
#28569 = CARTESIAN_POINT ( 'NONE',  ( -4.155524648305278568, -2.455537445457761869, -68.32382590962500046 ) ) ;
#28570 = VERTEX_POINT ( 'NONE', #13525 ) ;
#28571 = CARTESIAN_POINT ( 'NONE',  ( -26.84172470026987867, 2.049348509503662097, 0.000000000000000000 ) ) ;
#28572 = AXIS2_PLACEMENT_3D ( 'NONE', #2386, #11972, #26452 ) ;
#28573 = CARTESIAN_POINT ( 'NONE',  ( -4.320323480314920417, -1.509945384023513082, -50.40743646232499486 ) ) ;
#28574 = ORIENTED_EDGE ( 'NONE', *, *, #17527, .F. ) ;
#28575 = CARTESIAN_POINT ( 'NONE',  ( 0.000000000000000000, 0.000000000000000000, 210.0000000000000284 ) ) ;
#28576 = VECTOR ( 'NONE', #27282, 1000.000000000000000 ) ;
#28577 = CARTESIAN_POINT ( 'NONE',  ( -13.12132034329999897, 20.99999999999999645, -69.22132034359999864 ) ) ;
#28578 = CARTESIAN_POINT ( 'NONE',  ( 27.63177371540000138, -3.383804565909999813E-15, 42.63947604839999883 ) ) ;
#28579 = UNCERTAINTY_MEASURE_WITH_UNIT (LENGTH_MEASURE( 1.000000000000000082E-05 ), #2447, 'distance_accuracy_value', 'NONE');
#28580 = CARTESIAN_POINT ( 'NONE',  ( -0.5716039300045591132, -28.49445895580208443, 4.689815098000011062 ) ) ;
#28581 = CARTESIAN_POINT ( 'NONE',  ( 10.99999999979999998, 20.99999999990000887, -70.09999999999999432 ) ) ;
#28582 = LINE ( 'NONE', #2154, #28595 ) ;
#28583 = ORIENTED_EDGE ( 'NONE', *, *, #8017, .T. ) ;
#28584 = CARTESIAN_POINT ( 'NONE',  ( 9.500000000000000000, 21.70000000000000284, -64.10000000019999788 ) ) ;
#28585 = CARTESIAN_POINT ( 'NONE',  ( 0.5612683548718201409, -26.79446734662158747, 225.9574525908840883 ) ) ;
#28586 = CARTESIAN_POINT ( 'NONE',  ( 19.36601073090000114, 20.00000521309999968, 230.3593855350000013 ) ) ;
#28587 = FACE_OUTER_BOUND ( 'NONE', #21932, .T. ) ;
#28588 = CARTESIAN_POINT ( 'NONE',  ( 16.50668551557458485, -9.891786026617527483, -0.6999999999999784173 ) ) ;
#28589 = CARTESIAN_POINT ( 'NONE',  ( -0.6685465368700000965, -28.49273882800000024, 225.9009104920000084 ) ) ;
#28590 = DIRECTION ( 'NONE',  ( -1.000000000000000000, 0.000000000000000000, 0.000000000000000000 ) ) ;
#28591 = EDGE_CURVE ( 'NONE', #6179, #21098, #6061, .T. ) ;
#28592 = LINE ( 'NONE', #7799, #19812 ) ;
#28593 = CARTESIAN_POINT ( 'NONE',  ( 1.599333684796359067, -1.229093439949832334, 227.6412452702620897 ) ) ;
#28594 = CARTESIAN_POINT ( 'NONE',  ( 2.743362564037614248, -4.941860934411918649, -55.10172062782499580 ) ) ;
#28595 = VECTOR ( 'NONE', #6704, 1000.000000000000000 ) ;
#28596 = DIRECTION ( 'NONE',  ( -1.000000000000000000, 0.000000000000000000, -2.257144471330000330E-12 ) ) ;
#28597 = CARTESIAN_POINT ( 'NONE',  ( -16.74153468538860068, -7.902894514795387515, 0.000000000000000000 ) ) ;
#28598 = DIRECTION ( 'NONE',  ( 1.000000000000000000, 0.000000000000000000, 0.000000000000000000 ) ) ;
#28599 = EDGE_LOOP ( 'NONE', ( #17987, #7389, #12573, #14149 ) ) ;
#28600 = PLANE ( 'NONE',  #24813 ) ;
#28601 = ORIENTED_EDGE ( 'NONE', *, *, #27686, .F. ) ;
#28602 = CARTESIAN_POINT ( 'NONE',  ( -23.88727024800000009, -14.22229899360000083, 223.9574921880000034 ) ) ;
#28603 = AXIS2_PLACEMENT_3D ( 'NONE', #24175, #5290, #10165 ) ;
#28604 = EDGE_CURVE ( 'NONE', #10911, #13888, #20330, .T. ) ;
#28605 = CARTESIAN_POINT ( 'NONE',  ( -1.777987283592920020, 4.296653259772734046, -57.89652090042500276 ) ) ;
#28606 = ORIENTED_EDGE ( 'NONE', *, *, #12119, .T. ) ;
#28607 = ITEM_DEFINED_TRANSFORMATION ( 'NONE', 'NONE', #13322,  #17722 ) ;
#28608 = VERTEX_POINT ( 'NONE', #15889 ) ;
#28609 = FACE_OUTER_BOUND ( 'NONE', #16519, .T. ) ;
#28610 = ORIENTED_EDGE ( 'NONE', *, *, #25681, .F. ) ;
#28611 = CARTESIAN_POINT ( 'NONE',  ( 8.000000000250498289, -24.42231254078294000, -29.98460556443784952 ) ) ;
#28612 = ADVANCED_FACE ( 'NONE', ( #9108 ), #14829, .F. ) ;
#28613 = CARTESIAN_POINT ( 'NONE',  ( -8.699999999633741155, -14.31588153610736036, -40.15003283749538099 ) ) ;
#28614 = CARTESIAN_POINT ( 'NONE',  ( -22.97691952320000297, 16.89267704250000079, 223.0000000000000000 ) ) ;
#28615 = CARTESIAN_POINT ( 'NONE',  ( -2.595987296770099206, -16.63200279373747037, -109.8342699011499946 ) ) ;
#28616 = CARTESIAN_POINT ( 'NONE',  ( -20.30403093128963476, 20.00000000003735323, 1.000000000000000888 ) ) ;
#28617 = CARTESIAN_POINT ( 'NONE',  ( 2.773795135624238295, 4.340636736956414943, -4.263467428500004708 ) ) ;
#28618 = CARTESIAN_POINT ( 'NONE',  ( -23.31151963009999761, -20.60626745989999975, 230.2432540810000319 ) ) ;
#28619 = ORIENTED_EDGE ( 'NONE', *, *, #29371, .T. ) ;
#28620 = DIRECTION ( 'NONE',  ( 0.000000000000000000, 0.000000000000000000, -1.000000000000000000 ) ) ;
#28621 = CARTESIAN_POINT ( 'NONE',  ( -0.7560282158644051620, 4.289996408053716515, -20.33583244400001178 ) ) ;
#28622 = CARTESIAN_POINT ( 'NONE',  ( -1.086409578978756896, 3.499999999999999556, 230.7417114753006047 ) ) ;
#28623 = CARTESIAN_POINT ( 'NONE',  ( 24.82162974202869421, -12.51998933900577349, 5.310645680000003921 ) ) ;
#28624 = CYLINDRICAL_SURFACE ( 'NONE', #20678, 2.000000000000003553 ) ;
#28625 = DIRECTION ( 'NONE',  ( 0.000000000000000000, 0.000000000000000000, 1.000000000000000000 ) ) ;
#28626 = CARTESIAN_POINT ( 'NONE',  ( -19.76607646299421361, 19.51851687837242366, 0.7753390690000139251 ) ) ;
#28627 = DIRECTION ( 'NONE',  ( 0.000000000000000000, 0.000000000000000000, -1.000000000000000000 ) ) ;
#28628 = CARTESIAN_POINT ( 'NONE',  ( -23.54244930407671532, -12.80639529791832842, 4.123351189496611724 ) ) ;
#28629 = CARTESIAN_POINT ( 'NONE',  ( -13.99999999969999820, 20.99999999999999645, -51.10000000000000142 ) ) ;
#28630 = EDGE_CURVE ( 'NONE', #10257, #25445, #2262, .T. ) ;
#28631 = CARTESIAN_POINT ( 'NONE',  ( 11.00000000000000000, 27.10555629988041204, -61.14106941751904856 ) ) ;
#28632 = EDGE_LOOP ( 'NONE', ( #3506, #29434, #27012, #16551, #20244, #2097, #10413, #16709 ) ) ;
#28633 = CARTESIAN_POINT ( 'NONE',  ( -10.24010329480000081, 19.99999999999999645, -1.477379946600000604 ) ) ;
#28634 = CARTESIAN_POINT ( 'NONE',  ( -15.75643827102668482, -9.267172193162394933, -0.6999999999999784173 ) ) ;
#28635 = FACE_OUTER_BOUND ( 'NONE', #24807, .T. ) ;
#28636 = VERTEX_POINT ( 'NONE', #22126 ) ;
#28637 = FACE_OUTER_BOUND ( 'NONE', #26776, .T. ) ;
#28638 = DIRECTION ( 'NONE',  ( 0.000000000000000000, 0.000000000000000000, 1.000000000000000000 ) ) ;
#28639 = ORIENTED_EDGE ( 'NONE', *, *, #24049, .T. ) ;
#28640 = VERTEX_POINT ( 'NONE', #10167 ) ;
#28641 = CARTESIAN_POINT ( 'NONE',  ( 0.000000000000000000, 0.000000000000000000, 0.000000000000000000 ) ) ;
#28642 = VERTEX_POINT ( 'NONE', #5893 ) ;
#28643 = CARTESIAN_POINT ( 'NONE',  ( -0.6521609807820000215, -27.79292263629999837, 224.0990923460000204 ) ) ;
#28644 = VERTEX_POINT ( 'NONE', #8563 ) ;
#28645 = FACE_OUTER_BOUND ( 'NONE', #20504, .T. ) ;
#28646 = CARTESIAN_POINT ( 'NONE',  ( 23.81866173088643635, 14.33570044285385947, 3.899998581000013509 ) ) ;
#28647 = EDGE_CURVE ( 'NONE', #24608, #26791, #26671, .T. ) ;
#28648 = DIRECTION ( 'NONE',  ( 1.000000000000000000, -1.224606353819998843E-16, 0.000000000000000000 ) ) ;
#28649 = CARTESIAN_POINT ( 'NONE',  ( 0.2553064023551063766, 4.393912938272285906, -35.69999999999999574 ) ) ;
#28650 = CARTESIAN_POINT ( 'NONE',  ( 19.40179356770304864, 20.00003053714920043, -0.3254732509765126403 ) ) ;
#28651 = CARTESIAN_POINT ( 'NONE',  ( -3.797496571118017528, -0.6966955563414738428, -0.6999999999999995115 ) ) ;
#28652 = CARTESIAN_POINT ( 'NONE',  ( 10.89131017139999891, -24.73114799890000270, -1.811764705899998606 ) ) ;
#28653 = FACE_OUTER_BOUND ( 'NONE', #27090, .T. ) ;
#28654 = CARTESIAN_POINT ( 'NONE',  ( -1.102325287918849650, -5.983340188646091740, -3.525234013000005717 ) ) ;
#28655 = CARTESIAN_POINT ( 'NONE',  ( 5.536217179945332134, 2.001767383715431503, -25.51249766019999399 ) ) ;
#28656 = CARTESIAN_POINT ( 'NONE',  ( -16.06988964647317886, -8.208161364834239748, 0.000000000000000000 ) ) ;
#28657 = VECTOR ( 'NONE', #7250, 1000.000000000000000 ) ;
#28658 = PLANE ( 'NONE',  #12175 ) ;
#28659 = EDGE_CURVE ( 'NONE', #12806, #17991, #13921, .T. ) ;
#28660 = CARTESIAN_POINT ( 'NONE',  ( 24.14840829003134104, 13.77363891352294267, 5.901294549000013490 ) ) ;
#28661 = DIRECTION ( 'NONE',  ( 0.000000000000000000, 0.000000000000000000, -1.000000000000000000 ) ) ;
#28662 = CARTESIAN_POINT ( 'NONE',  ( -4.646804529178781173, -0.2974863596997279203, -4.148838774900000637 ) ) ;
#28663 = ADVANCED_FACE ( 'NONE', ( #11252 ), #25428, .T. ) ;
#28664 = CARTESIAN_POINT ( 'NONE',  ( -24.50000001620000134, 3.000285568850000245E-15, 190.0000000039999861 ) ) ;
#28665 = CARTESIAN_POINT ( 'NONE',  ( 7.638687372243864182, -5.597492073922072819, -34.74908987243156133 ) ) ;
#28666 = CARTESIAN_POINT ( 'NONE',  ( 16.09014176753201752, 11.26838425375450115, -4.336808689942017243E-16 ) ) ;
#28667 = ORIENTED_EDGE ( 'NONE', *, *, #17728, .F. ) ;
#28668 = AXIS2_PLACEMENT_3D ( 'NONE', #18538, #9242, #25195 ) ;
#28669 = EDGE_CURVE ( 'NONE', #5834, #24961, #8700, .T. ) ;
#28670 = DIRECTION ( 'NONE',  ( 1.000000000000000000, 0.000000000000000000, 0.000000000000000000 ) ) ;
#28671 = CARTESIAN_POINT ( 'NONE',  ( -4.273414424137721213, 4.913340199448848367, -28.58728588869999143 ) ) ;
#28672 = VERTEX_POINT ( 'NONE', #17846 ) ;
#28673 = CARTESIAN_POINT ( 'NONE',  ( -10.00000000070000183, -25.00000000000000000, -26.16393202249999916 ) ) ;
#28674 = CARTESIAN_POINT ( 'NONE',  ( 23.83861932470720291, 15.61961844235199948, 4.689445052000001724 ) ) ;
#28675 = ORIENTED_EDGE ( 'NONE', *, *, #3704, .T. ) ;
#28676 = EDGE_LOOP ( 'NONE', ( #163, #8989, #25148, #23282 ) ) ;
#28677 = VERTEX_POINT ( 'NONE', #25579 ) ;
#28678 = CIRCLE ( 'NONE', #30176, 26.80000000000000071 ) ;
#28679 = ORIENTED_EDGE ( 'NONE', *, *, #3232, .F. ) ;
#28680 = CARTESIAN_POINT ( 'NONE',  ( -17.49999999969999820, -29.92349012522117846, -29.18094649280867614 ) ) ;
#28681 = EDGE_CURVE ( 'NONE', #15176, #2437, #27609, .T. ) ;
#28682 = DIRECTION ( 'NONE',  ( 0.000000000000000000, 0.000000000000000000, -1.000000000000000000 ) ) ;
#28683 = CARTESIAN_POINT ( 'NONE',  ( -0.8668912886149129360, 2.622943012334922219, -67.92365636629153869 ) ) ;
#28684 = EDGE_LOOP ( 'NONE', ( #16021, #11226, #23990, #6133 ) ) ;
#28685 = FACE_OUTER_BOUND ( 'NONE', #22925, .T. ) ;
#28686 = B_SPLINE_CURVE_WITH_KNOTS ( 'NONE', 5,
 ( #835, #29614, #8048, #989, #20480, #16074, #18107, #29925, #10723 ),
 .UNSPECIFIED., .F., .F.,
 ( 6, 3, 6 ),
 ( 0.000000000000000000, 1.646696145469999983, 2.782752055940000080 ),
 .UNSPECIFIED. ) ;
#28687 = DIRECTION ( 'NONE',  ( 1.881554647690000340E-09, 1.000000000000000000, 0.000000000000000000 ) ) ;
#28688 = CARTESIAN_POINT ( 'NONE',  ( -7.999999999695856623, -18.27877680370596636, -30.94409471158115110 ) ) ;
#28689 = CARTESIAN_POINT ( 'NONE',  ( 0.1059454459490000028, -28.50005195860000029, 226.0959520840000039 ) ) ;
#28690 = ORIENTED_EDGE ( 'NONE', *, *, #11149, .T. ) ;
#28691 = ADVANCED_FACE ( 'NONE', ( #1188 ), #10052, .F. ) ;
#28692 = CARTESIAN_POINT ( 'NONE',  ( -19.73536700009918121, 20.00033765927653917, -0.09955921259694186509 ) ) ;
#28693 = AXIS2_PLACEMENT_3D ( 'NONE', #26050, #4489, #18586 ) ;
#28694 = CARTESIAN_POINT ( 'NONE',  ( 5.320018516182488000, -2.211191048809329374, -17.27122516810000619 ) ) ;
#28695 = DIRECTION ( 'NONE',  ( 2.764840495839172918E-12, 0.9128796883888953273, -0.4082287037029531107 ) ) ;
#28696 = CARTESIAN_POINT ( 'NONE',  ( -8.699999999711218734, -30.00985298778766008, -28.70958934910558469 ) ) ;
#28697 = VERTEX_POINT ( 'NONE', #13611 ) ;
#28698 = CARTESIAN_POINT ( 'NONE',  ( -27.92857142820000149, 5.329070518200000398E-15, 137.9396849850000137 ) ) ;
#28699 = LINE ( 'NONE', #18632, #5230 ) ;
#28700 = CARTESIAN_POINT ( 'NONE',  ( 26.80000000069999899, -3.281945028320000125E-15, 92.88981852279999885 ) ) ;
#28701 = CARTESIAN_POINT ( 'NONE',  ( 8.000000000285856672, -13.61361098174325868, -34.64062768040190576 ) ) ;
#28702 = B_SPLINE_CURVE_WITH_KNOTS ( 'NONE', 3,
 ( #15088, #777, #27044, #29398, #20121, #15233 ),
 .UNSPECIFIED., .F., .F.,
 ( 4, 2, 4 ),
 ( 0.000000000000000000, 0.5000000000000000000, 1.000000000000000000 ),
 .UNSPECIFIED. ) ;
#28703 = CARTESIAN_POINT ( 'NONE',  ( -5.072625435919005586E-16, -3.702906486519338703E-16, 226.6412452697749984 ) ) ;
#28704 = CARTESIAN_POINT ( 'NONE',  ( 17.18658402241074867, -10.09981795543446736, -0.6999999999999784173 ) ) ;
#28705 = CARTESIAN_POINT ( 'NONE',  ( 11.00000000000000000, 25.22617105830878614, -61.82510970417090590 ) ) ;
#28706 = VERTEX_POINT ( 'NONE', #15971 ) ;
#28707 = CARTESIAN_POINT ( 'NONE',  ( 17.14656078602323319, -7.900182044548062166, -0.6999999999999784173 ) ) ;
#28708 = CARTESIAN_POINT ( 'NONE',  ( -17.40631047800548004, -8.049650370842703850, -0.6999999999999784173 ) ) ;
#28709 = CARTESIAN_POINT ( 'NONE',  ( -27.61317819196527878, 4.248065245814218294, 0.2686740700000300741 ) ) ;
#28710 = CARTESIAN_POINT ( 'NONE',  ( -2.744116393020877620, -4.299119443564640264, -68.10000000002500542 ) ) ;
#28711 = VERTEX_POINT ( 'NONE', #4015 ) ;
#28712 = DIRECTION ( 'NONE',  ( -1.000000000000000000, 0.000000000000000000, 0.000000000000000000 ) ) ;
#28713 = VERTEX_POINT ( 'NONE', #20861 ) ;
#28714 = DIRECTION ( 'NONE',  ( 1.595945597898660305E-12, -0.7071067811865475727, -0.7071067811865475727 ) ) ;
#28715 = ADVANCED_FACE ( 'NONE', ( #30459 ), #16585, .T. ) ;
#28716 = CARTESIAN_POINT ( 'NONE',  ( 0.3196029497759475535, 5.089975830446680227, -69.83875473022500557 ) ) ;
#28717 = VERTEX_POINT ( 'NONE', #13928 ) ;
#28718 = CARTESIAN_POINT ( 'NONE',  ( 0.1206012444329082195, -5.909053133798479962, -25.41888333260000721 ) ) ;
#28719 = CARTESIAN_POINT ( 'NONE',  ( 2.910560681360000016E-11, 19.99999999999999645, -45.10000000000000142 ) ) ;
#28720 = EDGE_CURVE ( 'NONE', #25281, #26584, #5274, .T. ) ;
#28721 = ADVANCED_FACE ( 'NONE', ( #28849 ), #5175, .T. ) ;
#28722 = CARTESIAN_POINT ( 'NONE',  ( 0.8945918243927832858, -4.819150861182647461, -58.74125695792500323 ) ) ;
#28723 = DIRECTION ( 'NONE',  ( 0.000000000000000000, 1.000000000000000000, 0.000000000000000000 ) ) ;
#28724 = CARTESIAN_POINT ( 'NONE',  ( -10.70000000000117168, -25.27195344040325864, -25.92068947064144524 ) ) ;
#28725 = CARTESIAN_POINT ( 'NONE',  ( 3.483928249571823343, 0.9656592618119906879, 230.7696496080370423 ) ) ;
#28726 = CARTESIAN_POINT ( 'NONE',  ( 18.95046173579999760, -18.95046173579999760, 143.2171415880000040 ) ) ;
#28727 = ORIENTED_EDGE ( 'NONE', *, *, #20977, .F. ) ;
#28728 = CARTESIAN_POINT ( 'NONE',  ( -5.304254813150000639E-10, 4.380584783799999468E-10, 230.0000000000000000 ) ) ;
#28729 = CARTESIAN_POINT ( 'NONE',  ( 24.55806919409999978, -14.46257963250000067, 226.0798541909999813 ) ) ;
#28730 = CARTESIAN_POINT ( 'NONE',  ( -10.18299983019999821, -6.475798291150000274, 231.9999989789999972 ) ) ;
#28731 = CARTESIAN_POINT ( 'NONE',  ( -15.73360964098195147, -8.979988381493612337, 0.000000000000000000 ) ) ;
#28732 = VECTOR ( 'NONE', #13164, 1000.000000000000000 ) ;
#28733 = CARTESIAN_POINT ( 'NONE',  ( 16.63016908727803056, -9.971084190299466243, -0.6999999999999784173 ) ) ;
#28734 = CARTESIAN_POINT ( 'NONE',  ( -0.8738876050170000243, -27.78662806160000187, 225.6801695290000112 ) ) ;
#28735 = DIRECTION ( 'NONE',  ( -0.000000000000000000, -0.000000000000000000, -1.000000000000000000 ) ) ;
#28736 = CARTESIAN_POINT ( 'NONE',  ( 0.000000000000000000, 0.000000000000000000, 115.0000000000000000 ) ) ;
#28737 = VECTOR ( 'NONE', #600, 1000.000000000000000 ) ;
#28738 = CARTESIAN_POINT ( 'NONE',  ( 7.797918471980000099, 19.99999999999999645, -43.60208152801600079 ) ) ;
#28739 = CARTESIAN_POINT ( 'NONE',  ( -6.398352591652365362, -16.59129340813300502, -74.91706649750152280 ) ) ;
#28740 = CYLINDRICAL_SURFACE ( 'NONE', #5271, 3.000000000000002220 ) ;
#28741 = CARTESIAN_POINT ( 'NONE',  ( 26.80000000069999899, -3.281945028320000125E-15, 86.78285841090000474 ) ) ;
#28742 = ORIENTED_EDGE ( 'NONE', *, *, #4438, .F. ) ;
#28743 = ORIENTED_EDGE ( 'NONE', *, *, #4787, .F. ) ;
#28744 = PLANE ( 'NONE',  #6915 ) ;
#28745 = CONICAL_SURFACE ( 'NONE', #22223, 11.99999999999999467, 1.243158134259999770 ) ;
#28746 = CARTESIAN_POINT ( 'NONE',  ( -1.989652436383612555, 4.808159600214577445, -57.94652090042499992 ) ) ;
#28747 = ORIENTED_EDGE ( 'NONE', *, *, #1679, .T. ) ;
#28748 = EDGE_CURVE ( 'NONE', #11411, #18136, #3042, .T. ) ;
#28749 = VERTEX_POINT ( 'NONE', #23689 ) ;
#28750 = CARTESIAN_POINT ( 'NONE',  ( -17.39770507061216165, -25.62059377601494603, -23.42289786304042920 ) ) ;
#28751 = EDGE_CURVE ( 'NONE', #27161, #29903, #18812, .T. ) ;
#28752 = EDGE_LOOP ( 'NONE', ( #21209, #20640, #2518, #30226 ) ) ;
#28753 = SURFACE_SIDE_STYLE ('',( #454 ) ) ;
#28754 = CARTESIAN_POINT ( 'NONE',  ( 12.55799324160000019, 20.99999999999999645, -55.95247857500000066 ) ) ;
#28755 = CARTESIAN_POINT ( 'NONE',  ( -27.79539923781684507, -0.5057481689249112566, 2.400000000000013234 ) ) ;
#28756 = CARTESIAN_POINT ( 'NONE',  ( -23.55444264242456498, 16.04540112444970390, 8.000000000000007105 ) ) ;
#28757 = CARTESIAN_POINT ( 'NONE',  ( 19.80526555972147307, 19.50877392102524155, 3.000000000000002665 ) ) ;
#28758 = CARTESIAN_POINT ( 'NONE',  ( -10.69999999930000101, -27.00000000000000000, -25.39999999999999858 ) ) ;
#28759 = CARTESIAN_POINT ( 'NONE',  ( 4.347198243976404974, 0.5700341643805826308, -5.626979598400000171 ) ) ;
#28760 = AXIS2_PLACEMENT_3D ( 'NONE', #10490, #8735, #3706 ) ;
#28761 = CARTESIAN_POINT ( 'NONE',  ( -22.91194469939999934, -20.25306243529999861, 230.5592437530000041 ) ) ;
#28762 = ORIENTED_EDGE ( 'NONE', *, *, #8467, .T. ) ;
#28763 = CARTESIAN_POINT ( 'NONE',  ( -24.25909092259999866, -14.95913241689999928, 224.2397348780000073 ) ) ;
#28764 = CARTESIAN_POINT ( 'NONE',  ( 1.771049722044198971, -6.234229536879996481, -21.89535708919999735 ) ) ;
#28765 = CARTESIAN_POINT ( 'NONE',  ( -27.79999999999999716, -2.359477751120000078E-11, 227.5999999999999943 ) ) ;
#28766 = CARTESIAN_POINT ( 'NONE',  ( 24.34137756859324853, -13.42980563341176037, 6.099998581000020792 ) ) ;
#28767 = DIRECTION ( 'NONE',  ( 5.962915006522623408E-16, 0.4383711467890810676, 0.8987940462991651502 ) ) ;
#28768 = CARTESIAN_POINT ( 'NONE',  ( 19.80538173169999894, 19.50875421069999760, 226.9999998930000231 ) ) ;
#28769 = CARTESIAN_POINT ( 'NONE',  ( -4.592700181227121980, -1.655560342997616896, -44.41497819512500200 ) ) ;
#28770 = CARTESIAN_POINT ( 'NONE',  ( -10.69999999999999929, -123.9932870109000049, -32.02938626120000265 ) ) ;
#28771 = CARTESIAN_POINT ( 'NONE',  ( -24.98081131316241255, -13.71897606304888662, 4.999998581000003384 ) ) ;
#28772 = CARTESIAN_POINT ( 'NONE',  ( -24.92639508767336309, -13.81781708088548122, 5.506973469000003618 ) ) ;
#28773 = EDGE_CURVE ( 'NONE', #23358, #28202, #2123, .T. ) ;
#28774 = CARTESIAN_POINT ( 'NONE',  ( 4.898425415290000099E-16, -2.000000000000000000, 229.2412452703699728 ) ) ;
#28775 = ORIENTED_EDGE ( 'NONE', *, *, #8409, .F. ) ;
#28776 = CARTESIAN_POINT ( 'NONE',  ( 6.052054646587431641, -17.25211205318136720, -75.15758481454749074 ) ) ;
#28777 = FILL_AREA_STYLE_COLOUR ( '', #27037 ) ;
#28778 = CARTESIAN_POINT ( 'NONE',  ( 7.768677137030000068, 16.06355773770000184, 230.7531949689999919 ) ) ;
#28779 = ORIENTED_EDGE ( 'NONE', *, *, #22083, .T. ) ;
#28780 = DIRECTION ( 'NONE',  ( 5.962915006522623408E-16, 0.4383711467890811231, 0.8987940462991652613 ) ) ;
#28781 = CARTESIAN_POINT ( 'NONE',  ( -1.460566089872938900, -4.291843709425553044, -46.99520033292500187 ) ) ;
#28782 = ORIENTED_EDGE ( 'NONE', *, *, #30813, .T. ) ;
#28783 = VERTEX_POINT ( 'NONE', #9041 ) ;
#28784 = DIRECTION ( 'NONE',  ( 0.000000000000000000, 0.000000000000000000, 1.000000000000000000 ) ) ;
#28785 = ORIENTED_EDGE ( 'NONE', *, *, #26568, .F. ) ;
#28786 = CARTESIAN_POINT ( 'NONE',  ( -0.1033151399490000039, -27.80006701330000141, 223.9040511909999793 ) ) ;
#28787 = ORIENTED_EDGE ( 'NONE', *, *, #2788, .F. ) ;
#28788 = AXIS2_PLACEMENT_3D ( 'NONE', #14323, #16657, #23923 ) ;
#28789 = DIRECTION ( 'NONE',  ( 1.000000000000000000, 0.000000000000000000, 0.000000000000000000 ) ) ;
#28790 = FACE_BOUND ( 'NONE', #21255, .T. ) ;
#28791 = CARTESIAN_POINT ( 'NONE',  ( 0.2353820488414976597, 4.569370376363825592, -35.70000000000000284 ) ) ;
#28792 = CARTESIAN_POINT ( 'NONE',  ( 19.84014010780992621, 20.00037855652159990, -0.006061537342544804675 ) ) ;
#28793 = CARTESIAN_POINT ( 'NONE',  ( -24.81746041937532965, 14.01353061208509310, 6.079865099000020479 ) ) ;
#28794 = CYLINDRICAL_SURFACE ( 'NONE', #6585, 1.999999999999999334 ) ;
#28795 = CARTESIAN_POINT ( 'NONE',  ( -19.76603762889999771, 19.51852293520000003, 229.2245375310000099 ) ) ;
#28796 = CARTESIAN_POINT ( 'NONE',  ( -4.184186767956295405, -1.312611723764782523, -10.02323088899999881 ) ) ;
#28797 = CARTESIAN_POINT ( 'NONE',  ( 4.370697773661015972, 1.580342671372847230, -26.01249766020000820 ) ) ;
#28798 = CARTESIAN_POINT ( 'NONE',  ( 13.00000000000000000, 23.13259184047820582, -60.45875467758818189 ) ) ;
#28799 =( BOUNDED_CURVE ( )  B_SPLINE_CURVE ( 5, ( #16765, #26386, #14424, #24023, #13799, #2465 ),
 .UNSPECIFIED., .F., .T. ) 
 B_SPLINE_CURVE_WITH_KNOTS ( ( 6, 6 ),
 ( 1.352733214049999910, 7.601046855679999936 ),
 .UNSPECIFIED. ) 
 CURVE ( )  GEOMETRIC_REPRESENTATION_ITEM ( )  RATIONAL_B_SPLINE_CURVE ( ( 0.7240463347079999501, 0.5103476925150000065, 0.3838633578460000084, 0.3093277433949999655, 0.2672497422500000330, 0.2539127278980000124 ) ) 
 REPRESENTATION_ITEM ( '' )  );
#28800 = DIRECTION ( 'NONE',  ( 1.000000000000000000, -3.981000000000000101E-12, 1.940999999999999908E-12 ) ) ;
#28801 = CARTESIAN_POINT ( 'NONE',  ( 19.49313413869766620, 19.58644549600961327, 0.4409083710000261114 ) ) ;
#28802 = CARTESIAN_POINT ( 'NONE',  ( -16.85343921394901301, 12.09981795542885585, -0.6999999999999784173 ) ) ;
#28803 = CARTESIAN_POINT ( 'NONE',  ( 4.116710911288352648, -1.508563155650267884, -5.836105321700007842 ) ) ;
#28804 = EDGE_CURVE ( 'NONE', #17105, #17588, #9390, .T. ) ;
#28805 = COLOUR_RGB ( '', 0.09019608, 0.27058824, 0.51372549) ;
#28806 = B_SPLINE_CURVE_WITH_KNOTS ( 'NONE', 5,
 ( #4589, #4290, #16235, #25851, #9467, #14045, #21274, #28508, #23496 ),
 .UNSPECIFIED., .F., .F.,
 ( 6, 3, 6 ),
 ( 8.011061266649999624, 8.831591450809998634, 9.652121634960000307 ),
 .UNSPECIFIED. ) ;
#28807 = CARTESIAN_POINT ( 'NONE',  ( 23.78820504408419723, -14.38694252465835710, 5.289459540744400279 ) ) ;
#28808 = CARTESIAN_POINT ( 'NONE',  ( 14.74592307778630484, -25.66596092470346591, -23.39674041003665650 ) ) ;
#28809 = CARTESIAN_POINT ( 'NONE',  ( -8.903108651239966420, -22.82508830966961000, 40.00000000000000000 ) ) ;
#28810 = ORIENTED_EDGE ( 'NONE', *, *, #19986, .T. ) ;
#28811 = EDGE_CURVE ( 'NONE', #17179, #24995, #18749, .T. ) ;
#28812 = CARTESIAN_POINT ( 'NONE',  ( 0.5537481963838299936, -28.49486543565701169, 3.899998581000013509 ) ) ;
#28813 = DIRECTION ( 'NONE',  ( 0.000000000000000000, 0.000000000000000000, -1.000000000000000000 ) ) ;
#28814 = VERTEX_POINT ( 'NONE', #18637 ) ;
#28815 = CARTESIAN_POINT ( 'NONE',  ( 24.80399018339999628, -14.03663607480000053, 226.0798554400000171 ) ) ;
#28816 = CARTESIAN_POINT ( 'NONE',  ( 24.29089620522634263, 14.90695587088477581, 3.920145809000019632 ) ) ;
#28817 = ORIENTED_EDGE ( 'NONE', *, *, #846, .T. ) ;
#28818 = ORIENTED_EDGE ( 'NONE', *, *, #7956, .T. ) ;
#28819 = ORIENTED_EDGE ( 'NONE', *, *, #12985, .F. ) ;
#28820 = PRESENTATION_STYLE_ASSIGNMENT (( #30895 ) ) ;
#28821 = ORIENTED_EDGE ( 'NONE', *, *, #19672, .T. ) ;
#28822 = DIRECTION ( 'NONE',  ( -1.000000000000000000, 0.000000000000000000, 0.000000000000000000 ) ) ;
#28823 = AXIS2_PLACEMENT_3D ( 'NONE', #18609, #13415, #20502 ) ;
#28824 = DIRECTION ( 'NONE',  ( -1.000000000000000000, 0.000000000000000000, -6.771000000000000128E-12 ) ) ;
#28825 = EDGE_CURVE ( 'NONE', #10713, #12574, #19772, .T. ) ;
#28827 = CARTESIAN_POINT ( 'NONE',  ( -2.064060864691235508, 2.140523675421532879, -68.09924264536260807 ) ) ;
#28826 = AXIS2_PLACEMENT_3D ( 'NONE', #12070, #2172, #31115 ) ;
#28828 = AXIS2_PLACEMENT_3D ( 'NONE', #281, #9861, #26692 ) ;
#28829 = ORIENTED_EDGE ( 'NONE', *, *, #3136, .F. ) ;
#28830 = DIRECTION ( 'NONE',  ( 0.000000000000000000, 0.000000000000000000, 1.000000000000000000 ) ) ;
#28831 = VECTOR ( 'NONE', #30667, 999.9999999999998863 ) ;
#28832 = DIRECTION ( 'NONE',  ( 1.000000000000000000, 0.000000000000000000, 0.000000000000000000 ) ) ;
#28833 = CARTESIAN_POINT ( 'NONE',  ( 19.49313413869766620, 19.58644549600961327, 0.4409083710000261114 ) ) ;
#28834 = CARTESIAN_POINT ( 'NONE',  ( -20.22682926819999949, -26.99999999999973355, -28.39999999990017798 ) ) ;
#28835 = CARTESIAN_POINT ( 'NONE',  ( 3.532196160932838502, -3.333259304328497485, -0.6997801443041695713 ) ) ;
#28836 = ORIENTED_EDGE ( 'NONE', *, *, #5558, .T. ) ;
#28837 = CARTESIAN_POINT ( 'NONE',  ( -20.50713102034104551, 18.79635956957924492, 4.000000085000010586 ) ) ;
#28838 = B_SPLINE_SURFACE_WITH_KNOTS ( 'NONE', 5, 1, ( 
 ( #29255, #2987 ),
 ( #12577, #4888 ),
 ( #5953, #24857 ),
 ( #946, #25318 ),
 ( #10535, #15402 ),
 ( #3132, #8306 ),
 ( #22646, #3286 ),
 ( #12890, #1089 ),
 ( #792, #27506 ),
 ( #17901, #27057 ),
 ( #13037, #12732 ),
 ( #25002, #29722 ),
 ( #5494, #22497 ),
 ( #5804, #13352 ),
 ( #10680, #15550 ) ),
 .UNSPECIFIED., .F., .F., .F.,
 ( 6, 3, 3, 3, 6 ),
 ( 2, 2 ),
 ( 0.000000000000000000, 0.5239010160460000343, 1.047802032090000113, 1.571703048140000059, 1.746336720149999966 ),
 ( -0.7000000000009999335, 2.556026163500000058E-06 ),
 .UNSPECIFIED. ) ;
#28839 = CARTESIAN_POINT ( 'NONE',  ( -2.766209873889304394, 4.939907206908331183, -15.67761783620001204 ) ) ;
#28840 = CARTESIAN_POINT ( 'NONE',  ( -8.699999999884559188, -60.75400889059604737, -3.446705952705766407 ) ) ;
#28841 = CARTESIAN_POINT ( 'NONE',  ( -27.54391552369999729, 3.373045395949999841E-15, 142.9562530130000084 ) ) ;
#28842 = ORIENTED_EDGE ( 'NONE', *, *, #30649, .F. ) ;
#28843 = DIRECTION ( 'NONE',  ( 0.000000000000000000, -0.3420201433259318913, 0.9396926207858126157 ) ) ;
#28844 = CARTESIAN_POINT ( 'NONE',  ( 28.49999999990000177, 2.434992796449999553, 222.0000000000000000 ) ) ;
#28845 = CARTESIAN_POINT ( 'NONE',  ( 22.87891075595186763, -13.95728375069770877, 5.909812224949991588 ) ) ;
#28846 = DIRECTION ( 'NONE',  ( 0.3633921898465276024, -0.9316362575375355393, 0.000000000000000000 ) ) ;
#28847 = CARTESIAN_POINT ( 'NONE',  ( 2.473875800322225427, -5.003071188766746502, -67.61367454182500580 ) ) ;
#28848 = EDGE_CURVE ( 'NONE', #11577, #27319, #16276, .T. ) ;
#28849 = FACE_OUTER_BOUND ( 'NONE', #3048, .T. ) ;
#28850 = CYLINDRICAL_SURFACE ( 'NONE', #29833, 6.000000000000001776 ) ;
#28851 = CIRCLE ( 'NONE', #8215, 2.000000000000000000 ) ;
#28852 = ORIENTED_EDGE ( 'NONE', *, *, #11146, .F. ) ;
#28853 = CARTESIAN_POINT ( 'NONE',  ( 28.50000000000000000, 8.881784197000000993E-16, 222.0000000000000000 ) ) ;
#28854 = CARTESIAN_POINT ( 'NONE',  ( 17.83931934270000141, 20.00000000000000000, 230.3499999999999943 ) ) ;
#28855 =( GEOMETRIC_REPRESENTATION_CONTEXT ( 3 ) GLOBAL_UNCERTAINTY_ASSIGNED_CONTEXT ( ( #19132 ) ) GLOBAL_UNIT_ASSIGNED_CONTEXT ( ( #22909, #13768, #30619 ) ) REPRESENTATION_CONTEXT ( 'NONE', 'WORKASPACE' ) );
#28856 = VECTOR ( 'NONE', #30731, 1000.000000000000000 ) ;
#28857 = ADVANCED_FACE ( 'NONE', ( #21632 ), #26792, .T. ) ;
#28858 = CIRCLE ( 'NONE', #12778, 27.92857142840000151 ) ;
#28859 = VECTOR ( 'NONE', #11288, 1000.000000000000000 ) ;
#28860 = CARTESIAN_POINT ( 'NONE',  ( -2.744116393020877620, -4.299119443564640264, -68.10000000002500542 ) ) ;
#28861 = CARTESIAN_POINT ( 'NONE',  ( -4.147568857911904772, -2.928510985069560757, -68.10000000002500542 ) ) ;
#28862 = ORIENTED_EDGE ( 'NONE', *, *, #16369, .F. ) ;
#28863 = DIRECTION ( 'NONE',  ( 0.000000000000000000, 1.000000000000000000, 0.000000000000000000 ) ) ;
#28864 =( NAMED_UNIT ( * ) SI_UNIT ( $, .STERADIAN. ) SOLID_ANGLE_UNIT ( ) );
#28865 = ORIENTED_EDGE ( 'NONE', *, *, #23894, .F. ) ;
#28866 = CARTESIAN_POINT ( 'NONE',  ( 8.000000000287716517, -16.96959321760095563, -37.81493174583665251 ) ) ;
#28867 = APPLICATION_CONTEXT ( 'automotive_design' ) ;
#28868 =( GEOMETRIC_REPRESENTATION_CONTEXT ( 3 ) GLOBAL_UNCERTAINTY_ASSIGNED_CONTEXT ( ( #5577 ) ) GLOBAL_UNIT_ASSIGNED_CONTEXT ( ( #22570, #17823, #22253 ) ) REPRESENTATION_CONTEXT ( 'NONE', 'WORKASPACE' ) );
#28869 = CARTESIAN_POINT ( 'NONE',  ( 0.9758793680739014098, -27.78334643823060546, 3.997481721999984750 ) ) ;
#28870 = VERTEX_POINT ( 'NONE', #28704 ) ;
#28871 = CARTESIAN_POINT ( 'NONE',  ( -3.878879136156893281, -1.961445906012333706, -27.96472909260000606 ) ) ;
#28872 = CONTEXT_DEPENDENT_SHAPE_REPRESENTATION ( #29274, #29760 ) ;
#28873 = CARTESIAN_POINT ( 'NONE',  ( 2.131628207279999844E-14, 1.421085471519999843E-14, 230.0904314459999966 ) ) ;
#28874 = B_SPLINE_CURVE_WITH_KNOTS ( 'NONE', 3,
 ( #12917, #22527, #8178, #972, #26773, #20158 ),
 .UNSPECIFIED., .F., .F.,
 ( 4, 2, 4 ),
 ( 0.000000000000000000, 0.5000000000000000000, 1.000000000000000000 ),
 .UNSPECIFIED. ) ;
#28875 = EDGE_CURVE ( 'NONE', #1244, #27171, #19109, .T. ) ;
#28876 = CARTESIAN_POINT ( 'NONE',  ( 0.7192951553254764985, 4.518739695583327887, -54.41500058692499664 ) ) ;
#28878 = CARTESIAN_POINT ( 'NONE',  ( -26.80000000000000071, 6.217248937899999413E-15, 136.7828584120000244 ) ) ;
#28877 = AXIS2_PLACEMENT_3D ( 'NONE', #13058, #3306, #22664 ) ;
#28879 = CONICAL_SURFACE ( 'NONE', #19839, 4.987531172069999741, 1.047197551199999799 ) ;
#28880 = CARTESIAN_POINT ( 'NONE',  ( -23.57322167415998138, -14.73624932338542060, 3.997250019000003540 ) ) ;
#28881 = CARTESIAN_POINT ( 'NONE',  ( 23.56533302370000271, -14.74861233630000079, 224.4930104139999969 ) ) ;
#28882 = AXIS2_PLACEMENT_3D ( 'NONE', #22385, #10884, #24897 ) ;
#28883 = UNCERTAINTY_MEASURE_WITH_UNIT (LENGTH_MEASURE( 1.000000000000000082E-05 ), #14838, 'distance_accuracy_value', 'NONE');
#28884 = FACE_OUTER_BOUND ( 'NONE', #25504, .T. ) ;
#28885 = CARTESIAN_POINT ( 'NONE',  ( -17.44828348017237829, -22.00029153676899440, -29.28989589971321195 ) ) ;
#28886 = EDGE_LOOP ( 'NONE', ( #16168, #18838, #29247, #26369, #28411, #16939 ) ) ;
#28887 = CARTESIAN_POINT ( 'NONE',  ( 24.32472724076343695, -13.45989056521276872, 6.099998581000020792 ) ) ;
#28888 = CARTESIAN_POINT ( 'NONE',  ( 23.62009186283282958, -12.66256056296848342, 224.2880739211889249 ) ) ;
#28889 = CARTESIAN_POINT ( 'NONE',  ( 10.35667741062603397, -26.55163333981976592, 90.00000000000000000 ) ) ;
#28890 = CARTESIAN_POINT ( 'NONE',  ( -7.999999999786640892, -67.40749995144636841, -17.04319545400304392 ) ) ;
#28891 = CARTESIAN_POINT ( 'NONE',  ( 0.000000000000000000, 0.000000000000000000, 90.00000000000000000 ) ) ;
#28892 = DIRECTION ( 'NONE',  ( -1.000000000000000000, 0.000000000000000000, 0.000000000000000000 ) ) ;
#28893 = CARTESIAN_POINT ( 'NONE',  ( 3.326860148959999819, 4.874695247160000022, 226.6412452697800006 ) ) ;
#28894 = ADVANCED_FACE ( 'NONE', ( #16732 ), #19595, .T. ) ;
#28895 = CARTESIAN_POINT ( 'NONE',  ( -0.9876156946363959799, -26.78228253927133196, 225.4913731638064576 ) ) ;
#28896 = VECTOR ( 'NONE', #7516, 1000.000000000000000 ) ;
#28897 = CYLINDRICAL_SURFACE ( 'NONE', #10750, 1.100000000000002309 ) ;
#28898 = CARTESIAN_POINT ( 'NONE',  ( 1.087346358790000053E-15, 2.000000000000000000, 227.6412452699999847 ) ) ;
#28899 = ADVANCED_FACE ( 'NONE', ( #12793 ), #26499, .T. ) ;
#28900 = CARTESIAN_POINT ( 'NONE',  ( 9.777910293735976310, 7.131609509313695305, 232.0000002394077683 ) ) ;
#28901 = CARTESIAN_POINT ( 'NONE',  ( 23.23277120357798964, 15.26692725135965745, 4.999998581000003384 ) ) ;
#28902 = FACE_OUTER_BOUND ( 'NONE', #17078, .T. ) ;
#28903 = AXIS2_PLACEMENT_3D ( 'NONE', #666, #24260, #15126 ) ;
#28904 = EDGE_CURVE ( 'NONE', #20192, #14021, #21941, .T. ) ;
#28905 = CARTESIAN_POINT ( 'NONE',  ( 7.259803861751887410, 3.808917229486211031, -42.67470805251851829 ) ) ;
#28906 = CARTESIAN_POINT ( 'NONE',  ( -24.12724309970000292, -13.81083407110000039, 223.9040321390000088 ) ) ;
#28907 = ORIENTED_EDGE ( 'NONE', *, *, #18279, .T. ) ;
#28908 = CARTESIAN_POINT ( 'NONE',  ( 24.53709010086652142, -14.49830767851621793, 223.9262482216262242 ) ) ;
#28909 = CARTESIAN_POINT ( 'NONE',  ( -4.240613917342963113, -1.711409762446096439, -59.38491726642499202 ) ) ;
#28910 = ORIENTED_EDGE ( 'NONE', *, *, #7747, .F. ) ;
#28911 = B_SPLINE_CURVE_WITH_KNOTS ( 'NONE', 5,
 ( #10261, #19864, #18960, #21172, #14096, #14677, #29134, #16595, #23699 ),
 .UNSPECIFIED., .F., .F.,
 ( 6, 3, 6 ),
 ( 46.94504270979999916, 50.80649256949999426, 53.82812367380000040 ),
 .UNSPECIFIED. ) ;
#28912 = CONTEXT_DEPENDENT_SHAPE_REPRESENTATION ( #29871, #26308 ) ;
#28913 = ORIENTED_EDGE ( 'NONE', *, *, #23303, .F. ) ;
#28914 = DIRECTION ( 'NONE',  ( -0.3633921898465292122, -0.9316362575375349842, 0.000000000000000000 ) ) ;
#28915 = ORIENTED_EDGE ( 'NONE', *, *, #13726, .F. ) ;
#28916 = AXIS2_PLACEMENT_3D ( 'NONE', #2219, #14487, #5033 ) ;
#28917 = CYLINDRICAL_SURFACE ( 'NONE', #23235, 4.099999999999997868 ) ;
#28918 = CARTESIAN_POINT ( 'NONE',  ( -24.37165444408190851, 14.77472139917419369, 4.895781291000017355 ) ) ;
#28919 = SURFACE_STYLE_FILL_AREA ( #3917 ) ;
#28920 = B_SPLINE_CURVE_WITH_KNOTS ( 'NONE', 3,
 ( #30822, #1875, #25323, #21076, #28148, #16032 ),
 .UNSPECIFIED., .F., .F.,
 ( 4, 2, 4 ),
 ( 0.000000000000000000, 0.5000000000000000000, 1.000000000000000000 ),
 .UNSPECIFIED. ) ;
#28921 = CARTESIAN_POINT ( 'NONE',  ( 3.974243191089999350, 11.57455430929999984, 232.6627648150000027 ) ) ;
#28922 = CARTESIAN_POINT ( 'NONE',  ( 10.00000000000000000, -13.30122639390952877, -75.84793558053411289 ) ) ;
#28923 = CARTESIAN_POINT ( 'NONE',  ( -4.273751495587445604, 4.364932658710685587, -3.968732180600002657 ) ) ;
#28924 = FACE_OUTER_BOUND ( 'NONE', #13854, .T. ) ;
#28925 = ORIENTED_EDGE ( 'NONE', *, *, #18281, .T. ) ;
#28926 = CYLINDRICAL_SURFACE ( 'NONE', #9984, 1.100000000000002309 ) ;
#28927 = CARTESIAN_POINT ( 'NONE',  ( -4.663991843195165465, -3.413757688390889555, -19.47254627020000939 ) ) ;
#28928 = CARTESIAN_POINT ( 'NONE',  ( 0.9163752123637586289, 3.499999999999999556, 230.7685035973587446 ) ) ;
#28929 = CARTESIAN_POINT ( 'NONE',  ( -8.699999999696727215, -25.22421763345087342, -30.84970730147981754 ) ) ;
#28930 = EDGE_CURVE ( 'NONE', #20670, #22879, #30073, .T. ) ;
#28931 = CARTESIAN_POINT ( 'NONE',  ( -5.871915332739999549, 10.61013173299999934, 230.6412452697800006 ) ) ;
#28932 = DIRECTION ( 'NONE',  ( 0.000000000000000000, 1.000000000000000000, 0.000000000000000000 ) ) ;
#28933 = ADVANCED_FACE ( 'NONE', ( #14862 ), #24914, .F. ) ;
#28934 = B_SPLINE_CURVE_WITH_KNOTS ( 'NONE', 3,
 ( #1550, #30959, #14596, #7350, #7190, #5299 ),
 .UNSPECIFIED., .F., .F.,
 ( 4, 2, 4 ),
 ( 0.000000000000000000, 0.5000000000000000000, 1.000000000000000000 ),
 .UNSPECIFIED. ) ;
#28935 = CARTESIAN_POINT ( 'NONE',  ( 4.259937771191533606, -20.47891468366403345, -30.82874092286507306 ) ) ;
#28936 = EDGE_CURVE ( 'NONE', #1204, #5832, #27779, .T. ) ;
#28937 = CARTESIAN_POINT ( 'NONE',  ( 1.018916989216064772, -26.78112380533112358, 224.5794179396494883 ) ) ;
#28938 = CARTESIAN_POINT ( 'NONE',  ( -24.97472003774791816, -13.73006752753317450, 5.208359076000035337 ) ) ;
#28939 = EDGE_CURVE ( 'NONE', #979, #13384, #6046, .T. ) ;
#28940 = CARTESIAN_POINT ( 'NONE',  ( 8.999999999770000869, 21.70000000000000284, -45.10000000000000142 ) ) ;
#28941 = ORIENTED_EDGE ( 'NONE', *, *, #458, .F. ) ;
#28942 = CARTESIAN_POINT ( 'NONE',  ( 2.749945525234485988, 3.922844750473964748, -30.14856724380000230 ) ) ;
#28943 = B_SPLINE_CURVE_WITH_KNOTS ( 'NONE', 3,
 ( #13238, #10584, #17801, #3032, #12625, #8053, #22854, #15148, #3184, #694, #5850, #12787 ),
 .UNSPECIFIED., .F., .F.,
 ( 4, 2, 2, 2, 2, 4 ),
 ( 0.000000000000000000, 0.2499999999999988343, 0.3749999999999989453, 0.4999999999999991118, 0.7499999999999995559, 1.000000000000000000 ),
 .UNSPECIFIED. ) ;
#28944 = DIRECTION ( 'NONE',  ( 5.962915006522623408E-16, 0.4383711467890811231, 0.8987940462991652613 ) ) ;
#28945 = VERTEX_POINT ( 'NONE', #25538 ) ;
#28946 = CARTESIAN_POINT ( 'NONE',  ( 25.35851007746311581, -13.00862288856444238, 4.319165765000021473 ) ) ;
#28947 = CARTESIAN_POINT ( 'NONE',  ( 1.970249664213433727, 5.584433078155761621, -46.29079303332500217 ) ) ;
#28948 = EDGE_LOOP ( 'NONE', ( #21450, #26160, #3163, #26273, #6824, #27697, #15206, #19936, #6299, #4764, #11845, #15665 ) ) ;
#28949 = ORIENTED_EDGE ( 'NONE', *, *, #21707, .T. ) ;
#28950 = CARTESIAN_POINT ( 'NONE',  ( 0.000000000000000000, 0.000000000000000000, 0.000000000000000000 ) ) ;
#28951 = ORIENTED_EDGE ( 'NONE', *, *, #12886, .F. ) ;
#28952 = CARTESIAN_POINT ( 'NONE',  ( -0.4820778521899999891, -28.49640832880000119, 223.9974845609999932 ) ) ;
#28953 = VERTEX_POINT ( 'NONE', #29629 ) ;
#28954 = CARTESIAN_POINT ( 'NONE',  ( -24.49999999470000134, 3.000285566209999917E-15, 90.00000000069999828 ) ) ;
#28955 = CARTESIAN_POINT ( 'NONE',  ( 2.020725942159999899, 3.500000000000000000, 227.9588918784999976 ) ) ;
#28956 = CARTESIAN_POINT ( 'NONE',  ( 10.00000000070000183, -30.00000000000000000, -28.40000000000000213 ) ) ;
#28957 = CARTESIAN_POINT ( 'NONE',  ( 0.6023992814822636266, 4.702695962538667729, -35.70000000000000284 ) ) ;
#28958 = CARTESIAN_POINT ( 'NONE',  ( 20.30396079652883756, 20.00000000004620304, 1.000000000000000888 ) ) ;
#28959 = CARTESIAN_POINT ( 'NONE',  ( -24.27467683362817397, 13.55001165674122987, 6.095967889000020179 ) ) ;
#28960 = CARTESIAN_POINT ( 'NONE',  ( -10.99999999969999998, 20.99999999999999645, -70.09999999999999432 ) ) ;
#28961 = CARTESIAN_POINT ( 'NONE',  ( -27.50000000000000000, 3.367667473009999970E-15, 43.28090191839999790 ) ) ;
#28962 = EDGE_CURVE ( 'NONE', #29947, #17135, #18422, .T. ) ;
#28963 = ORIENTED_EDGE ( 'NONE', *, *, #28748, .T. ) ;
#28964 = CARTESIAN_POINT ( 'NONE',  ( 5.967946066639521874, -1.056419632483374116, -8.771482634700005221 ) ) ;
#28965 = CARTESIAN_POINT ( 'NONE',  ( 3.499930668453409055, 4.992711500635231836, -29.21106724380000230 ) ) ;
#28966 = DIRECTION ( 'NONE',  ( -0.6343890248118320141, -0.7730139489027949562, 0.000000000000000000 ) ) ;
#28967 = CARTESIAN_POINT ( 'NONE',  ( 23.83006841374216833, -14.31758446293960141, 5.507121129000008608 ) ) ;
#28968 = CARTESIAN_POINT ( 'NONE',  ( 19.36636234657989775, 19.99999973364792538, -0.3591601440000036227 ) ) ;
#28969 = CARTESIAN_POINT ( 'NONE',  ( 13.00000000000000000, 24.54213077165692525, -59.94572446259928711 ) ) ;
#28970 = CARTESIAN_POINT ( 'NONE',  ( 2.193015549840575229, -20.47026972997080563, -27.49515152708232790 ) ) ;
#28971 = CARTESIAN_POINT ( 'NONE',  ( -3.941349475653395551, -1.876729865818549392, -12.97655742010000246 ) ) ;
#28972 = B_SPLINE_CURVE_WITH_KNOTS ( 'NONE', 5,
 ( #10611, #22425, #17379, #27288, #25088, #7626 ),
 .UNSPECIFIED., .F., .F.,
 ( 6, 6 ),
 ( 0.000000000000000000, 2.300779637260000232 ),
 .UNSPECIFIED. ) ;
#28973 = B_SPLINE_CURVE_WITH_KNOTS ( 'NONE', 3,
 ( #18824, #23571, #31100, #19140, #25922, #6555 ),
 .UNSPECIFIED., .F., .F.,
 ( 4, 2, 4 ),
 ( 0.000000000000000000, 0.5000000000000000000, 1.000000000000000000 ),
 .UNSPECIFIED. ) ;
#28974 = CARTESIAN_POINT ( 'NONE',  ( 24.07552309629999954, -13.90001137839999856, 223.9000014189999774 ) ) ;
#28975 = DIRECTION ( 'NONE',  ( 0.2815395311429195746, 0.9595496299847261490, 0.000000000000000000 ) ) ;
#28976 = CARTESIAN_POINT ( 'NONE',  ( -0.9813161448490499428, -3.499840617129381659, 230.7583807310667225 ) ) ;
#28977 = ORIENTED_EDGE ( 'NONE', *, *, #6124, .F. ) ;
#28978 = CARTESIAN_POINT ( 'NONE',  ( 18.03540948973492775, -8.309720466357155999, -0.6999999999999784173 ) ) ;
#28979 = CARTESIAN_POINT ( 'NONE',  ( -12.75378086759999796, -32.00000000000000000, -31.28675134614999820 ) ) ;
#28980 = EDGE_LOOP ( 'NONE', ( #17573, #24991, #14373, #25755 ) ) ;
#28981 = CARTESIAN_POINT ( 'NONE',  ( 24.69936741169999905, -14.21947533890000059, 226.1000014189999945 ) ) ;
#28982 = CARTESIAN_POINT ( 'NONE',  ( 13.67718073920000066, 21.70000000000000284, -57.16242423349999768 ) ) ;
#28983 = VERTEX_POINT ( 'NONE', #27417 ) ;
#28984 = ORIENTED_EDGE ( 'NONE', *, *, #28720, .F. ) ;
#28985 = ORIENTED_EDGE ( 'NONE', *, *, #14412, .F. ) ;
#28986 = ORIENTED_EDGE ( 'NONE', *, *, #18113, .T. ) ;
#28987 = CARTESIAN_POINT ( 'NONE',  ( -10.88910015670000142, 21.70000000000000284, -56.10000000020000499 ) ) ;
#28988 = CARTESIAN_POINT ( 'NONE',  ( -21.16705332929999983, 21.30254446269999846, 222.0000000000000000 ) ) ;
#28989 = EDGE_CURVE ( 'NONE', #18765, #9238, #4198, .T. ) ;
#28990 = DIRECTION ( 'NONE',  ( 0.000000000000000000, -0.9128796883888949942, 0.4082287037029534438 ) ) ;
#28991 = ORIENTED_EDGE ( 'NONE', *, *, #9065, .F. ) ;
#28992 = DIRECTION ( 'NONE',  ( 1.000000000000000000, -6.668066630619518976E-24, -2.257150022442225012E-12 ) ) ;
#28993 = CARTESIAN_POINT ( 'NONE',  ( 10.69999999989999928, -25.00000000000000000, -7.274962170899998526 ) ) ;
#28994 = CARTESIAN_POINT ( 'NONE',  ( -17.38167868481496114, -31.99978167043220623, -29.80148372884886498 ) ) ;
#28995 = DIRECTION ( 'NONE',  ( 0.000000000000000000, -1.000000000000000000, 0.000000000000000000 ) ) ;
#28996 = ORIENTED_EDGE ( 'NONE', *, *, #29785, .T. ) ;
#28997 = ADVANCED_FACE ( 'NONE', ( #8999 ), #26622, .T. ) ;
#28998 = CARTESIAN_POINT ( 'NONE',  ( -21.17688367750145773, 18.05241592653123206, 5.000000064000004407 ) ) ;
#28999 = AXIS2_PLACEMENT_3D ( 'NONE', #14413, #5109, #3055 ) ;
#29000 = CARTESIAN_POINT ( 'NONE',  ( 3.256742448429973624, 4.730705660258329281, -16.61259163650000303 ) ) ;
#29001 = CARTESIAN_POINT ( 'NONE',  ( 28.50000000000000000, 8.881784197000000993E-16, 222.0000000000000000 ) ) ;
#29002 = CIRCLE ( 'NONE', #19460, 3.491271820589999741 ) ;
#29003 = CARTESIAN_POINT ( 'NONE',  ( -27.92857142909999979, 3.420150602519999655E-15, 142.0603150149999863 ) ) ;
#29004 = CARTESIAN_POINT ( 'NONE',  ( -1.484924240490000047, 1.484924240490000047, 227.6412452697800006 ) ) ;
#29005 = CARTESIAN_POINT ( 'NONE',  ( 24.61862080450000079, 14.40921680009999939, 222.0000000000000000 ) ) ;
#29006 = CARTESIAN_POINT ( 'NONE',  ( -24.39492853991606225, 13.33306305658284430, 3.899998581000068132 ) ) ;
#29007 = DIRECTION ( 'NONE',  ( 5.962915006522622422E-16, 0.4383711467890810676, 0.8987940462991651502 ) ) ;
#29008 = LINE ( 'NONE', #2886, #10204 ) ;
#29009 = CARTESIAN_POINT ( 'NONE',  ( 21.55746468670000127, 17.28477200280000048, 229.9172016159999998 ) ) ;
#29010 = CARTESIAN_POINT ( 'NONE',  ( -18.35450744919999977, 0.3144422474040000082, 230.6999999999999886 ) ) ;
#29011 = ORIENTED_EDGE ( 'NONE', *, *, #21350, .F. ) ;
#29012 = CARTESIAN_POINT ( 'NONE',  ( -2.825020644939634007, -4.425443225455641283, -0.6999999999999992895 ) ) ;
#29013 = VECTOR ( 'NONE', #20593, 1000.000000000000000 ) ;
#29014 = CARTESIAN_POINT ( 'NONE',  ( -26.93696268452645981, -0.4901285798021789986, 0.000000000000000000 ) ) ;
#29015 = CARTESIAN_POINT ( 'NONE',  ( -4.834657140208623360, 0.1770554249713849337, -68.10000000002501963 ) ) ;
#29016 = ADVANCED_FACE ( 'NONE', ( #6638 ), #15240, .T. ) ;
#29017 = ORIENTED_EDGE ( 'NONE', *, *, #107, .F. ) ;
#29018 = AXIS2_PLACEMENT_3D ( 'NONE', #11506, #13551, #13870 ) ;
#29019 = DIRECTION ( 'NONE',  ( 0.000000000000000000, 0.000000000000000000, -1.000000000000000000 ) ) ;
#29020 = AXIS2_PLACEMENT_3D ( 'NONE', #4388, #11624, #13357 ) ;
#29021 = ORIENTED_EDGE ( 'NONE', *, *, #26296, .F. ) ;
#29022 = CARTESIAN_POINT ( 'NONE',  ( -11.08586295458008486, 19.99999999999999645, -1.599967101673252401 ) ) ;
#29023 = CARTESIAN_POINT ( 'NONE',  ( 0.8794532062878365197, -27.78659480101269708, 3.957673652000032405 ) ) ;
#29024 = ORIENTED_EDGE ( 'NONE', *, *, #70, .F. ) ;
#29025 = CARTESIAN_POINT ( 'NONE',  ( 3.104103280670445830, -4.533555713950848443, -28.13292313650000409 ) ) ;
#29026 = CARTESIAN_POINT ( 'NONE',  ( 8.903108651239925564, -22.82508830966962421, 90.00000000000000000 ) ) ;
#29027 = CARTESIAN_POINT ( 'NONE',  ( -4.185672079393978784, 2.483218523716627768, -50.83267869292499341 ) ) ;
#29028 = CARTESIAN_POINT ( 'NONE',  ( 8.700000000241349341, -24.55027189127212850, -26.62408091262140530 ) ) ;
#29029 = DIRECTION ( 'NONE',  ( 1.000000000000000000, 0.000000000000000000, 0.000000000000000000 ) ) ;
#29030 = B_SPLINE_SURFACE_WITH_KNOTS ( 'NONE', 5, 1, ( 
 ( #17467, #18076 ),
 ( #15116, #4088 ),
 ( #20764, #9110 ),
 ( #16197, #11169 ),
 ( #18710, #1581 ),
 ( #23610, #20606 ),
 ( #3934, #30372 ),
 ( #21235, #18232 ),
 ( #15891, #8800 ),
 ( #27841, #11016 ),
 ( #6598, #18402 ),
 ( #13527, #15721 ),
 ( #1885, #25811 ),
 ( #8959, #30834 ),
 ( #16046, #27999 ),
 ( #20927, #30529 ),
 ( #23139, #1422 ),
 ( #21087, #6443 ),
 ( #30204, #4246 ),
 ( #8636, #25658 ),
 ( #2046, #28309 ),
 ( #23289, #13367 ),
 ( #25335, #6292 ),
 ( #1734, #13686 ),
 ( #25962, #13845 ),
 ( #11330, #18558 ),
 ( #28159, #11636 ) ),
 .UNSPECIFIED., .F., .F., .F.,
 ( 6, 3, 3, 3, 3, 3, 3, 3, 6 ),
 ( 2, 2 ),
 ( 0.000000000000000000, 12.04914910469999967, 24.12830621100000172, 36.22018076730000047, 48.28758829720000278, 60.33208762030000116, 72.38455155859999479, 84.43687076610000020, 88.75867308210000317 ),
 ( -2.393070191420000080E-05, 0.7036780443879999680 ),
 .UNSPECIFIED. ) ;
#29031 = EDGE_CURVE ( 'NONE', #13864, #7590, #22794, .T. ) ;
#29032 = CARTESIAN_POINT ( 'NONE',  ( -7.999999999643747195, -11.71436167353443736, -38.59800651357252121 ) ) ;
#29033 = TOROIDAL_SURFACE ( 'NONE', #17486, 24.50000000000000000, 3.200000000000000178 ) ;
#29034 = CARTESIAN_POINT ( 'NONE',  ( 3.503013490861627499, 0.9326026542233571970, 230.7640337244206421 ) ) ;
#29035 = VECTOR ( 'NONE', #26820, 1000.000000000000000 ) ;
#29036 = CARTESIAN_POINT ( 'NONE',  ( -17.40556230546145500, -22.00020956758401525, -29.63986184916237221 ) ) ;
#29037 = ORIENTED_EDGE ( 'NONE', *, *, #10251, .T. ) ;
#29038 = CARTESIAN_POINT ( 'NONE',  ( 10.00000000070000183, 19.99999999999999645, -42.39999999999999858 ) ) ;
#29039 = CARTESIAN_POINT ( 'NONE',  ( -24.22405393111669980, -13.63981656684929078, 5.760125276000005456 ) ) ;
#29040 = CARTESIAN_POINT ( 'NONE',  ( -6.530148857409999508, -10.14823162649999944, 231.9999989789999972 ) ) ;
#29041 = FACE_OUTER_BOUND ( 'NONE', #18630, .T. ) ;
#29042 = CARTESIAN_POINT ( 'NONE',  ( -12.09920997781542873, 0.2766207017873786866, 232.0000000000048033 ) ) ;
#29043 = CARTESIAN_POINT ( 'NONE',  ( -8.699999999725333666, -24.55029269852046170, -26.62421763350704040 ) ) ;
#29044 = DIRECTION ( 'NONE',  ( 0.000000000000000000, 0.8660254037843289066, -0.5000000000001899592 ) ) ;
#29045 = AXIS2_PLACEMENT_3D ( 'NONE', #19729, #9507, #16729 ) ;
#29046 = CARTESIAN_POINT ( 'NONE',  ( -20.77600556902951823, -21.68409854416798410, 0.7595836940000044724 ) ) ;
#29047 = CARTESIAN_POINT ( 'NONE',  ( 0.5621952752015302313, -27.49459032396439540, 4.043049797261333289 ) ) ;
#29048 = ADVANCED_FACE ( 'NONE', ( #28353, #28509 ), #20965, .T. ) ;
#29049 = CARTESIAN_POINT ( 'NONE',  ( -4.785279987099964494, -31.71089578132184883, 8.000000000000007105 ) ) ;
#29050 = CARTESIAN_POINT ( 'NONE',  ( 1.007237960741796279, -1.747572776708517406, 227.6412452703083886 ) ) ;
#29051 = EDGE_CURVE ( 'NONE', #8590, #9948, #6779, .T. ) ;
#29052 = CARTESIAN_POINT ( 'NONE',  ( -24.34663841809999951, -12.78636765230000094, 5.000000000000000000 ) ) ;
#29053 = DIRECTION ( 'NONE',  ( -3.134067079931429195E-12, -0.3568421334038983650, 0.9341647027306021478 ) ) ;
#29054 = CARTESIAN_POINT ( 'NONE',  ( 7.195957064175671825, -115.1234601580806611, 21.94894157346885066 ) ) ;
#29055 = VERTEX_POINT ( 'NONE', #23497 ) ;
#29056 = VECTOR ( 'NONE', #8585, 1000.000000000000000 ) ;
#29057 = CARTESIAN_POINT ( 'NONE',  ( 6.760007715859396527, 4.357143524031256376, -42.94209588227683128 ) ) ;
#29058 = ADVANCED_FACE ( 'NONE', ( #16396 ), #21790, .T. ) ;
#29059 = ORIENTED_EDGE ( 'NONE', *, *, #10079, .F. ) ;
#29060 = CARTESIAN_POINT ( 'NONE',  ( 24.80399018339999628, -14.03663607480000053, 226.0798554400000171 ) ) ;
#29061 = CARTESIAN_POINT ( 'NONE',  ( 5.975646968830259809, -0.1056191442178888718, -58.09793411332499602 ) ) ;
#29062 = VERTEX_POINT ( 'NONE', #11524 ) ;
#29063 = VERTEX_POINT ( 'NONE', #26312 ) ;
#29066 = EDGE_CURVE ( 'NONE', #27949, #10599, #4758, .T. ) ;
#29065 = CARTESIAN_POINT ( 'NONE',  ( -18.00000000000000000, 2.204291436879999808E-15, 230.6412452697800006 ) ) ;
#29064 = VECTOR ( 'NONE', #7520, 1000.000000000000000 ) ;
#29067 = ORIENTED_EDGE ( 'NONE', *, *, #9079, .F. ) ;
#29068 = ORIENTED_EDGE ( 'NONE', *, *, #18911, .T. ) ;
#29069 = CARTESIAN_POINT ( 'NONE',  ( -24.52721838136531574, 14.51532614515681097, 4.239732039000021047 ) ) ;
#29070 = CARTESIAN_POINT ( 'NONE',  ( 9.993285220779439371, -25.61999708228226069, 86.39444872449999480 ) ) ;
#29071 = CARTESIAN_POINT ( 'NONE',  ( -19.80535357377644701, 19.50875577052588739, 1.400000021000019634 ) ) ;
#29072 = CARTESIAN_POINT ( 'NONE',  ( 1.348918213770420316, 4.124136235849971577, -10.57047964830000275 ) ) ;
#29073 = DIRECTION ( 'NONE',  ( 1.000000000000000000, 0.000000000000000000, -0.000000000000000000 ) ) ;
#29074 = ORIENTED_EDGE ( 'NONE', *, *, #24442, .F. ) ;
#29075 = DIRECTION ( 'NONE',  ( -0.7198537139083028835, 0.6941258031311204890, 0.000000000000000000 ) ) ;
#29076 = CARTESIAN_POINT ( 'NONE',  ( -24.61381496313306982, -14.36755986783020056, 3.957524336000023624 ) ) ;
#29077 = ADVANCED_FACE ( 'NONE', ( #20811 ), #21862, .T. ) ;
#29078 = AXIS2_PLACEMENT_3D ( 'NONE', #8754, #6858, #23412 ) ;
#29079 = CARTESIAN_POINT ( 'NONE',  ( 2.992916622598568388, -2.824380467281232487, -18.03565260999999964 ) ) ;
#29080 = CARTESIAN_POINT ( 'NONE',  ( 0.7993620172799370538, 3.499999999999998668, 230.7846409045036751 ) ) ;
#29081 = CARTESIAN_POINT ( 'NONE',  ( 0.9950318228358414618, -27.48257863589062922, 225.4905541412982757 ) ) ;
#29082 = B_SPLINE_CURVE_WITH_KNOTS ( 'NONE', 3,
 ( #7425, #26624, #14675, #24261, #2706, #4456 ),
 .UNSPECIFIED., .F., .F.,
 ( 4, 2, 4 ),
 ( 0.000000000000000000, 0.5000000000000000000, 1.000000000000000000 ),
 .UNSPECIFIED. ) ;
#29083 = CARTESIAN_POINT ( 'NONE',  ( 8.000000000050000892, -13.30122639390952877, -75.84793558053411289 ) ) ;
#29084 = DIRECTION ( 'NONE',  ( 0.9316362575375356503, 0.3633921898465274913, 0.000000000000000000 ) ) ;
#29085 = CARTESIAN_POINT ( 'NONE',  ( 0.5498575204270217398, -4.501552459765377101, -43.78057807742499818 ) ) ;
#29086 = B_SPLINE_CURVE_WITH_KNOTS ( 'NONE', 5,
 ( #24484, #15185, #27299, #26995, #29188, #9852, #5434, #17684, #24943, #5585, #7489, #29504, #19918, #27150, #24635 ),
 .UNSPECIFIED., .F., .F.,
 ( 6, 3, 3, 3, 6 ),
 ( 0.000000000000000000, 0.1000000000011452422, 0.4000000000045809689, 0.7000000000005726086, 1.000000000000000000 ),
 .UNSPECIFIED. ) ;
#29087 = CARTESIAN_POINT ( 'NONE',  ( -7.999999999982724042, -116.6191538659648188, 10.70265178694466002 ) ) ;
#29088 = DIRECTION ( 'NONE',  ( 0.000000000000000000, 0.000000000000000000, -1.000000000000000000 ) ) ;
#29089 = FACE_BOUND ( 'NONE', #9726, .T. ) ;
#29090 = CARTESIAN_POINT ( 'NONE',  ( -21.99953312590000110, 17.62920693369999725, 229.0000000010000178 ) ) ;
#29091 = DIRECTION ( 'NONE',  ( -0.9880370573969196046, 0.1542166437529880751, 0.000000000000000000 ) ) ;
#29092 = EDGE_LOOP ( 'NONE', ( #4531, #11387, #20354, #20127, #22488, #4323, #28373 ) ) ;
#29093 = CARTESIAN_POINT ( 'NONE',  ( -2.923929784071483073, -5.123485640109426420, -31.67642233980000555 ) ) ;
#29094 = ORIENTED_EDGE ( 'NONE', *, *, #6339, .F. ) ;
#29095 = CARTESIAN_POINT ( 'NONE',  ( -10.00000000057676530, -41.43235263067919760, -26.99482620585297710 ) ) ;
#29096 = CARTESIAN_POINT ( 'NONE',  ( 4.647199600633202365, 1.656603404052558348, -46.67627377572500791 ) ) ;
#29097 = ORIENTED_EDGE ( 'NONE', *, *, #15087, .F. ) ;
#29098 = VERTEX_POINT ( 'NONE', #24251 ) ;
#29099 = AXIS2_PLACEMENT_3D ( 'NONE', #9653, #14544, #26343 ) ;
#29100 = CARTESIAN_POINT ( 'NONE',  ( 22.29837091775305424, -18.13432743042971751, 244.8619695981046505 ) ) ;
#29101 = VERTEX_POINT ( 'NONE', #24570 ) ;
#29102 = CARTESIAN_POINT ( 'NONE',  ( -0.8057362888000000334, -27.78873281839999976, 224.2403608809999866 ) ) ;
#29103 = EDGE_CURVE ( 'NONE', #24186, #30146, #5365, .T. ) ;
#29104 = ORIENTED_EDGE ( 'NONE', *, *, #7045, .F. ) ;
#29105 = CARTESIAN_POINT ( 'NONE',  ( 27.79539923781684507, 0.5057481689249130330, 1.000000000000000888 ) ) ;
#29106 = LINE ( 'NONE', #7398, #9430 ) ;
#29107 = CARTESIAN_POINT ( 'NONE',  ( 1.325687545906950593, 4.708841374623678355, -35.69999999999998153 ) ) ;
#29108 = EDGE_CURVE ( 'NONE', #21516, #7813, #10095, .T. ) ;
#29109 = CIRCLE ( 'NONE', #16039, 1.100000000390000787 ) ;
#29110 = EDGE_CURVE ( 'NONE', #5828, #25188, #357, .T. ) ;
#29111 = CARTESIAN_POINT ( 'NONE',  ( -22.41257468390000085, 16.47776880720000037, 223.0000000000000000 ) ) ;
#29112 = CARTESIAN_POINT ( 'NONE',  ( -24.49145440957854802, 14.57548795260905550, 5.680829343999993952 ) ) ;
#29113 = CARTESIAN_POINT ( 'NONE',  ( -133283.2115610000037, -454258.9661130000022, -160669.8390839999774 ) ) ;
#29114 = DIRECTION ( 'NONE',  ( 5.962915006522623408E-16, 0.4383711467890811231, 0.8987940462991652613 ) ) ;
#29115 = VERTEX_POINT ( 'NONE', #14972 ) ;
#29116 = CARTESIAN_POINT ( 'NONE',  ( 4.416054526660082580, -3.250752328011468961, -9.972776792900004850 ) ) ;
#29117 = CARTESIAN_POINT ( 'NONE',  ( -3.866422574246632937, 4.445403037619903408, -27.58728588870000209 ) ) ;
#29118 = CARTESIAN_POINT ( 'NONE',  ( 27.92857142909999979, -3.420150602509999660E-15, 87.93968498519998889 ) ) ;
#29119 = CARTESIAN_POINT ( 'NONE',  ( 24.52721838744800920, -14.51532614964689394, 5.760265122000007842 ) ) ;
#29120 = CARTESIAN_POINT ( 'NONE',  ( 23.94167923218613225, 14.12976891125826029, 6.079852602000002548 ) ) ;
#29121 = CARTESIAN_POINT ( 'NONE',  ( 2.107992564109750333, -27.41908764619381245, 20.00000000000000355 ) ) ;
#29122 = CARTESIAN_POINT ( 'NONE',  ( -2.929853409778804263, 3.622264489389750874, -13.60352819869999763 ) ) ;
#29123 = CARTESIAN_POINT ( 'NONE',  ( 1.311146135488785669, -27.76947565999227763, 5.759639119000015128 ) ) ;
#29124 = CARTESIAN_POINT ( 'NONE',  ( 14.40197535836999876, -27.00000000000014566, -22.62649730800000114 ) ) ;
#29125 = PLANE ( 'NONE',  #13283 ) ;
#29126 = VERTEX_POINT ( 'NONE', #660 ) ;
#29127 = DIRECTION ( 'NONE',  ( -1.000000000000000000, 5.665498452320000818E-16, 0.000000000000000000 ) ) ;
#29128 = CARTESIAN_POINT ( 'NONE',  ( -12.57202792198531682, -32.00000000000000000, -30.61316950642639867 ) ) ;
#29129 = CIRCLE ( 'NONE', #23627, 4.999999999999998224 ) ;
#29130 = EDGE_LOOP ( 'NONE', ( #1219, #8110, #27453, #12900, #3118, #15905 ) ) ;
#29131 = CARTESIAN_POINT ( 'NONE',  ( 1.280497938707983563, 1.670464374140186781, 226.6412452697800006 ) ) ;
#29132 = FACE_OUTER_BOUND ( 'NONE', #18965, .T. ) ;
#29133 = VERTEX_POINT ( 'NONE', #2698 ) ;
#29134 = CARTESIAN_POINT ( 'NONE',  ( 4.198625184269999977, 11.29386254379999954, 230.6412452697800006 ) ) ;
#29135 = EDGE_LOOP ( 'NONE', ( #6106, #6360, #30475, #11665 ) ) ;
#29136 = ORIENTED_EDGE ( 'NONE', *, *, #21926, .F. ) ;
#29137 = FILL_AREA_STYLE_COLOUR ( '', #19855 ) ;
#29138 = VERTEX_POINT ( 'NONE', #29432 ) ;
#29139 = FACE_OUTER_BOUND ( 'NONE', #26008, .T. ) ;
#29140 = CARTESIAN_POINT ( 'NONE',  ( -16.29518228970498583, 11.96970539749145068, -0.6999999999999785283 ) ) ;
#29141 = CARTESIAN_POINT ( 'NONE',  ( 2.664535259099999805E-15, 2.694277338339796213, -67.89769279494430521 ) ) ;
#29142 = VERTEX_POINT ( 'NONE', #12598 ) ;
#29143 = CARTESIAN_POINT ( 'NONE',  ( -1.630907769230000026, -5.558498091359999727, 229.6412452697800006 ) ) ;
#29144 = CARTESIAN_POINT ( 'NONE',  ( -13.67718144140000014, 21.70000000000000284, -57.16242377749999548 ) ) ;
#29145 = EDGE_CURVE ( 'NONE', #1536, #12797, #13518, .T. ) ;
#29146 = CARTESIAN_POINT ( 'NONE',  ( -17.30352168679151248, -31.99964266802675894, -30.24496221943030250 ) ) ;
#29147 = CARTESIAN_POINT ( 'NONE',  ( 10.69999999992642614, -25.11956699865401532, -9.802329118429168986 ) ) ;
#29148 = EDGE_LOOP ( 'NONE', ( #11741, #12313, #21875, #1048 ) ) ;
#29149 = PRESENTATION_LAYER_ASSIGNMENT (  '', '', ( #9047 ) ) ;
#29150 = CARTESIAN_POINT ( 'NONE',  ( -13.00000000000000178, 24.78814172467860644, -59.85618379839584691 ) ) ;
#29151 = CARTESIAN_POINT ( 'NONE',  ( 1.270104287659547859, 5.038743611242932907, -16.05080441500000532 ) ) ;
#29152 = FACE_OUTER_BOUND ( 'NONE', #21251, .T. ) ;
#29153 = CARTESIAN_POINT ( 'NONE',  ( 7.638687372303289536, 6.462009008171509805, -40.63090155201393117 ) ) ;
#29154 = CARTESIAN_POINT ( 'NONE',  ( -10.69999999930000101, -29.06671945329999929, -26.22544931050000017 ) ) ;
#29155 = CARTESIAN_POINT ( 'NONE',  ( 24.01396915060000126, 14.05529641579999911, 222.0000000000000000 ) ) ;
#29156 = CARTESIAN_POINT ( 'NONE',  ( 22.68367506382111287, -14.27296989803571314, 5.420582065402280492 ) ) ;
#29157 = FACE_OUTER_BOUND ( 'NONE', #16631, .T. ) ;
#29158 = DIRECTION ( 'NONE',  ( 0.000000000000000000, 1.000000000000000000, 0.000000000000000000 ) ) ;
#29159 = CARTESIAN_POINT ( 'NONE',  ( -11.19633371010000111, -24.50869457490000158, -1.530575679400000944 ) ) ;
#29160 = CARTESIAN_POINT ( 'NONE',  ( -12.12499970569999874, 20.99999999999999645, -55.73512393480000071 ) ) ;
#29161 = ORIENTED_EDGE ( 'NONE', *, *, #8815, .F. ) ;
#29162 = CARTESIAN_POINT ( 'NONE',  ( 4.692739937119916327, 0.5303478879513032762, -54.61771407622499197 ) ) ;
#29163 = CARTESIAN_POINT ( 'NONE',  ( -12.40426553248159180, -25.63275973170342326, -23.41588860887158319 ) ) ;
#29164 = CARTESIAN_POINT ( 'NONE',  ( -26.79556473285982321, -0.4875557887251183442, -0.6999999999999784173 ) ) ;
#29165 = CARTESIAN_POINT ( 'NONE',  ( -3.691491291332746449, -3.512112988921174850, -68.10000000002500542 ) ) ;
#29166 = EDGE_LOOP ( 'NONE', ( #15337, #14372, #25687, #23814 ) ) ;
#29167 = ADVANCED_FACE ( 'NONE', ( #21742 ), #26815, .T. ) ;
#29168 = CARTESIAN_POINT ( 'NONE',  ( -2.874128808496339893, 2.180705937046730547, -91.64589571366730070 ) ) ;
#29169 = ORIENTED_EDGE ( 'NONE', *, *, #24218, .F. ) ;
#29170 = CARTESIAN_POINT ( 'NONE',  ( -11.56700259526638419, 19.99999999999999645, -1.400000000399997946 ) ) ;
#29171 = CARTESIAN_POINT ( 'NONE',  ( -1.084269253894827534, -5.810518403417324507, -68.38745670422500211 ) ) ;
#29172 = ORIENTED_EDGE ( 'NONE', *, *, #2374, .T. ) ;
#29173 = CARTESIAN_POINT ( 'NONE',  ( -3.834000099192958810, 2.652495916366497841, -25.96779765529999651 ) ) ;
#29174 = CARTESIAN_POINT ( 'NONE',  ( 1.630907769230000026, 5.558498091359999727, 227.6412452697800006 ) ) ;
#29175 = CARTESIAN_POINT ( 'NONE',  ( -2.393684743089937061, 3.904820337558664978, -45.05531229042499319 ) ) ;
#29176 = CARTESIAN_POINT ( 'NONE',  ( -24.13062658843018227, -13.18986347163402506, 4.086914725630220069 ) ) ;
#29177 = CARTESIAN_POINT ( 'NONE',  ( 0.5569265643388185971, -27.49469370723012673, 224.0404533956380249 ) ) ;
#29178 = CARTESIAN_POINT ( 'NONE',  ( -15.72433334783165293, 11.02535689765575455, -1.400000000000001910 ) ) ;
#29179 = UNCERTAINTY_MEASURE_WITH_UNIT (LENGTH_MEASURE( 1.000000000000000082E-05 ), #4494, 'distance_accuracy_value', 'NONE');
#29180 = B_SPLINE_CURVE_WITH_KNOTS ( 'NONE', 3,
 ( #24432, #207, #24269, #370 ),
 .UNSPECIFIED., .F., .F.,
 ( 4, 4 ),
 ( 0.000000000000000000, 1.000000000000000000 ),
 .UNSPECIFIED. ) ;
#29181 = CARTESIAN_POINT ( 'NONE',  ( -7.999999999684021645, -16.70556587905094759, -33.14831771973513241 ) ) ;
#29182 = CARTESIAN_POINT ( 'NONE',  ( -17.42926651578709496, -22.00025083071089682, -29.45738651627399918 ) ) ;
#29183 = ORIENTED_EDGE ( 'NONE', *, *, #3459, .F. ) ;
#29184 = CARTESIAN_POINT ( 'NONE',  ( 14.63279312439391155, -31.99961502282818415, -26.42651388579572114 ) ) ;
#29185 = CARTESIAN_POINT ( 'NONE',  ( -8.000000000457589522, -24.26136093481186862, -29.62468611113247263 ) ) ;
#29186 = CARTESIAN_POINT ( 'NONE',  ( -10.27234744519999943, 6.417650034250000246, 231.9999989789999972 ) ) ;
#29187 = DIRECTION ( 'NONE',  ( -0.9915824307782121760, 0.1294769592320275942, 0.000000000000000000 ) ) ;
#29188 = CARTESIAN_POINT ( 'NONE',  ( 23.95489023949999918, -14.10735628980000023, 223.9201486480000085 ) ) ;
#29189 = CARTESIAN_POINT ( 'NONE',  ( 2.033218777617324502, -21.81692582114836654, -30.17614928724987777 ) ) ;
#29191 = B_SPLINE_CURVE_WITH_KNOTS ( 'NONE', 3,
 ( #9806, #26789, #5233, #2568, #19563, #3026 ),
 .UNSPECIFIED., .F., .F.,
 ( 4, 2, 4 ),
 ( 0.000000000000000000, 0.5000000000000000000, 1.000000000000000000 ),
 .UNSPECIFIED. ) ;
#29190 = CARTESIAN_POINT ( 'NONE',  ( -17.05870563379187033, -7.915918418981195970, 0.000000000000000000 ) ) ;
#29192 = CARTESIAN_POINT ( 'NONE',  ( -25.36600720539997766, -15.15696894355576241, -0.2432540810000105580 ) ) ;
#29193 = CARTESIAN_POINT ( 'NONE',  ( -8.000000000000000000, -15.86465192213301556, -74.65259062561435144 ) ) ;
#29194 = CARTESIAN_POINT ( 'NONE',  ( 17.16657240420000008, 10.97998838177520931, -1.452769935612311825 ) ) ;
#29195 = CARTESIAN_POINT ( 'NONE',  ( -7.999999999674821005, -13.66746466538290328, -34.50691966471094929 ) ) ;
#29196 = EDGE_CURVE ( 'NONE', #11537, #2785, #2280, .T. ) ;
#29197 = B_SPLINE_CURVE_WITH_KNOTS ( 'NONE', 3,
 ( #14703, #14397, #2586, #21633, #5092, #10133 ),
 .UNSPECIFIED., .F., .F.,
 ( 4, 2, 4 ),
 ( 0.000000000000000000, 0.5000000000000000000, 1.000000000000000000 ),
 .UNSPECIFIED. ) ;
#29198 = CARTESIAN_POINT ( 'NONE',  ( -23.95771898009571999, -13.50170546721040310, 6.071909320494010665 ) ) ;
#29199 = CARTESIAN_POINT ( 'NONE',  ( -2.595987296770099650, -18.41037502479620969, -108.0771722350183381 ) ) ;
#29200 = EDGE_LOOP ( 'NONE', ( #19578, #13184, #3257, #2514 ) ) ;
#29201 = ADVANCED_FACE ( 'NONE', ( #10556 ), #30840, .T. ) ;
#29202 = CARTESIAN_POINT ( 'NONE',  ( 20.30396079662882158, 20.00000000004802203, 1.400000000000012346 ) ) ;
#29203 = DIRECTION ( 'NONE',  ( 1.000000000000000000, 0.000000000000000000, 0.000000000000000000 ) ) ;
#29204 = LINE ( 'NONE', #10027, #19481 ) ;
#29205 = CARTESIAN_POINT ( 'NONE',  ( 5.975646968830259809, -0.1056191442178888718, -58.57793411332500000 ) ) ;
#29206 = ORIENTED_EDGE ( 'NONE', *, *, #23034, .F. ) ;
#29207 = CONTEXT_DEPENDENT_SHAPE_REPRESENTATION ( #17416, #14249 ) ;
#29208 = ORIENTED_EDGE ( 'NONE', *, *, #2519, .T. ) ;
#29209 = CARTESIAN_POINT ( 'NONE',  ( -17.43404799081794465, -25.38543018601581736, -23.55866962503008821 ) ) ;
#29210 = ORIENTED_EDGE ( 'NONE', *, *, #22290, .T. ) ;
#29211 = VERTEX_POINT ( 'NONE', #17620 ) ;
#29212 = EDGE_CURVE ( 'NONE', #22033, #30387, #20658, .T. ) ;
#29213 =( NAMED_UNIT ( * ) PLANE_ANGLE_UNIT ( ) SI_UNIT ( $, .RADIAN. ) );
#29214 = CARTESIAN_POINT ( 'NONE',  ( -24.00289803497245700, 14.02635913871703011, 4.098597478000010064 ) ) ;
#29215 = CARTESIAN_POINT ( 'NONE',  ( -25.17013648539154147, -13.36928061894358244, 224.5014256759218370 ) ) ;
#29216 = ADVANCED_FACE ( 'NONE', ( #1425 ), #20297, .T. ) ;
#29217 = B_SPLINE_SURFACE_WITH_KNOTS ( 'NONE', 5, 1, ( 
 ( #13805, #30952 ),
 ( #18983, #23252 ),
 ( #25772, #2321 ),
 ( #1849, #11903 ),
 ( #6559, #16772 ),
 ( #9224, #28734 ),
 ( #30495, #25927 ),
 ( #28589, #4362 ),
 ( #13648, #13965 ),
 ( #16467, #23576 ),
 ( #26081, #4520 ),
 ( #31105, #14118 ),
 ( #7031, #23722 ),
 ( #2161, #11749 ),
 ( #16620, #26228 ) ),
 .UNSPECIFIED., .F., .F., .F.,
 ( 6, 3, 3, 3, 6 ),
 ( 2, 2 ),
 ( 0.000000000000000000, 0.5239015562240000312, 1.047803112450000018, 1.571704668670000027, 1.746338520749999956 ),
 ( -0.7000000000009999335, 2.556819966299999618E-06 ),
 .UNSPECIFIED. ) ;
#29218 = CIRCLE ( 'NONE', #16662, 2.000000000010000889 ) ;
#29219 = CARTESIAN_POINT ( 'NONE',  ( 6.460394865750000548, 10.46154704049999928, 232.6627648150000027 ) ) ;
#29220 = CARTESIAN_POINT ( 'NONE',  ( 10.69999999996467288, -29.52967710426907288, -26.74956343519520274 ) ) ;
#29221 = CARTESIAN_POINT ( 'NONE',  ( 4.416054526660082580, -3.250752328011468961, -7.972776792900008402 ) ) ;
#29222 = VECTOR ( 'NONE', #829, 999.9999999999998863 ) ;
#29223 = CARTESIAN_POINT ( 'NONE',  ( 13.99999999979999821, 20.99999999999999645, -67.09999999999999432 ) ) ;
#29224 = EDGE_LOOP ( 'NONE', ( #6540, #12269, #9059, #5715 ) ) ;
#29225 = CARTESIAN_POINT ( 'NONE',  ( 1.704222867702336552, -3.764723383760178343, -44.10000000002499831 ) ) ;
#29226 = AXIS2_PLACEMENT_3D ( 'NONE', #28219, #16260, #4314 ) ;
#29227 = CARTESIAN_POINT ( 'NONE',  ( -4.861312627796362307, -13.76085703350993228, -30.76755074928387401 ) ) ;
#29228 = CARTESIAN_POINT ( 'NONE',  ( 4.979326355943800131, -2.377326608238005790, -21.88180150030000348 ) ) ;
#29229 = CARTESIAN_POINT ( 'NONE',  ( 14.85000000009999788, -27.00000000000000000, -28.39999999989999679 ) ) ;
#29230 = CARTESIAN_POINT ( 'NONE',  ( 0.09666810063946208731, -27.50000000000001066, 226.1000000000000227 ) ) ;
#29231 = CARTESIAN_POINT ( 'NONE',  ( -10.20188979230000115, 6.555481593160000564, 230.6412452697800006 ) ) ;
#29232 = DIRECTION ( 'NONE',  ( 0.000000000000000000, 0.000000000000000000, 1.000000000000000000 ) ) ;
#29233 = CARTESIAN_POINT ( 'NONE',  ( -3.250950776947242993, -3.159825117472811140, -46.80083066912501266 ) ) ;
#29234 = CARTESIAN_POINT ( 'NONE',  ( -10.69999999999999929, -127.2537393281999982, -34.36317439833000265 ) ) ;
#29235 = CARTESIAN_POINT ( 'NONE',  ( 10.69999999999999929, -27.00000000000000000, -31.39999999999999858 ) ) ;
#29236 = CARTESIAN_POINT ( 'NONE',  ( -24.93720648713954446, 13.79881813474513486, 6.099998581000020792 ) ) ;
#29237 = ADVANCED_FACE ( 'NONE', ( #13057 ), #17919, .T. ) ;
#29238 = CARTESIAN_POINT ( 'NONE',  ( -26.73216212440000206, 9.347130611989999949, 229.4485730460000070 ) ) ;
#29239 = PLANE ( 'NONE',  #11744 ) ;
#29240 = VECTOR ( 'NONE', #3264, 1000.000000000000114 ) ;
#29241 = B_SPLINE_CURVE_WITH_KNOTS ( 'NONE', 3,
 ( #2022, #23264, #6419, #16478, #30808, #16017 ),
 .UNSPECIFIED., .F., .F.,
 ( 4, 2, 4 ),
 ( 0.000000000000000000, 0.5000000000000008882, 1.000000000000000000 ),
 .UNSPECIFIED. ) ;
#29242 = VERTEX_POINT ( 'NONE', #27228 ) ;
#29243 = CARTESIAN_POINT ( 'NONE',  ( 5.869757812515316253, 0.5877190740209992104, -30.63116556699999649 ) ) ;
#29244 = ORIENTED_EDGE ( 'NONE', *, *, #4048, .F. ) ;
#29245 = CARTESIAN_POINT ( 'NONE',  ( 25.12046395012945155, -13.46291002088068289, 3.957489296000010981 ) ) ;
#29246 = CARTESIAN_POINT ( 'NONE',  ( 4.432674687120906398, 4.607520344841867121, -48.69426496242499525 ) ) ;
#29247 = ORIENTED_EDGE ( 'NONE', *, *, #21269, .F. ) ;
#29248 = EDGE_CURVE ( 'NONE', #25714, #28115, #12753, .T. ) ;
#29249 = ORIENTED_EDGE ( 'NONE', *, *, #15208, .T. ) ;
#29250 = DIRECTION ( 'NONE',  ( -2.775557561562891351E-17, 0.000000000000000000, 1.000000000000000000 ) ) ;
#29251 = ORIENTED_EDGE ( 'NONE', *, *, #24471, .T. ) ;
#29252 = CARTESIAN_POINT ( 'NONE',  ( 20.11799773827349824, 19.99998646409962433, 229.6587445809824146 ) ) ;
#29253 = EDGE_LOOP ( 'NONE', ( #4335, #674 ) ) ;
#29254 = CARTESIAN_POINT ( 'NONE',  ( 8.000000000479330353, -14.59835909869570081, -37.69297980903808565 ) ) ;
#29255 = CARTESIAN_POINT ( 'NONE',  ( 24.98081130624543889, 13.71897605842228529, 4.999998581000003384 ) ) ;
#29256 = FACE_OUTER_BOUND ( 'NONE', #21649, .T. ) ;
#29257 = DIRECTION ( 'NONE',  ( 0.000000000000000000, -1.000000000000000000, 0.000000000000000000 ) ) ;
#29258 = CARTESIAN_POINT ( 'NONE',  ( -12.42573721508254714, -28.24511507758019135, -23.34563525619502755 ) ) ;
#29259 = EDGE_CURVE ( 'NONE', #18513, #23194, #15272, .T. ) ;
#29260 = CARTESIAN_POINT ( 'NONE',  ( 9.499999999864446210, -15.71418478743095548, -37.87087219225396950 ) ) ;
#29261 = CARTESIAN_POINT ( 'NONE',  ( 0.000000000000000000, 0.000000000000000000, 115.0000000000000000 ) ) ;
#29262 = AXIS2_PLACEMENT_3D ( 'NONE', #24871, #3449, #10394 ) ;
#29263 = CARTESIAN_POINT ( 'NONE',  ( -23.79652740965775237, -14.37370918960761657, 224.0358530723576393 ) ) ;
#29264 = ORIENTED_EDGE ( 'NONE', *, *, #9638, .F. ) ;
#29265 = CARTESIAN_POINT ( 'NONE',  ( -3.925562765917044228, -3.929887376319241898, -10.81399163100000216 ) ) ;
#29266 = CARTESIAN_POINT ( 'NONE',  ( -2.126050624815288614, 4.685496013473724020, -30.78885571289999845 ) ) ;
#29267 = DIRECTION ( 'NONE',  ( 0.000000000000000000, 0.000000000000000000, -1.000000000000000000 ) ) ;
#29268 = CARTESIAN_POINT ( 'NONE',  ( 24.20792487550426841, -13.66932880343719781, 6.079865098000015067 ) ) ;
#29269 = DIRECTION ( 'NONE',  ( -1.000000000000000000, 5.687697999151106851E-16, -6.771501495036750356E-12 ) ) ;
#29270 = CARTESIAN_POINT ( 'NONE',  ( -28.50000000000000000, -5.684341886079999373E-14, 229.0000000000000000 ) ) ;
#29271 = CARTESIAN_POINT ( 'NONE',  ( 0.9902601296000002051, -27.78262976010000074, 225.5064715119999903 ) ) ;
#29272 = CARTESIAN_POINT ( 'NONE',  ( -4.274658871253798509, -0.8336587121505270037, -31.09652066320001040 ) ) ;
#29273 = CARTESIAN_POINT ( 'NONE',  ( 1.157672466183025994, -27.77645868488734138, 5.900907654000003610 ) ) ;
#29274 =( REPRESENTATION_RELATIONSHIP ('NONE','NONE', #2712, #28252 ) REPRESENTATION_RELATIONSHIP_WITH_TRANSFORMATION ( #6878 )SHAPE_REPRESENTATION_RELATIONSHIP( ) );
#29275 = CARTESIAN_POINT ( 'NONE',  ( -24.34942396232675321, -13.41447636113284680, 4.689458291000009105 ) ) ;
#29276 = CARTESIAN_POINT ( 'NONE',  ( -0.9470189794284002982, -3.499851337386873595, 230.7636321640559913 ) ) ;
#29277 = EDGE_CURVE ( 'NONE', #22078, #1493, #10246, .T. ) ;
#29278 = EDGE_LOOP ( 'NONE', ( #30072, #11219, #29939, #19046 ) ) ;
#29279 = EDGE_CURVE ( 'NONE', #4649, #19471, #5669, .T. ) ;
#29280 = FACE_OUTER_BOUND ( 'NONE', #14501, .T. ) ;
#29281 = CARTESIAN_POINT ( 'NONE',  ( -2.540108707139367539, -20.45867351756849928, -27.50080737777486561 ) ) ;
#29282 = VERTEX_POINT ( 'NONE', #19993 ) ;
#29283 = CARTESIAN_POINT ( 'NONE',  ( 0.9307262455818937630, 1.887507898842907927, 226.6412452697800290 ) ) ;
#29284 = DIRECTION ( 'NONE',  ( -1.000000000000000000, 5.665498452320000818E-16, 0.000000000000000000 ) ) ;
#29286 = ORIENTED_EDGE ( 'NONE', *, *, #18343, .F. ) ;
#29285 = CONICAL_SURFACE ( 'NONE', #3653, 1.120011618224791450, 0.0001253086068439055573 ) ;
#29287 = CARTESIAN_POINT ( 'NONE',  ( -4.523686073471028024, 1.015938900863429195, -44.10000000002499831 ) ) ;
#29288 = ORIENTED_EDGE ( 'NONE', *, *, #17652, .F. ) ;
#29289 = ORIENTED_EDGE ( 'NONE', *, *, #6981, .F. ) ;
#29290 = SURFACE_STYLE_FILL_AREA ( #10109 ) ;
#29291 = EDGE_LOOP ( 'NONE', ( #3273, #28984, #26782, #1152 ) ) ;
#29292 = CARTESIAN_POINT ( 'NONE',  ( 28.35924375250000296, 3.617365304089999312E-14, 229.7625741969999922 ) ) ;
#29293 = CARTESIAN_POINT ( 'NONE',  ( 10.00000000070000183, -130.0000000000000000, -41.24671599790000442 ) ) ;
#29294 = CARTESIAN_POINT ( 'NONE',  ( 0.000000000000000000, 0.000000000000000000, 227.6412452697800006 ) ) ;
#29295 = ORIENTED_EDGE ( 'NONE', *, *, #157, .F. ) ;
#29296 = CARTESIAN_POINT ( 'NONE',  ( -25.12046394328145382, 13.46291001830483580, 6.042507865999996675 ) ) ;
#29297 = DIRECTION ( 'NONE',  ( 0.000000000000000000, 0.000000000000000000, -1.000000000000000000 ) ) ;
#29298 = DIRECTION ( 'NONE',  ( 1.000000000000000000, 0.000000000000000000, 0.000000000000000000 ) ) ;
#29299 = CARTESIAN_POINT ( 'NONE',  ( -6.585786437629999490, -16.41511111490214603, -74.85294138696069410 ) ) ;
#29300 = AXIS2_PLACEMENT_3D ( 'NONE', #10695, #20289, #29893 ) ;
#29301 = CARTESIAN_POINT ( 'NONE',  ( 26.84464183080000055, -3.287411895189999871E-15, 42.56249624490000372 ) ) ;
#29302 = CARTESIAN_POINT ( 'NONE',  ( -4.180754675048095947, 1.217138862148074763, -16.30443125759999745 ) ) ;
#29303 = CARTESIAN_POINT ( 'NONE',  ( -23.25788685383075105, -13.43083806724683882, 193.2171415880000040 ) ) ;
#29304 = CARTESIAN_POINT ( 'NONE',  ( 8.000000000279957391, -18.28443193505134445, -36.42483736938841332 ) ) ;
#29305 = DIRECTION ( 'NONE',  ( 1.000000000000000000, -1.841917067661885521E-12, 2.653884470265303553E-12 ) ) ;
#29306 = CARTESIAN_POINT ( 'NONE',  ( 27.79999999460000026, 2.375185947459999891, 222.0000000000000000 ) ) ;
#29307 = CARTESIAN_POINT ( 'NONE',  ( 23.34136241352823404, 16.91641428746209286, 1.000000000000000888 ) ) ;
#29308 = DIRECTION ( 'NONE',  ( 1.000000000000000000, 0.000000000000000000, 0.000000000000000000 ) ) ;
#29309 = CARTESIAN_POINT ( 'NONE',  ( 26.12735226819999923, 9.150265136599999849, 229.9751247030000059 ) ) ;
#29310 = CARTESIAN_POINT ( 'NONE',  ( 24.50000001620000134, -3.000285568839999855E-15, 140.0000000040000145 ) ) ;
#29311 = EDGE_CURVE ( 'NONE', #3166, #11286, #22663, .T. ) ;
#29312 = EDGE_LOOP ( 'NONE', ( #15643, #28236, #13217, #266 ) ) ;
#29313 = CARTESIAN_POINT ( 'NONE',  ( -5.212126283948660621, -2.851000302232811201, -52.86982952342499686 ) ) ;
#29314 = DIRECTION ( 'NONE',  ( 0.000000000000000000, -0.3420201433259318913, 0.9396926207858126157 ) ) ;
#29315 = B_SPLINE_CURVE_WITH_KNOTS ( 'NONE', 3,
 ( #18837, #18528, #20737, #1391, #28130, #30804 ),
 .UNSPECIFIED., .F., .F.,
 ( 4, 2, 4 ),
 ( 0.000000000000000000, 0.5000000000000000000, 1.000000000000000000 ),
 .UNSPECIFIED. ) ;
#29316 = ADVANCED_FACE ( 'NONE', ( #10869 ), #29817, .T. ) ;
#29317 = CARTESIAN_POINT ( 'NONE',  ( 22.63260994176697238, -19.28417101125922883, -0.6999999999999784173 ) ) ;
#29318 = CARTESIAN_POINT ( 'NONE',  ( -4.361734194508183116, 1.139633373421352402, -68.10000000002500542 ) ) ;
#29319 = EDGE_CURVE ( 'NONE', #11709, #27054, #8482, .T. ) ;
#29320 = VECTOR ( 'NONE', #15124, 1000.000000000000000 ) ;
#29321 = ORIENTED_EDGE ( 'NONE', *, *, #3926, .T. ) ;
#29322 = AXIS2_PLACEMENT_3D ( 'NONE', #6447, #13848, #14006 ) ;
#29323 = CARTESIAN_POINT ( 'NONE',  ( -3.589938250752385596, -0.3047143574548395462, -93.72782493932767522 ) ) ;
#29324 = AXIS2_PLACEMENT_3D ( 'NONE', #18959, #28564, #2298 ) ;
#29325 = ORIENTED_EDGE ( 'NONE', *, *, #19425, .T. ) ;
#29326 = CARTESIAN_POINT ( 'NONE',  ( -6.000000000000000000, -15.18061163548115466, -76.53197586718597734 ) ) ;
#29327 = B_SPLINE_CURVE_WITH_KNOTS ( 'NONE', 5,
 ( #3488, #30087, #26956, #1138, #993, #24599 ),
 .UNSPECIFIED., .F., .F.,
 ( 6, 6 ),
 ( 3.365645383459999973, 3.604193613869999702 ),
 .UNSPECIFIED. ) ;
#29328 = CARTESIAN_POINT ( 'NONE',  ( -8.000000000026910030, -116.9355502247062617, 17.89675170932962089 ) ) ;
#29329 = ORIENTED_EDGE ( 'NONE', *, *, #21960, .F. ) ;
#29330 = CARTESIAN_POINT ( 'NONE',  ( 6.118976883090258667, 2.212479739890888197, -26.51249766020000109 ) ) ;
#29331 = FACE_OUTER_BOUND ( 'NONE', #11402, .T. ) ;
#29332 = CARTESIAN_POINT ( 'NONE',  ( -25.45339887876027163, 13.89659413885661365, 0.2374258030000131470 ) ) ;
#29333 = LINE ( 'NONE', #7777, #18041 ) ;
#29334 = DIRECTION ( 'NONE',  ( -0.000000000000000000, 1.000000000000000000, -2.258510841069999963E-12 ) ) ;
#29335 = CARTESIAN_POINT ( 'NONE',  ( -4.768428784999852788, -18.52815030097902493, -28.44238646348855681 ) ) ;
#29336 = VERTEX_POINT ( 'NONE', #29589 ) ;
#29337 = CARTESIAN_POINT ( 'NONE',  ( -7.999999999682374074, -15.09104283142151282, -33.18208307865850060 ) ) ;
#29338 = AXIS2_PLACEMENT_3D ( 'NONE', #18164, #20222, #20535 ) ;
#29339 = DIRECTION ( 'NONE',  ( 2.764802276011834743E-12, 0.9128796883888953273, -0.4082287037029531662 ) ) ;
#29340 = ORIENTED_EDGE ( 'NONE', *, *, #7644, .F. ) ;
#29341 = CARTESIAN_POINT ( 'NONE',  ( 14.73716614372071376, -31.99975091343083022, -26.99668318814331158 ) ) ;
#29342 = DIRECTION ( 'NONE',  ( 1.000000000000000000, -1.224606353819998843E-16, 0.000000000000000000 ) ) ;
#29343 = AXIS2_PLACEMENT_3D ( 'NONE', #1384, #30496, #30166 ) ;
#29345 = ADVANCED_FACE ( 'NONE', ( #24877 ), #12231, .T. ) ;
#29344 = TOROIDAL_SURFACE ( 'NONE', #2233, 24.50000000000000000, 3.200000000000000178 ) ;
#29346 = CARTESIAN_POINT ( 'NONE',  ( -23.83861932771936765, -15.61961844720760340, 5.310552105000033052 ) ) ;
#29347 = CARTESIAN_POINT ( 'NONE',  ( -3.244486662300113622, -0.9559324580886872091, -96.93852766387357178 ) ) ;
#29348 = CARTESIAN_POINT ( 'NONE',  ( -24.33897390745588751, -13.43341002469357548, 4.640669265424538281 ) ) ;
#29349 = VECTOR ( 'NONE', #12700, 1000.000000000000114 ) ;
#29350 = CARTESIAN_POINT ( 'NONE',  ( -4.421808970600616284, -26.43392618132182292, 209.5992702222104640 ) ) ;
#29351 = CARTESIAN_POINT ( 'NONE',  ( 2.458800944228217933, -3.193228378228379238, -0.6999999999999992895 ) ) ;
#29352 = CARTESIAN_POINT ( 'NONE',  ( 14.53700916270368459, -27.90446693802870826, 0.2374258030000131470 ) ) ;
#29353 = FACE_OUTER_BOUND ( 'NONE', #22298, .T. ) ;
#29354 = FILL_AREA_STYLE ('',( #5590 ) ) ;
#29355 = FACE_OUTER_BOUND ( 'NONE', #30547, .T. ) ;
#29356 = CARTESIAN_POINT ( 'NONE',  ( -9.484767271962882162, -25.06561782275614547, 25.91365951406786294 ) ) ;
#29357 = CARTESIAN_POINT ( 'NONE',  ( -0.6094664100040195764, -28.49364619262437870, 4.999998581000003384 ) ) ;
#29358 = PRESENTATION_LAYER_ASSIGNMENT (  '', '', ( #24341 ) ) ;
#29359 = ORIENTED_EDGE ( 'NONE', *, *, #7674, .T. ) ;
#29360 = CARTESIAN_POINT ( 'NONE',  ( 11.66358246589999936, -24.14124255329999968, -1.399999999999998579 ) ) ;
#29361 = CARTESIAN_POINT ( 'NONE',  ( 24.71695093370000151, -14.18891100779999981, 226.0986570600000221 ) ) ;
#29362 = VECTOR ( 'NONE', #19225, 1000.000000000000000 ) ;
#29363 = CARTESIAN_POINT ( 'NONE',  ( -4.050122923326521018, -2.059172231882739457, -62.76424626872500312 ) ) ;
#29364 = VECTOR ( 'NONE', #27812, 1000.000000000000000 ) ;
#29365 = ORIENTED_EDGE ( 'NONE', *, *, #22789, .F. ) ;
#29366 = CIRCLE ( 'NONE', #1736, 4.997501249380000843 ) ;
#29367 = AXIS2_PLACEMENT_3D ( 'NONE', #20448, #6125, #15719 ) ;
#29368 = VERTEX_POINT ( 'NONE', #30207 ) ;
#29369 = CARTESIAN_POINT ( 'NONE',  ( 10.45000000009999930, -26.99999999999950617, -28.39999999990030588 ) ) ;
#29370 = ORIENTED_EDGE ( 'NONE', *, *, #16284, .T. ) ;
#29371 = EDGE_CURVE ( 'NONE', #8103, #359, #767, .T. ) ;
#29372 = CARTESIAN_POINT ( 'NONE',  ( 0.000000000000000000, 0.000000000000000000, 230.0000000000000000 ) ) ;
#29373 = CARTESIAN_POINT ( 'NONE',  ( -24.30808044443811156, 13.48997716914403533, 3.899998581000013509 ) ) ;
#29374 = CARTESIAN_POINT ( 'NONE',  ( -26.79999999999999361, -1.754055898254264445, 143.2171415879999756 ) ) ;
#29375 = ADVANCED_FACE ( 'NONE', ( #27847 ), #16356, .T. ) ;
#29376 = CARTESIAN_POINT ( 'NONE',  ( 11.47889647200000063, 4.402643528619999636, 232.6627648150000027 ) ) ;
#29377 = CARTESIAN_POINT ( 'NONE',  ( 24.34137756859324853, -13.42980563341176037, 6.099998581000020792 ) ) ;
#29378 = CARTESIAN_POINT ( 'NONE',  ( -4.184186767956290964, -1.312611723764788296, -9.523230888999998811 ) ) ;
#29379 = AXIS2_PLACEMENT_3D ( 'NONE', #6856, #16457, #16306 ) ;
#29380 = STYLED_ITEM ( 'NONE', ( #25554 ), #17044 ) ;
#29381 = CARTESIAN_POINT ( 'NONE',  ( 28.04325408110000240, -4.263256414559999688E-14, 230.2432540810000319 ) ) ;
#29382 = ORIENTED_EDGE ( 'NONE', *, *, #21142, .T. ) ;
#29383 = CARTESIAN_POINT ( 'NONE',  ( 2.636753967748677763, -3.464035022006507702, -44.10000000002499121 ) ) ;
#29384 = CARTESIAN_POINT ( 'NONE',  ( -24.98081131316241255, -13.71897606304888662, 4.895818166000015736 ) ) ;
#29385 = EDGE_CURVE ( 'NONE', #2672, #26555, #1890, .T. ) ;
#29386 = CARTESIAN_POINT ( 'NONE',  ( -3.251750336246070461, -5.089746299513510763, -21.70891267860000795 ) ) ;
#29387 = CARTESIAN_POINT ( 'NONE',  ( -12.41832131459880273, -25.71382967685944365, -33.43067980453216137 ) ) ;
#29388 = DIRECTION ( 'NONE',  ( 0.000000000000000000, 0.000000000000000000, 1.000000000000000000 ) ) ;
#29389 = CARTESIAN_POINT ( 'NONE',  ( 9.999999999969375608, -29.39900052789773000, -30.24364015896112434 ) ) ;
#29390 = AXIS2_PLACEMENT_3D ( 'NONE', #1692, #3568, #25457 ) ;
#29391 = CARTESIAN_POINT ( 'NONE',  ( -23.50695067596906185, -14.84192170558064738, 225.0734924212516432 ) ) ;
#29392 = CARTESIAN_POINT ( 'NONE',  ( -4.251810618965843780, 2.500173132353668226, -44.09354844312500177 ) ) ;
#29393 = CARTESIAN_POINT ( 'NONE',  ( -10.69999999999999929, -120.8032508028999956, -31.27837281569999917 ) ) ;
#29394 = FACE_OUTER_BOUND ( 'NONE', #22216, .T. ) ;
#29395 = CARTESIAN_POINT ( 'NONE',  ( -19.41377926560965506, 19.99999670840111676, 230.3187478872601162 ) ) ;
#29396 = CARTESIAN_POINT ( 'NONE',  ( -27.09307779339999911, -1.459449460099999974E-12, 229.9751247039999953 ) ) ;
#29397 = EDGE_CURVE ( 'NONE', #15988, #23469, #14317, .T. ) ;
#29398 = CARTESIAN_POINT ( 'NONE',  ( -17.36983091284663061, -9.971084190247578860, -0.6999999999999784173 ) ) ;
#29399 = VERTEX_POINT ( 'NONE', #25965 ) ;
#29400 = CARTESIAN_POINT ( 'NONE',  ( 0.6138679561251692007, 4.311712124478116692, -29.50600711719999936 ) ) ;
#29401 = CIRCLE ( 'NONE', #6298, 26.79999999889999884 ) ;
#29402 = ORIENTED_EDGE ( 'NONE', *, *, #16435, .T. ) ;
#29403 = CARTESIAN_POINT ( 'NONE',  ( 24.78870453580057998, -12.58522324566301620, 4.492873455000018446 ) ) ;
#29404 = CARTESIAN_POINT ( 'NONE',  ( 3.874396413951474827, -2.399869827310081583, -49.73324460762500365 ) ) ;
#29405 = ORIENTED_EDGE ( 'NONE', *, *, #11241, .F. ) ;
#29406 = VERTEX_POINT ( 'NONE', #1739 ) ;
#29407 = APPLICATION_PROTOCOL_DEFINITION ( 'draft international standard', 'automotive_design', 1998, #28867 ) ;
#29408 = ORIENTED_EDGE ( 'NONE', *, *, #24170, .F. ) ;
#29409 = VERTEX_POINT ( 'NONE', #23613 ) ;
#29410 = CARTESIAN_POINT ( 'NONE',  ( 11.20000000009999930, -27.00000000000000000, -34.17350269180000311 ) ) ;
#29411 = CARTESIAN_POINT ( 'NONE',  ( 28.68577476828162531, -9.950727360111285336, 1.000000000000000888 ) ) ;
#29412 = DIRECTION ( 'NONE',  ( 0.000000000000000000, -1.000000000000000000, 0.000000000000000000 ) ) ;
#29413 = DIRECTION ( 'NONE',  ( -2.257127817980000114E-12, 0.000000000000000000, -1.000000000000000000 ) ) ;
#29414 = B_SPLINE_CURVE_WITH_KNOTS ( 'NONE', 3,
 ( #23541, #14241, #14400, #28708, #9350, #21477 ),
 .UNSPECIFIED., .F., .F.,
 ( 4, 2, 4 ),
 ( 0.000000000000000000, 0.5000000000000000000, 1.000000000000000000 ),
 .UNSPECIFIED. ) ;
#29415 = B_SPLINE_CURVE_WITH_KNOTS ( 'NONE', 3,
 ( #26437, #2822, #7387, #24387, #635, #24080 ),
 .UNSPECIFIED., .F., .F.,
 ( 4, 2, 4 ),
 ( 0.000000000000000000, 0.5000000000000000000, 1.000000000000000000 ),
 .UNSPECIFIED. ) ;
#29416 = CARTESIAN_POINT ( 'NONE',  ( -9.897162125286939727, -25.37356426548038613, 188.3395398250000028 ) ) ;
#29417 = CARTESIAN_POINT ( 'NONE',  ( -4.301560380444131582, 2.091195337698785295, -0.6999999999999991784 ) ) ;
#29418 = CARTESIAN_POINT ( 'NONE',  ( 2.223383862040879677, -3.430296892840221101, 0.3340606116999991215 ) ) ;
#29419 = DIRECTION ( 'NONE',  ( 1.000000000000000000, 6.668066630619518976E-24, -2.257150022442225012E-12 ) ) ;
#29420 = VERTEX_POINT ( 'NONE', #4403 ) ;
#29421 = ADVANCED_FACE ( 'NONE', ( #18405 ), #13531, .F. ) ;
#29422 = CARTESIAN_POINT ( 'NONE',  ( -1.831588579526997940, 3.958388136463042439, -7.731725184300007214 ) ) ;
#29423 = CARTESIAN_POINT ( 'NONE',  ( 2.224662748255027633, -4.232576503996232198, -32.26971934059999825 ) ) ;
#29424 = CARTESIAN_POINT ( 'NONE',  ( 0.9559440766510057808, -27.78378678420316206, 225.5621479832471437 ) ) ;
#29425 = PRODUCT_DEFINITION_FORMATION_WITH_SPECIFIED_SOURCE ( 'ANY', '', #29916, .NOT_KNOWN. ) ;
#29426 = CARTESIAN_POINT ( 'NONE',  ( 24.30808045080437907, -13.48997717272881047, 6.099998581000020792 ) ) ;
#29427 = CARTESIAN_POINT ( 'NONE',  ( -24.47688144805034938, -13.18130191084491010, 225.7329853482806357 ) ) ;
#29428 = CARTESIAN_POINT ( 'NONE',  ( -27.50000000000000000, 3.367667473009999970E-15, 0.000000000000000000 ) ) ;
#29429 = CARTESIAN_POINT ( 'NONE',  ( -7.973786364210958766, -115.4211104591501993, 21.28333694629189665 ) ) ;
#29430 = CARTESIAN_POINT ( 'NONE',  ( -3.500772897184936561, -3.093025330206538470, -33.83447003410000775 ) ) ;
#29431 = CARTESIAN_POINT ( 'NONE',  ( 1.605176535610508326, -27.75389821387976852, 4.999998581000003384 ) ) ;
#29432 = CARTESIAN_POINT ( 'NONE',  ( 10.89131017049999883, -25.00000000000000000, -1.811764705999995062 ) ) ;
#29433 = CARTESIAN_POINT ( 'NONE',  ( 22.97695743748386832, 16.89262754991261062, 7.000000000000006217 ) ) ;
#29434 = ORIENTED_EDGE ( 'NONE', *, *, #2843, .T. ) ;
#29435 = ADVANCED_FACE ( 'NONE', ( #11172 ), #3938, .F. ) ;
#29436 = EDGE_CURVE ( 'NONE', #790, #26662, #11689, .T. ) ;
#29437 = DIRECTION ( 'NONE',  ( 0.000000000000000000, -2.257145581549999994E-12, -1.000000000000000000 ) ) ;
#29438 = CARTESIAN_POINT ( 'NONE',  ( 10.69999999999822826, -24.07808197001402917, -27.61475634682798841 ) ) ;
#29439 = ORIENTED_EDGE ( 'NONE', *, *, #1742, .F. ) ;
#29440 = ADVANCED_FACE ( 'NONE', ( #25662 ), #4091, .F. ) ;
#29441 = DIRECTION ( 'NONE',  ( 0.000000000000000000, -1.000000000000000000, 2.257145581549999994E-12 ) ) ;
#29442 = CARTESIAN_POINT ( 'NONE',  ( 7.707106507606773960, -115.2381290211091738, 21.69251943803729787 ) ) ;
#29443 = VERTEX_POINT ( 'NONE', #2205 ) ;
#29444 = CARTESIAN_POINT ( 'NONE',  ( -4.895342878087565630, -0.3722554304256932567, -44.10000000002499121 ) ) ;
#29445 = ORIENTED_EDGE ( 'NONE', *, *, #12099, .F. ) ;
#29446 = ORIENTED_EDGE ( 'NONE', *, *, #26211, .F. ) ;
#29447 = B_SPLINE_CURVE_WITH_KNOTS ( 'NONE', 3,
 ( #29141, #31049, #28683, #60, #28827, #7286, #3630, #22538, #5532, #22682 ),
 .UNSPECIFIED., .F., .F.,
 ( 4, 2, 2, 2, 4 ),
 ( 0.000000000000000000, 0.2500000000000000000, 0.4999999999999999445, 0.7500000000000000000, 1.000000000000000000 ),
 .UNSPECIFIED. ) ;
#29448 = EDGE_CURVE ( 'NONE', #18243, #24363, #29680, .T. ) ;
#29449 = ORIENTED_EDGE ( 'NONE', *, *, #29708, .F. ) ;
#29450 = CARTESIAN_POINT ( 'NONE',  ( 25.84472112319999937, 9.051226241569999331, 230.6999999999999886 ) ) ;
#29451 = CARTESIAN_POINT ( 'NONE',  ( -28.49999999979999998, 7.466149641079999455, 222.0000000000000000 ) ) ;
#29452 = CARTESIAN_POINT ( 'NONE',  ( 16.08958307947758470, -8.732827806336466381, -0.6999999999999784173 ) ) ;
#29453 = VERTEX_POINT ( 'NONE', #23458 ) ;
#29454 = CARTESIAN_POINT ( 'NONE',  ( -20.30396346370000060, 20.00000000000000000, 228.1999999999999886 ) ) ;
#29455 = CARTESIAN_POINT ( 'NONE',  ( -24.06826084733133797, 20.50742046740553093, 8.000000000000007105 ) ) ;
#29456 = ADVANCED_FACE ( 'NONE', ( #29394 ), #16658, .F. ) ;
#29457 = CYLINDRICAL_SURFACE ( 'NONE', #1496, 2.000000000000004441 ) ;
#29458 = CARTESIAN_POINT ( 'NONE',  ( -10.69999999999999929, -26.63513617180875670, -25.40000000000000213 ) ) ;
#29459 = B_SPLINE_CURVE_WITH_KNOTS ( 'NONE', 5,
 ( #10808, #20402, #755, #10346, #29989, #15671, #25283, #3718, #19939 ),
 .UNSPECIFIED., .F., .F.,
 ( 6, 3, 6 ),
 ( 0.000000000000000000, 54.03331039209999886, 92.56095350929999199 ),
 .UNSPECIFIED. ) ;
#29460 = CARTESIAN_POINT ( 'NONE',  ( 4.373195337096347224, -2.904765488536225515, 0.04124526979999709742 ) ) ;
#29461 = CARTESIAN_POINT ( 'NONE',  ( -2.322678811625143780, -3.635533071076384015, -21.70891267860000795 ) ) ;
#29462 = CYLINDRICAL_SURFACE ( 'NONE', #22390, 1.100000000000000089 ) ;
#29463 = APPLICATION_CONTEXT ( 'automotive_design' ) ;
#29464 = DIRECTION ( 'NONE',  ( -1.000000000000000000, 0.000000000000000000, -2.257144471330000330E-12 ) ) ;
#29465 = DIRECTION ( 'NONE',  ( -1.000000000000000000, 0.000000000000000000, 0.000000000000000000 ) ) ;
#29466 = CARTESIAN_POINT ( 'NONE',  ( 8.000000000248304488, -25.92947504235655032, -31.20249033167290165 ) ) ;
#29467 = CARTESIAN_POINT ( 'NONE',  ( -23.47117976025595354, -14.33053685711701419, 224.1195089972090102 ) ) ;
#29468 = ADVANCED_FACE ( 'NONE', ( #14931 ), #1689, .T. ) ;
#29469 = DIRECTION ( 'NONE',  ( 1.000000000000000000, 1.167320209990000089E-13, -2.253435535809999718E-12 ) ) ;
#29470 = CARTESIAN_POINT ( 'NONE',  ( -11.48163258379999974, -24.28840542069999842, -1.419991652300001128 ) ) ;
#29471 = CARTESIAN_POINT ( 'NONE',  ( -7.999999999703424791, -29.80249410822368006, -29.47052640025566816 ) ) ;
#29472 = ORIENTED_EDGE ( 'NONE', *, *, #30062, .T. ) ;
#29473 = CARTESIAN_POINT ( 'NONE',  ( -1.777987283592920020, 4.296653259772734046, -56.39652090042499566 ) ) ;
#29474 = CARTESIAN_POINT ( 'NONE',  ( -6.000000000000000000, -17.05999687705277879, -77.21601615383784178 ) ) ;
#29475 = B_SPLINE_CURVE_WITH_KNOTS ( 'NONE', 5,
 ( #9418, #19495, #21397, #9732, #19025, #2202 ),
 .UNSPECIFIED., .F., .F.,
 ( 6, 6 ),
 ( -2.300779637610000261, 0.000000000000000000 ),
 .UNSPECIFIED. ) ;
#29476 = B_SPLINE_CURVE_WITH_KNOTS ( 'NONE', 3,
 ( #9425, #23616, #23145, #16359, #14011, #30841 ),
 .UNSPECIFIED., .F., .F.,
 ( 4, 2, 4 ),
 ( 0.000000000000000000, 0.5000000000000000000, 1.000000000000000000 ),
 .UNSPECIFIED. ) ;
#29477 = CARTESIAN_POINT ( 'NONE',  ( -4.084346732781014566, 1.529807325146986807, -38.22530605782345958 ) ) ;
#29478 = CARTESIAN_POINT ( 'NONE',  ( -4.235963752770566693, 0.8297158020410684287, -68.10000000002500542 ) ) ;
#29479 = ORIENTED_EDGE ( 'NONE', *, *, #22964, .F. ) ;
#29480 = CARTESIAN_POINT ( 'NONE',  ( -1.111846212942793288, 3.388043077328151131, -88.52261276238974119 ) ) ;
#29481 = VERTEX_POINT ( 'NONE', #2511 ) ;
#29482 = DIRECTION ( 'NONE',  ( 1.000000000000000000, 0.000000000000000000, 0.000000000000000000 ) ) ;
#29483 = CARTESIAN_POINT ( 'NONE',  ( -7.999999999991574740, -117.2096321409668462, 12.46567123851033010 ) ) ;
#29484 = VERTEX_POINT ( 'NONE', #11943 ) ;
#29485 = CARTESIAN_POINT ( 'NONE',  ( 2.833778097863423717, 3.583098331959791771, -63.23768011632500219 ) ) ;
#29486 = CARTESIAN_POINT ( 'NONE',  ( -23.08867861179999892, -20.40921893140000165, 229.2930746810000073 ) ) ;
#29487 = STYLED_ITEM ( 'NONE', ( #9331 ), #10459 ) ;
#29488 = CARTESIAN_POINT ( 'NONE',  ( 16.06675444873834380, 10.97998838177521286, -1.000005633855494125E-09 ) ) ;
#29489 = EDGE_CURVE ( 'NONE', #17596, #19970, #26430, .T. ) ;
#29490 = DIRECTION ( 'NONE',  ( 0.000000000000000000, 0.3420201433259318913, -0.9396926207858126157 ) ) ;
#29491 = CARTESIAN_POINT ( 'NONE',  ( -7.999999999661212335, -10.00744863972343168, -36.67931076521506384 ) ) ;
#29492 = EDGE_LOOP ( 'NONE', ( #4067, #14137, #27470, #2853 ) ) ;
#29493 = UNCERTAINTY_MEASURE_WITH_UNIT (LENGTH_MEASURE( 1.000000000000000082E-05 ), #11540, 'distance_accuracy_value', 'NONE');
#29494 = EDGE_CURVE ( 'NONE', #25858, #1290, #708, .T. ) ;
#29495 = CARTESIAN_POINT ( 'NONE',  ( 24.60726958085803417, -14.37955347769869263, 4.098597479000015475 ) ) ;
#29496 = EDGE_CURVE ( 'NONE', #28711, #7680, #16913, .T. ) ;
#29497 = EDGE_CURVE ( 'NONE', #3121, #18573, #2814, .T. ) ;
#29498 = CARTESIAN_POINT ( 'NONE',  ( 18.92330595649999836, 19.72869720889999812, 229.8506619570000282 ) ) ;
#29499 = VERTEX_POINT ( 'NONE', #2361 ) ;
#29500 = CARTESIAN_POINT ( 'NONE',  ( 14.74203063447135165, -31.99976192563964972, -27.02823022071577341 ) ) ;
#29501 = CARTESIAN_POINT ( 'NONE',  ( 8.700000000291131741, -15.36262080770071670, -37.98492059649628771 ) ) ;
#29502 = CARTESIAN_POINT ( 'NONE',  ( -21.71008920740291259, 18.50699696262706695, 5.000000064000004407 ) ) ;
#29503 = CARTESIAN_POINT ( 'NONE',  ( 2.584869084651857385, -1.587944713799994467, -97.21305981300143628 ) ) ;
#29504 = CARTESIAN_POINT ( 'NONE',  ( 23.52644129050000288, -14.81042608839999808, 224.6894478949999723 ) ) ;
#29505 = CARTESIAN_POINT ( 'NONE',  ( -6.706468900734749106, -25.94814536837671426, 208.3914661911716735 ) ) ;
#29506 = PRODUCT_DEFINITION_SHAPE ( 'NONE', 'NONE',  #31130 ) ;
#29507 = CARTESIAN_POINT ( 'NONE',  ( 0.4034208554058360541, -3.803105581716118344, -0.6999999999999992895 ) ) ;
#29508 = CARTESIAN_POINT ( 'NONE',  ( 14.60916111670818474, -28.04296597385482315, 1.000000000000000888 ) ) ;
#29509 = DIRECTION ( 'NONE',  ( -6.181427515845962162E-12, 0.4082287037029531107, 0.9128796883888953273 ) ) ;
#29510 = CARTESIAN_POINT ( 'NONE',  ( 11.00000000000000000, 25.22617105830878614, -61.82510970417090590 ) ) ;
#29511 = CARTESIAN_POINT ( 'NONE',  ( -7.999999999680079021, -14.41853751394117111, -33.53780267086614231 ) ) ;
#29512 = CIRCLE ( 'NONE', #15450, 5.400000000370001274 ) ;
#29513 = VECTOR ( 'NONE', #4354, 1000.000000000000000 ) ;
#29514 = CARTESIAN_POINT ( 'NONE',  ( -23.82266443414333423, -12.31939917416737629, 93.21714158843887787 ) ) ;
#29515 = CARTESIAN_POINT ( 'NONE',  ( -0.5821515579339680002, -27.79407096281863687, 5.208100973000007627 ) ) ;
#29516 = ORIENTED_EDGE ( 'NONE', *, *, #17758, .F. ) ;
#29517 = LINE ( 'NONE', #5903, #26334 ) ;
#29518 = DIRECTION ( 'NONE',  ( 0.7071067811865475727, -0.7071067811865475727, 0.000000000000000000 ) ) ;
#29519 = CARTESIAN_POINT ( 'NONE',  ( -20.90359613196108057, 16.91137956061550085, -0.6999999999999992895 ) ) ;
#29520 = CARTESIAN_POINT ( 'NONE',  ( -4.892971904093138313, 0.02481116134537240947, -63.32122063472500173 ) ) ;
#29521 = ORIENTED_EDGE ( 'NONE', *, *, #3411, .F. ) ;
#29522 = ITEM_DEFINED_TRANSFORMATION ( 'NONE', 'NONE', #12343,  #17722 ) ;
#29523 = VERTEX_POINT ( 'NONE', #19500 ) ;
#29524 = CARTESIAN_POINT ( 'NONE',  ( 26.79556473285982321, 0.4875557887250580036, 0.000000000000000000 ) ) ;
#29525 = VERTEX_POINT ( 'NONE', #4870 ) ;
#29526 = ORIENTED_EDGE ( 'NONE', *, *, #11545, .F. ) ;
#29527 = FACE_OUTER_BOUND ( 'NONE', #1398, .T. ) ;
#29528 = CARTESIAN_POINT ( 'NONE',  ( -23.20948082139999968, -13.40000000000000036, 226.0999999999999943 ) ) ;
#29529 = CARTESIAN_POINT ( 'NONE',  ( -25.09216856445464927, -13.51511586023699785, 224.2647128708496211 ) ) ;
#29530 = AXIS2_PLACEMENT_3D ( 'NONE', #25556, #11227, #20833 ) ;
#29531 = B_SPLINE_CURVE_WITH_KNOTS ( 'NONE', 3,
 ( #18042, #10517, #3575, #13169, #22944, #27191, #30009, #5629, #15229, #926, #19440, #721, #17074, #2764, #29178, #12357, #10312, #24475 ),
 .UNSPECIFIED., .F., .F.,
 ( 4, 2, 2, 2, 2, 2, 2, 2, 4 ),
 ( 0.000000000000000000, 0.1250000000000000000, 0.2500000000000000000, 0.3750000000000000000, 0.5000000000000000000, 0.6250000000000000000, 0.7500000000000000000, 0.8750000000000000000, 1.000000000000000000 ),
 .UNSPECIFIED. ) ;
#29532 = CARTESIAN_POINT ( 'NONE',  ( 8.350000000354834029, -111.9817663810069774, 5.760339591729700004 ) ) ;
#29533 = B_SPLINE_CURVE_WITH_KNOTS ( 'NONE', 5,
 ( #22820, #5976, #18080, #813, #20298, #12911 ),
 .UNSPECIFIED., .F., .F.,
 ( 6, 6 ),
 ( 0.000000000000000000, 2.300779653469999797 ),
 .UNSPECIFIED. ) ;
#29534 = AXIS2_PLACEMENT_3D ( 'NONE', #2885, #21779, #21629 ) ;
#29535 = CARTESIAN_POINT ( 'NONE',  ( 24.83272649506304219, -12.49791454618707398, 5.208434320000010942 ) ) ;
#29536 = EDGE_CURVE ( 'NONE', #2944, #29946, #5693, .T. ) ;
#29537 = CARTESIAN_POINT ( 'NONE',  ( -2.299991308520000465E-10, 20.99999999999999645, -64.10000000000000853 ) ) ;
#29538 = ORIENTED_EDGE ( 'NONE', *, *, #22913, .T. ) ;
#29539 = CARTESIAN_POINT ( 'NONE',  ( 2.319980218398844940, -3.564287903756054199, -44.10000000002499831 ) ) ;
#29540 = CARTESIAN_POINT ( 'NONE',  ( -24.98081131316241255, -13.71897606304888662, 4.999998581000003384 ) ) ;
#29541 = CARTESIAN_POINT ( 'NONE',  ( 1.391539067366913018, -4.898323207587138128, -22.23285708920000658 ) ) ;
#29542 = CARTESIAN_POINT ( 'NONE',  ( -12.40641005330448898, -23.35436477320368454, -32.06844556927040912 ) ) ;
#29543 = CARTESIAN_POINT ( 'NONE',  ( -10.00000000000000000, 19.99999999999999645, -42.39999999999999858 ) ) ;
#29544 = CARTESIAN_POINT ( 'NONE',  ( 24.07552309629999954, -13.90001137829999855, 226.1000014189999945 ) ) ;
#29545 = CARTESIAN_POINT ( 'NONE',  ( -23.62704991831892798, -14.65035393207314840, 225.6826156241376111 ) ) ;
#29546 = CARTESIAN_POINT ( 'NONE',  ( -1.909971040720825908, -5.612411004515823088, -46.99520033292500187 ) ) ;
#29547 = VECTOR ( 'NONE', #12322, 1000.000000000000000 ) ;
#29548 = PLANE ( 'NONE',  #10710 ) ;
#29549 = CARTESIAN_POINT ( 'NONE',  ( 9.254368700311683682, -25.15168151593200818, 204.8447925225967481 ) ) ;
#29550 = CARTESIAN_POINT ( 'NONE',  ( -18.06506883821712961, 19.99992188150034877, 230.6935433854662847 ) ) ;
#29551 = CARTESIAN_POINT ( 'NONE',  ( -26.80000000069999899, 3.281945028329999726E-15, 43.21714158909999526 ) ) ;
#29552 = EDGE_CURVE ( 'NONE', #10592, #6458, #15357, .T. ) ;
#29553 = VECTOR ( 'NONE', #26905, 1000.000000000000000 ) ;
#29554 = CARTESIAN_POINT ( 'NONE',  ( 23.92402432494557729, -13.56054119037707117, 226.0877068033694002 ) ) ;
#29555 = ORIENTED_EDGE ( 'NONE', *, *, #7045, .T. ) ;
#29556 = CARTESIAN_POINT ( 'NONE',  ( -4.346598770676703083, -0.007247149673123010061, -28.16856466009999593 ) ) ;
#29557 = VECTOR ( 'NONE', #16190, 1000.000000000000000 ) ;
#29558 = ORIENTED_EDGE ( 'NONE', *, *, #10254, .T. ) ;
#29559 = FACE_OUTER_BOUND ( 'NONE', #11468, .T. ) ;
#29560 = CARTESIAN_POINT ( 'NONE',  ( -4.185672079393965461, 2.483218523716621107, -51.23267869292500620 ) ) ;
#29561 = ORIENTED_EDGE ( 'NONE', *, *, #29196, .F. ) ;
#29562 = EDGE_CURVE ( 'NONE', #16870, #20235, #16973, .T. ) ;
#29563 = EDGE_LOOP ( 'NONE', ( #6134, #17835, #5317, #27703 ) ) ;
#29564 = DIRECTION ( 'NONE',  ( -0.8660254037843286845, -0.5000000000001905143, 4.166995253231288982E-16 ) ) ;
#29565 = EDGE_LOOP ( 'NONE', ( #4915, #367, #28679, #8851 ) ) ;
#29566 = ORIENTED_EDGE ( 'NONE', *, *, #6199, .F. ) ;
#29567 = LINE ( 'NONE', #23087, #13041 ) ;
#29568 = CARTESIAN_POINT ( 'NONE',  ( -17.62053209685469923, -9.769114620074489608, 0.000000000000000000 ) ) ;
#29569 = DIRECTION ( 'NONE',  ( 1.000000000000000000, 0.000000000000000000, 0.000000000000000000 ) ) ;
#29570 = LINE ( 'NONE', #27508, #26508 ) ;
#29571 = AXIS2_PLACEMENT_3D ( 'NONE', #139, #4853, #26560 ) ;
#29572 = CARTESIAN_POINT ( 'NONE',  ( -12.52275726678476175, -27.79162686073846444, -23.08395539522074102 ) ) ;
#29573 = CARTESIAN_POINT ( 'NONE',  ( -3.810063518243186120, 1.754619919559086139, -0.6999999999999995115 ) ) ;
#29574 = CARTESIAN_POINT ( 'NONE',  ( 3.123710955063065509, -2.074832491810036039, 0.5412452697999986517 ) ) ;
#29575 = CARTESIAN_POINT ( 'NONE',  ( -24.00379068851701447, -14.02496465848369844, 223.9000014189999774 ) ) ;
#29576 = CARTESIAN_POINT ( 'NONE',  ( -10.00000000000000000, -13.30122639390952877, -75.84793558053411289 ) ) ;
#29577 = CARTESIAN_POINT ( 'NONE',  ( 2.618538529469167653, 3.470429992801025154, -14.72796858840001022 ) ) ;
#29578 = CARTESIAN_POINT ( 'NONE',  ( 3.503437880484523426, 2.636891074944038404, -31.86032172560000575 ) ) ;
#29579 = CARTESIAN_POINT ( 'NONE',  ( 1.484924240490000047, -1.484924240490000047, 226.6412452697800006 ) ) ;
#29580 = AXIS2_PLACEMENT_3D ( 'NONE', #10895, #22237, #20331 ) ;
#29581 = EDGE_CURVE ( 'NONE', #17360, #6881, #9725, .T. ) ;
#29582 = CARTESIAN_POINT ( 'NONE',  ( 16.40303402077768169, -9.791839085275103827, -0.6999999989999727834 ) ) ;
#29583 = CARTESIAN_POINT ( 'NONE',  ( -24.34628147195961390, -13.42155311436081355, 225.9641454712443078 ) ) ;
#29584 = CARTESIAN_POINT ( 'NONE',  ( -7.534632680830990026, -7.897185061638417380, -36.96526048005145526 ) ) ;
#29585 = CARTESIAN_POINT ( 'NONE',  ( 0.6521647005340001080, -27.79285400239999859, 225.9009072510000067 ) ) ;
#29586 = CARTESIAN_POINT ( 'NONE',  ( 3.746497173757565413, -0.1670055334890632737, -35.69999999999999574 ) ) ;
#29587 = CARTESIAN_POINT ( 'NONE',  ( -20.30403093128963476, 20.00000000003735323, 3.000000106999994642 ) ) ;
#29588 = B_SPLINE_CURVE_WITH_KNOTS ( 'NONE', 5,
 ( #20363, #27916, #27750, #27286, #6036, #6196, #22887, #25087, #29956, #13275, #17983, #24777 ),
 .UNSPECIFIED., .F., .F.,
 ( 6, 3, 3, 6 ),
 ( 0.000000000000000000, 1.359200785760000141, 2.718430693529999775, 3.788335907300000027 ),
 .UNSPECIFIED. ) ;
#29589 = CARTESIAN_POINT ( 'NONE',  ( 11.20000000009999930, -31.44000000000000128, -28.39999999989999679 ) ) ;
#29590 = PLANE ( 'NONE',  #28877 ) ;
#29591 = ORIENTED_EDGE ( 'NONE', *, *, #11703, .T. ) ;
#29592 = AXIS2_PLACEMENT_3D ( 'NONE', #17572, #20406, #15217 ) ;
#29593 = FACE_OUTER_BOUND ( 'NONE', #17792, .T. ) ;
#29594 = FACE_OUTER_BOUND ( 'NONE', #25824, .T. ) ;
#29595 = ORIENTED_EDGE ( 'NONE', *, *, #30961, .F. ) ;
#29596 = B_SPLINE_CURVE_WITH_KNOTS ( 'NONE', 3,
 ( #29193, #118, #7493, #16929, #5589, #15190 ),
 .UNSPECIFIED., .F., .F.,
 ( 4, 2, 4 ),
 ( 0.000000000000000000, 0.5000000000000000000, 1.000000000000000000 ),
 .UNSPECIFIED. ) ;
#29597 = LINE ( 'NONE', #20001, #22870 ) ;
#29598 = DIRECTION ( 'NONE',  ( -1.000000000000000000, 0.000000000000000000, 0.000000000000000000 ) ) ;
#29599 = ORIENTED_EDGE ( 'NONE', *, *, #28189, .F. ) ;
#29600 = DIRECTION ( 'NONE',  ( -2.764840495839172918E-12, -0.9128796883888953273, 0.4082287037029530552 ) ) ;
#29601 = ORIENTED_EDGE ( 'NONE', *, *, #7104, .F. ) ;
#29602 = EDGE_CURVE ( 'NONE', #2709, #28983, #25510, .T. ) ;
#29603 = EDGE_LOOP ( 'NONE', ( #28941, #22193, #5142, #7959 ) ) ;
#29604 =( NAMED_UNIT ( * ) PLANE_ANGLE_UNIT ( ) SI_UNIT ( $, .RADIAN. ) );
#29605 = VECTOR ( 'NONE', #2602, 1000.000000000000114 ) ;
#29606 = VERTEX_POINT ( 'NONE', #19653 ) ;
#29607 = CARTESIAN_POINT ( 'NONE',  ( 17.04201355691706610, -10.10244847084225484, 0.000000000000000000 ) ) ;
#29608 = AXIS2_PLACEMENT_3D ( 'NONE', #11969, #11821, #16533 ) ;
#29609 = CARTESIAN_POINT ( 'NONE',  ( 16.27441336928229276, -8.340546694414939566, -0.6999999999999783062 ) ) ;
#29610 = VERTEX_POINT ( 'NONE', #29235 ) ;
#29611 = CARTESIAN_POINT ( 'NONE',  ( -24.95427444319612675, 13.76797446832583560, 6.099998581000020792 ) ) ;
#29612 = CARTESIAN_POINT ( 'NONE',  ( -23.81866442513004856, -14.33570206453694240, 6.099998581000020792 ) ) ;
#29613 = DIRECTION ( 'NONE',  ( -0.7071067811865469066, -0.6644630243886066046, -0.2418447626481643187 ) ) ;
#29614 = CARTESIAN_POINT ( 'NONE',  ( -7.999999999656092875, -13.57196071827068096, -36.34117526632622486 ) ) ;
#29615 = EDGE_CURVE ( 'NONE', #27542, #13694, #21388, .T. ) ;
#29616 = ORIENTED_EDGE ( 'NONE', *, *, #21380, .T. ) ;
#29617 = EDGE_CURVE ( 'NONE', #6309, #21418, #9718, .T. ) ;
#29618 = CARTESIAN_POINT ( 'NONE',  ( 1.213582369797461258, 4.521795443253901148, -2.053410702900000828 ) ) ;
#29619 = CARTESIAN_POINT ( 'NONE',  ( 4.354753084053725409, 0.1085053810021691101, -20.67661200060000226 ) ) ;
#29620 = CARTESIAN_POINT ( 'NONE',  ( -24.08872333959828893, -11.87645233066224826, 193.2171415879999756 ) ) ;
#29621 = CARTESIAN_POINT ( 'NONE',  ( 6.150013584267105315, 4.806477681428259707, -43.16125079399513709 ) ) ;
#29622 = CARTESIAN_POINT ( 'NONE',  ( 0.000000000000000000, 21.70000000000000284, -44.10000000017312516 ) ) ;
#29623 = CARTESIAN_POINT ( 'NONE',  ( -7.861312627756137594, -6.255048793414832886, -36.09728094221726025 ) ) ;
#29624 = LINE ( 'NONE', #6011, #26861 ) ;
#29625 =( GEOMETRIC_REPRESENTATION_CONTEXT ( 3 ) GLOBAL_UNCERTAINTY_ASSIGNED_CONTEXT ( ( #16304 ) ) GLOBAL_UNIT_ASSIGNED_CONTEXT ( ( #1680, #3880, #20717 ) ) REPRESENTATION_CONTEXT ( 'NONE', 'WORKASPACE' ) );
#29626 = ADVANCED_FACE ( 'NONE', ( #20259, #30010, #27193 ), #10364, .T. ) ;
#29627 = CIRCLE ( 'NONE', #22091, 26.80000000000000071 ) ;
#29628 = CARTESIAN_POINT ( 'NONE',  ( -0.8926240818011654810, 3.415131430766678022, -0.6999999999999784173 ) ) ;
#29629 = CARTESIAN_POINT ( 'NONE',  ( -27.69999999930000101, 3.392159599999999562E-15, 190.0000000000000000 ) ) ;
#29630 = DIRECTION ( 'NONE',  ( 4.250489863290715314E-14, 6.005940811918195789E-13, 1.000000000000000000 ) ) ;
#29631 = ORIENTED_EDGE ( 'NONE', *, *, #28276, .F. ) ;
#29632 = CARTESIAN_POINT ( 'NONE',  ( -1.650988191866306742, 3.989749455477753504, -57.14652090042499566 ) ) ;
#29633 = CARTESIAN_POINT ( 'NONE',  ( -19.29999999990000248, -26.99999999999986144, -28.39999999990009272 ) ) ;
#29634 = B_SPLINE_CURVE_WITH_KNOTS ( 'NONE', 3,
 ( #5265, #24468, #2902, #22106, #13592, #11079 ),
 .UNSPECIFIED., .F., .F.,
 ( 4, 2, 4 ),
 ( 0.000000000000000000, 0.4999999999999975575, 1.000000000000000000 ),
 .UNSPECIFIED. ) ;
#29635 = CARTESIAN_POINT ( 'NONE',  ( -4.101794773665658589, 5.071170285168458136, -13.60352819870000474 ) ) ;
#29636 = CLOSED_SHELL ( 'NONE', ( #26454, #30344, #20507, #41, #17860, #14861, #29626, #6224, #11695, #26902, #14069, #10829, #18520, #17260, #28691, #15755, #26327, #16731, #19031, #15028, #2551, #16330, #18919, #31076, #613, #29216, #30653, #30281, #27850, #11397, #12196, #10461, #13280, #6272, #26000, #28027, #18306, #15916, #4283, #323, #19710, #12476, #12198, #18217, #16098, #2438, #24965, #28147, #15949, #3700, #10469, #10792, #15805, #12581, #28001, #11216, #4334, #25967, #27042, #27256, #19136, #9788, #28377, #27656, #5220, #22786, #6102, #16513, #30248, #24390, #22322, #28266, #24005, #23045, #29841, #27947, #24198, #676, #1957, #9433, #14311, #9618, #26625, #5281, #7901, #27190, #8130, #7905, #23551, #9057, #28283, #3249, #25854, #10263, #10861, #27143, #29996, #10228, #10321, #4780, #16941, #20383, #23257, #12341, #10567, #7920, #12941, #727, #13076, #15245, #9228, #11582, #14911, #22507, #11130, #4862, #7632, #21735, #2020, #19974, #25172, #13151, #13736, #6681, #15598, #18408, #19647, #18119, #17136, #10299, #29440, #1271, #5561, #26553, #19583, #3638, #4822, #8027, #23646, #30183, #25390, #17518, #17282 ) ) ;
#29637 = CARTESIAN_POINT ( 'NONE',  ( -27.85782817081202012, 2.925281790394680836, 8.000000000000007105 ) ) ;
#29638 = EDGE_CURVE ( 'NONE', #24321, #20581, #30348, .T. ) ;
#29639 = CARTESIAN_POINT ( 'NONE',  ( -4.403294653383551527, 1.129803870268460075, -68.10000000002499121 ) ) ;
#29640 = ORIENTED_EDGE ( 'NONE', *, *, #20435, .T. ) ;
#29641 = ORIENTED_EDGE ( 'NONE', *, *, #12979, .T. ) ;
#29642 = FACE_OUTER_BOUND ( 'NONE', #10402, .T. ) ;
#29643 =( LENGTH_UNIT ( ) NAMED_UNIT ( * ) SI_UNIT ( .MILLI., .METRE. ) );
#29644 = EDGE_LOOP ( 'NONE', ( #7119, #25288, #25074, #22218, #16614, #19349, #19868, #12923 ) ) ;
#29645 = PLANE ( 'NONE',  #12958 ) ;
#29646 = CARTESIAN_POINT ( 'NONE',  ( 23.62421573330318836, 14.65442405561991634, 6.042470792000015578 ) ) ;
#29647 = CARTESIAN_POINT ( 'NONE',  ( 4.883349601227579662, 0.1168011502185895972, -63.66686508972499325 ) ) ;
#29648 = EDGE_CURVE ( 'NONE', #23341, #21601, #13747, .T. ) ;
#29649 = CARTESIAN_POINT ( 'NONE',  ( -27.50000000000000000, 3.367667473009999970E-15, 0.000000000000000000 ) ) ;
#29650 = CARTESIAN_POINT ( 'NONE',  ( -28.44355746342733227, 4.375812428242645602, 0.2374258030000131470 ) ) ;
#29651 = DIRECTION ( 'NONE',  ( 0.000000000000000000, 0.000000000000000000, 1.000000000000000000 ) ) ;
#29652 = LINE ( 'NONE', #22113, #6034 ) ;
#29653 = FACE_BOUND ( 'NONE', #23350, .T. ) ;
#29654 = VERTEX_POINT ( 'NONE', #27039 ) ;
#29655 = CARTESIAN_POINT ( 'NONE',  ( 16.47468026044998268, -8.132810122024002553, -4.336808689942017736E-16 ) ) ;
#29656 = B_SPLINE_CURVE_WITH_KNOTS ( 'NONE', 3,
 ( #7370, #21226, #24205, #13997 ),
 .UNSPECIFIED., .F., .F.,
 ( 4, 4 ),
 ( 0.000000000000000000, 1.000000000000000000 ),
 .UNSPECIFIED. ) ;
#29657 = CARTESIAN_POINT ( 'NONE',  ( -3.552713678799999608E-15, 0.000000000000000000, 43.21714158840000408 ) ) ;
#29658 = ORIENTED_EDGE ( 'NONE', *, *, #20299, .T. ) ;
#29659 = CARTESIAN_POINT ( 'NONE',  ( 3.503090509817559539, 0.9324612816629570533, 227.7184664424436846 ) ) ;
#29660 = CARTESIAN_POINT ( 'NONE',  ( -22.73383167079628819, -14.19258501544933004, 4.402070809670797225 ) ) ;
#29661 = CARTESIAN_POINT ( 'NONE',  ( 0.000000000000000000, 0.000000000000000000, 229.2412452700000074 ) ) ;
#29662 = CARTESIAN_POINT ( 'NONE',  ( -24.29748893039695545, -13.50839063705114995, 4.437671896236813573 ) ) ;
#29663 = CARTESIAN_POINT ( 'NONE',  ( -23.26185891380717763, -14.66761890373121524, 4.713248588340865020 ) ) ;
#29664 = AXIS2_PLACEMENT_3D ( 'NONE', #23277, #1721, #20917 ) ;
#29665 = CARTESIAN_POINT ( 'NONE',  ( 3.215880358400865280, -2.702085720338708974, -0.6999999999999992895 ) ) ;
#29666 = CARTESIAN_POINT ( 'NONE',  ( -28.35455043824866550, -0.5159221438580923191, 0.2374258030000131470 ) ) ;
#29667 = CARTESIAN_POINT ( 'NONE',  ( 27.50000000000000000, -3.367667472999999580E-15, 143.2809019210000088 ) ) ;
#29668 = ORIENTED_EDGE ( 'NONE', *, *, #6169, .T. ) ;
#29669 = CARTESIAN_POINT ( 'NONE',  ( 24.39135169767337885, -14.74223403355047068, 4.689353541000001790 ) ) ;
#29670 = CARTESIAN_POINT ( 'NONE',  ( 14.09657531829999932, 28.30410039250000054, 229.0000000000000000 ) ) ;
#29671 = CARTESIAN_POINT ( 'NONE',  ( -5.852082250035282485, -26.15431190117149995, 21.03698545514888707 ) ) ;
#29672 = DIRECTION ( 'NONE',  ( 0.000000000000000000, 0.000000000000000000, -1.000000000000000000 ) ) ;
#29673 = ADVANCED_FACE ( 'NONE', ( #10984 ), #3113, .F. ) ;
#29674 = ORIENTED_EDGE ( 'NONE', *, *, #7138, .T. ) ;
#29675 = CARTESIAN_POINT ( 'NONE',  ( 11.37440860439999923, -24.37257236010000128, -1.450121496399996213 ) ) ;
#29676 = EDGE_CURVE ( 'NONE', #17407, #553, #28122, .T. ) ;
#29677 = SURFACE_SIDE_STYLE ('',( #25269 ) ) ;
#29678 = CARTESIAN_POINT ( 'NONE',  ( 14.80403571755166148, -23.72938950558570781, -32.28486879153918210 ) ) ;
#29679 = CARTESIAN_POINT ( 'NONE',  ( 3.750246723960807049, 0.6078790020706823505, -41.11345739176283587 ) ) ;
#29680 = B_SPLINE_CURVE_WITH_KNOTS ( 'NONE', 3,
 ( #11795, #20930, #21401, #16201, #30991, #30533, #9423, #28628, #25498, #28162, #25814, #4253 ),
 .UNSPECIFIED., .F., .F.,
 ( 4, 2, 2, 2, 2, 4 ),
 ( 0.000000000000000000, 0.2499999999999983347, 0.3749999999999973355, 0.4999999999999963363, 0.7499999999999981126, 1.000000000000000000 ),
 .UNSPECIFIED. ) ;
#29681 = CARTESIAN_POINT ( 'NONE',  ( 1.094823181362614140, 5.872682718251108547, -63.90744533522500603 ) ) ;
#29682 = VERTEX_POINT ( 'NONE', #25141 ) ;
#29683 = ORIENTED_EDGE ( 'NONE', *, *, #5213, .F. ) ;
#29684 = CARTESIAN_POINT ( 'NONE',  ( 27.71261514784112379, 0.5042418800004094814, 0.5514269430000329208 ) ) ;
#29685 = ORIENTED_EDGE ( 'NONE', *, *, #26573, .F. ) ;
#29686 = EDGE_LOOP ( 'NONE', ( #7720, #686, #28818, #23404 ) ) ;
#29687 = CARTESIAN_POINT ( 'NONE',  ( -10.46446609379999870, 21.70000000000000284, -54.63553390589999736 ) ) ;
#29688 = CARTESIAN_POINT ( 'NONE',  ( 25.32653163311281830, -13.07087917458821202, 4.239730452999995514 ) ) ;
#29689 = CARTESIAN_POINT ( 'NONE',  ( -22.90527192528401201, 16.36193184990112570, 8.000000000000007105 ) ) ;
#29690 = CARTESIAN_POINT ( 'NONE',  ( -17.35782682096630225, -25.84383608289461520, -33.50599114333153494 ) ) ;
#29691 = APPLICATION_CONTEXT ( 'automotive_design' ) ;
#29692 = CARTESIAN_POINT ( 'NONE',  ( 24.37165445055180157, -14.77472140295711434, 4.999998581000003384 ) ) ;
#29693 = CARTESIAN_POINT ( 'NONE',  ( 16.37473331889771089, 11.76353838340827984, -0.6999999989999727834 ) ) ;
#29694 = VERTEX_POINT ( 'NONE', #29855 ) ;
#29695 = CARTESIAN_POINT ( 'NONE',  ( 1.984258505993609978, -3.678877725158681944, -44.10000000002499831 ) ) ;
#29696 = CARTESIAN_POINT ( 'NONE',  ( 24.41841038956698640, 14.69667349781389376, 3.899998581000013509 ) ) ;
#29697 = VECTOR ( 'NONE', #23787, 1000.000000000000000 ) ;
#29698 = CARTESIAN_POINT ( 'NONE',  ( -1.961220842236323536, 4.382205557898919857, -23.67530126170000315 ) ) ;
#29699 = CARTESIAN_POINT ( 'NONE',  ( 28.49528339128749366, 0.5184828350247886464, 8.000000000000007105 ) ) ;
#29700 = DIRECTION ( 'NONE',  ( 0.000000000000000000, 0.000000000000000000, 1.000000000000000000 ) ) ;
#29701 = DIRECTION ( 'NONE',  ( 0.000000000000000000, 0.000000000000000000, 1.000000000000000000 ) ) ;
#29702 = DIRECTION ( 'NONE',  ( 1.000000000000000000, 0.000000000000000000, -0.000000000000000000 ) ) ;
#29703 = CARTESIAN_POINT ( 'NONE',  ( -0.5560430376289927645, 4.887756486939889733, -47.51410749632499630 ) ) ;
#29704 = CARTESIAN_POINT ( 'NONE',  ( -4.299999999899999814, -27.00000000000000000, -28.39999999989999679 ) ) ;
#29705 = CARTESIAN_POINT ( 'NONE',  ( 3.931979172340990036, -26.51120696000497645, 209.7426969702732720 ) ) ;
#29706 = DIRECTION ( 'NONE',  ( -1.000000000000000000, 0.000000000000000000, -2.257144471330000330E-12 ) ) ;
#29707 = CARTESIAN_POINT ( 'NONE',  ( -22.81399828927099094, -14.09994392937124985, 43.21714158846111786 ) ) ;
#29708 = EDGE_CURVE ( 'NONE', #3758, #28478, #2596, .T. ) ;
#29709 = CARTESIAN_POINT ( 'NONE',  ( 6.438687372225744276, -8.560122214837054599, -36.64192442626541890 ) ) ;
#29710 = ORIENTED_EDGE ( 'NONE', *, *, #21840, .F. ) ;
#29711 = CARTESIAN_POINT ( 'NONE',  ( -3.554763430470067043, 2.566410659217312151, -34.96696136359999940 ) ) ;
#29712 = EDGE_CURVE ( 'NONE', #22582, #30573, #8443, .T. ) ;
#29713 = ORIENTED_EDGE ( 'NONE', *, *, #12886, .T. ) ;
#29714 = LINE ( 'NONE', #24687, #11261 ) ;
#29715 = CARTESIAN_POINT ( 'NONE',  ( 4.545032752014871669, -0.3361547907463971474, -49.12442242802499237 ) ) ;
#29716 = VERTEX_POINT ( 'NONE', #22945 ) ;
#29717 = ORIENTED_EDGE ( 'NONE', *, *, #12770, .T. ) ;
#29718 = DIRECTION ( 'NONE',  ( 0.000000000000000000, 0.000000000000000000, 1.000000000000000000 ) ) ;
#29719 = VECTOR ( 'NONE', #14965, 1000.000000000000000 ) ;
#29720 = EDGE_LOOP ( 'NONE', ( #27862, #1428, #15523, #24266, #6494 ) ) ;
#29721 = ORIENTED_EDGE ( 'NONE', *, *, #4535, .T. ) ;
#29722 = CARTESIAN_POINT ( 'NONE',  ( 23.87170004953230773, 14.24726900334573187, 3.904031772999999816 ) ) ;
#29723 = CARTESIAN_POINT ( 'NONE',  ( 9.897162125400447152, -25.37356426577149549, 88.33953982530000815 ) ) ;
#29724 = CARTESIAN_POINT ( 'NONE',  ( -13.12132034329999897, 21.69999999990000106, -69.22132034359999864 ) ) ;
#29725 = DIRECTION ( 'NONE',  ( -1.000000000000000000, 1.224606353819999829E-16, 0.000000000000000000 ) ) ;
#29726 = CARTESIAN_POINT ( 'NONE',  ( 13.00000000000000000, 24.88415091498285747, -60.88541708338509295 ) ) ;
#29727 = CARTESIAN_POINT ( 'NONE',  ( -4.035443471795205461, 2.350095507017441410, -0.6999999999999992895 ) ) ;
#29728 = DIRECTION ( 'NONE',  ( 5.962915006522622422E-16, 0.4383711467890810676, 0.8987940462991651502 ) ) ;
#29729 = LINE ( 'NONE', #1096, #15004 ) ;
#29730 = CARTESIAN_POINT ( 'NONE',  ( 9.993285220779513978, -25.61999708228223227, 143.6055512739999926 ) ) ;
#29731 = B_SPLINE_CURVE_WITH_KNOTS ( 'NONE', 3,
 ( #27109, #22396, #22695, #3642, #3333, #5543, #17352, #12942, #25209, #1301 ),
 .UNSPECIFIED., .F., .F.,
 ( 4, 2, 2, 2, 4 ),
 ( 0.000000000000000000, 0.2500000000000000000, 0.5000000000000000000, 0.7500000000000000000, 1.000000000000000000 ),
 .UNSPECIFIED. ) ;
#29732 = CARTESIAN_POINT ( 'NONE',  ( -5.517889265940039145, -2.627421812126006451, -12.97655742010000246 ) ) ;
#29733 = CARTESIAN_POINT ( 'NONE',  ( -2.705882613314523955, 5.963358562559473164, -31.12635571289999703 ) ) ;
#29734 = CARTESIAN_POINT ( 'NONE',  ( 0.000000000000000000, 0.000000000000000000, 115.0000000000000000 ) ) ;
#29735 = CARTESIAN_POINT ( 'NONE',  ( -17.59696554489119080, -9.791838634853515799, 0.000000000000000000 ) ) ;
#29736 = CARTESIAN_POINT ( 'NONE',  ( 10.00000000070000183, -27.00000000000000000, -25.39999999999999858 ) ) ;
#29737 = CARTESIAN_POINT ( 'NONE',  ( -8.699999998977590465, -24.26136093481122558, -29.62468611113576955 ) ) ;
#29738 = CYLINDRICAL_SURFACE ( 'NONE', #16814, 26.80000000000000071 ) ;
#29739 = EDGE_CURVE ( 'NONE', #1536, #11539, #15739, .T. ) ;
#29740 = CIRCLE ( 'NONE', #30236, 26.80000000000000071 ) ;
#29741 = CARTESIAN_POINT ( 'NONE',  ( 21.13530760622606763, 17.06006193239099034, -0.6999999999999784173 ) ) ;
#29742 = CARTESIAN_POINT ( 'NONE',  ( 17.16657240420000008, 10.97998838177520931, -1.452769935612311825 ) ) ;
#29743 = CARTESIAN_POINT ( 'NONE',  ( 23.55411374389282386, 16.04538543799059980, 8.000000000000007105 ) ) ;
#29744 = ORIENTED_EDGE ( 'NONE', *, *, #6705, .F. ) ;
#29745 = CARTESIAN_POINT ( 'NONE',  ( -8.349999999680450813, -115.5267901938268977, 21.04701627019373333 ) ) ;
#29746 = CARTESIAN_POINT ( 'NONE',  ( 2.748065355789120812, 2.239845275076990827, 230.8106057538952598 ) ) ;
#29747 = ORIENTED_EDGE ( 'NONE', *, *, #29825, .T. ) ;
#29748 = CARTESIAN_POINT ( 'NONE',  ( -19.80526744909999692, 19.50877353739999975, 229.0000000010000178 ) ) ;
#29749 = CARTESIAN_POINT ( 'NONE',  ( 17.83929309184204826, 20.00000000005427125, -0.3499999999999892086 ) ) ;
#29750 = ORIENTED_EDGE ( 'NONE', *, *, #11351, .F. ) ;
#29751 = CARTESIAN_POINT ( 'NONE',  ( -0.8784922619252688580, -26.78562592415266153, 4.333924731881555026 ) ) ;
#29752 = ORIENTED_EDGE ( 'NONE', *, *, #12946, .F. ) ;
#29753 = ORIENTED_EDGE ( 'NONE', *, *, #23158, .T. ) ;
#29754 = ORIENTED_EDGE ( 'NONE', *, *, #29552, .T. ) ;
#29755 = CARTESIAN_POINT ( 'NONE',  ( 28.50000000000000000, 3.197442310919999608E-14, 229.0000000000000000 ) ) ;
#29756 = LINE ( 'NONE', #12612, #2108 ) ;
#29757 = CARTESIAN_POINT ( 'NONE',  ( -3.510330247560000227, -1.917702154400000136, -44.00000000037249492 ) ) ;
#29758 = ORIENTED_EDGE ( 'NONE', *, *, #3517, .T. ) ;
#29759 = LINE ( 'NONE', #3171, #2876 ) ;
#29760 = PRODUCT_DEFINITION_SHAPE ( 'NONE', 'NONE',  #31128 ) ;
#29761 = CARTESIAN_POINT ( 'NONE',  ( -0.3076636919214117971, -28.49867017228250177, 5.759626916000016195 ) ) ;
#29762 = CARTESIAN_POINT ( 'NONE',  ( -17.49999999969999820, -29.39114981890000067, -32.77697038446999755 ) ) ;
#29763 = CARTESIAN_POINT ( 'NONE',  ( -11.00000000000000000, 26.42151601322854759, -59.26168417594741555 ) ) ;
#29764 = EDGE_CURVE ( 'NONE', #18684, #7240, #18370, .T. ) ;
#29765 = CARTESIAN_POINT ( 'NONE',  ( -1.763726019828893321, -5.203278105301040846, -1.575630512700004537 ) ) ;
#29766 = CARTESIAN_POINT ( 'NONE',  ( -2.322678811625146444, -3.635533071076381795, -21.20891267860001150 ) ) ;
#29767 = CARTESIAN_POINT ( 'NONE',  ( -4.130757957910000097E-10, -1.288485762530000039E-09, 230.0000000000000000 ) ) ;
#29768 = AXIS2_PLACEMENT_3D ( 'NONE', #27463, #25270, #13460 ) ;
#29769 = CARTESIAN_POINT ( 'NONE',  ( 16.37473331889771089, 11.76353838340827984, 0.000000000000000000 ) ) ;
#29770 = CARTESIAN_POINT ( 'NONE',  ( -2.172877275949271159, -3.409783563088108149, -92.08560516904439908 ) ) ;
#29771 = CARTESIAN_POINT ( 'NONE',  ( -17.99934820270000202, 20.17941515389999907, 230.6999999999999886 ) ) ;
#29772 = LINE ( 'NONE', #3336, #731 ) ;
#29773 = EDGE_CURVE ( 'NONE', #18419, #29716, #11235, .T. ) ;
#29774 = CARTESIAN_POINT ( 'NONE',  ( -13.75032424529999986, -27.60893268180000248, 229.0000000000000000 ) ) ;
#29775 = CARTESIAN_POINT ( 'NONE',  ( 9.987902756569999596, 15.20391984080000114, 230.6999999999999886 ) ) ;
#29776 = CARTESIAN_POINT ( 'NONE',  ( 9.999999999770000869, 21.35000000040000145, -60.10000000000000142 ) ) ;
#29777 = VERTEX_POINT ( 'NONE', #2167 ) ;
#29778 = CARTESIAN_POINT ( 'NONE',  ( -4.072259770650996202, 2.021700601780457962, -56.39877225282500461 ) ) ;
#29779 = VECTOR ( 'NONE', #9345, 1000.000000000000114 ) ;
#29780 = DIRECTION ( 'NONE',  ( 0.000000000000000000, 0.000000000000000000, -1.000000000000000000 ) ) ;
#29781 = CARTESIAN_POINT ( 'NONE',  ( 3.530284718056032833, 5.524446756132658898, -5.200967428500000267 ) ) ;
#29782 = EDGE_LOOP ( 'NONE', ( #17969, #15282, #3017, #17921 ) ) ;
#29783 = CARTESIAN_POINT ( 'NONE',  ( -0.9048562442035532616, 4.261764438836468827, -39.55777057273417086 ) ) ;
#29784 = CARTESIAN_POINT ( 'NONE',  ( -4.195251052989737772, 0.4538500998018956123, -68.10000000002501963 ) ) ;
#29785 = EDGE_CURVE ( 'NONE', #18702, #19859, #16861, .T. ) ;
#29786 = ORIENTED_EDGE ( 'NONE', *, *, #2695, .F. ) ;
#29787 = ORIENTED_EDGE ( 'NONE', *, *, #22457, .F. ) ;
#29788 = CARTESIAN_POINT ( 'NONE',  ( 2.741849580885529658, 1.023520720862898248, -95.04696119083976669 ) ) ;
#29789 = B_SPLINE_CURVE_WITH_KNOTS ( 'NONE', 3,
 ( #1573, #27516, #15556, #25166, #25325, #6118 ),
 .UNSPECIFIED., .F., .F.,
 ( 4, 2, 4 ),
 ( 0.000000000000000000, 0.5000000000000000000, 1.000000000000000000 ),
 .UNSPECIFIED. ) ;
#29790 = ORIENTED_EDGE ( 'NONE', *, *, #12310, .F. ) ;
#29791 = CARTESIAN_POINT ( 'NONE',  ( -24.81746041937532965, 14.01353061208509310, 3.920132063000014710 ) ) ;
#29792 = FACE_OUTER_BOUND ( 'NONE', #17899, .T. ) ;
#29793 = CARTESIAN_POINT ( 'NONE',  ( -3.807105672873282831, -5.136256491778199873, -65.13409070562501313 ) ) ;
#29794 = CARTESIAN_POINT ( 'NONE',  ( -26.94142135619999934, -9.898318926829999143, 230.0000000000000000 ) ) ;
#29795 = CARTESIAN_POINT ( 'NONE',  ( -22.59122543795706051, 17.98290286765915980, 0.5017677510000262409 ) ) ;
#29796 = CARTESIAN_POINT ( 'NONE',  ( -27.72015578919999967, -7.265888686289999399, 222.0000000000000000 ) ) ;
#29797 = AXIS2_PLACEMENT_3D ( 'NONE', #10155, #262, #7780 ) ;
#29798 = CARTESIAN_POINT ( 'NONE',  ( -25.41286868644903763, 12.90211872717319430, 4.492873454000012146 ) ) ;
#29799 = ORIENTED_EDGE ( 'NONE', *, *, #5870, .F. ) ;
#29800 = PRODUCT_DEFINITION_CONTEXT ( 'detailed design', #22038, 'design' ) ;
#29801 = B_SPLINE_CURVE_WITH_KNOTS ( 'NONE', 5,
 ( #5591, #22130, #29195, #21980, #24798, #24643, #22282, #29511, #19771, #739, #10629, #436 ),
 .UNSPECIFIED., .F., .F.,
 ( 6, 3, 3, 6 ),
 ( 2.782752055940000080, 3.293393369179999919, 4.940089939870000002, 5.565010778459999585 ),
 .UNSPECIFIED. ) ;
#29802 = CARTESIAN_POINT ( 'NONE',  ( 0.2892544189978767388, -26.79878419700509085, 6.071490516278870153 ) ) ;
#29803 = PLANE ( 'NONE',  #4982 ) ;
#29804 = ORIENTED_EDGE ( 'NONE', *, *, #16999, .T. ) ;
#29805 = CARTESIAN_POINT ( 'NONE',  ( 25.17364887440000132, -13.36205984489999921, 224.4930265309999982 ) ) ;
#29806 = CARTESIAN_POINT ( 'NONE',  ( 17.14656078602323319, -7.900182044548062166, -0.6999999999999784173 ) ) ;
#29807 = CARTESIAN_POINT ( 'NONE',  ( -16.85343921394901301, 12.09981795542885585, -0.6999999999999784173 ) ) ;
#29808 = EDGE_CURVE ( 'NONE', #26986, #15618, #20252, .T. ) ;
#29809 = CARTESIAN_POINT ( 'NONE',  ( 24.08512461539509175, 13.58911351521636490, 0.02487527300001901587 ) ) ;
#29810 = DIRECTION ( 'NONE',  ( 2.764802276011834339E-12, 0.9128796883888953273, -0.4082287037029531107 ) ) ;
#29811 = CARTESIAN_POINT ( 'NONE',  ( 3.514399168375105909, -2.498675756239369328, -0.6999999999999992895 ) ) ;
#29812 = CARTESIAN_POINT ( 'NONE',  ( -10.79767709090000061, -24.52928868880000124, -0.9448358073000027169 ) ) ;
#29813 = CARTESIAN_POINT ( 'NONE',  ( -9.999999999559999964, 21.70000000000000284, -60.10000000000000142 ) ) ;
#29814 = ORIENTED_EDGE ( 'NONE', *, *, #16373, .F. ) ;
#29815 = FACE_OUTER_BOUND ( 'NONE', #27498, .T. ) ;
#29816 = CARTESIAN_POINT ( 'NONE',  ( -21.16705332919999805, 21.30254446269999846, 229.0000000000000000 ) ) ;
#29817 = TOROIDAL_SURFACE ( 'NONE', #7206, 24.50000000000000000, 4.000000000000000000 ) ;
#29818 = AXIS2_PLACEMENT_3D ( 'NONE', #7952, #24956, #22604 ) ;
#29819 = CARTESIAN_POINT ( 'NONE',  ( -24.76914019444433279, -10.23375669952358358, 93.21714158839957065 ) ) ;
#29820 = CARTESIAN_POINT ( 'NONE',  ( -0.5944614571882205212, -27.79380703160649446, 5.104049977999985721 ) ) ;
#29821 = EDGE_CURVE ( 'NONE', #13982, #22703, #23848, .T. ) ;
#29822 = DIRECTION ( 'NONE',  ( -0.000000000000000000, 1.000000000000000000, -2.257145581549999994E-12 ) ) ;
#29823 = DIRECTION ( 'NONE',  ( -0.7071067811865475727, 0.7071067811865475727, 0.000000000000000000 ) ) ;
#29824 = CARTESIAN_POINT ( 'NONE',  ( -0.1113126277073495929, 2.989789856717120387, -42.27519293863267791 ) ) ;
#29825 = EDGE_CURVE ( 'NONE', #9526, #25596, #19882, .T. ) ;
#29826 = CARTESIAN_POINT ( 'NONE',  ( 4.508719565894415915, 1.847421675581904843, -60.89141554682500157 ) ) ;
#29827 = ORIENTED_EDGE ( 'NONE', *, *, #11639, .T. ) ;
#29828 = CARTESIAN_POINT ( 'NONE',  ( 18.31380613830149073, 20.00001766699981331, 230.6700634801132992 ) ) ;
#29829 = EDGE_CURVE ( 'NONE', #7420, #21140, #25111, .T. ) ;
#29830 = ORIENTED_EDGE ( 'NONE', *, *, #17231, .T. ) ;
#29831 = CARTESIAN_POINT ( 'NONE',  ( -4.667733413579616908, -30.93201666723582122, 1.000000002999990034 ) ) ;
#29832 = ORIENTED_EDGE ( 'NONE', *, *, #1050, .T. ) ;
#29833 = AXIS2_PLACEMENT_3D ( 'NONE', #2888, #22243, #9978 ) ;
#29834 = CIRCLE ( 'NONE', #20290, 3.200000000000002398 ) ;
#29835 = FACE_OUTER_BOUND ( 'NONE', #18613, .T. ) ;
#29836 = CIRCLE ( 'NONE', #24840, 28.50000000000000000 ) ;
#29837 = CARTESIAN_POINT ( 'NONE',  ( -12.30000000003916938, -24.07808196999506123, -29.18524365327784409 ) ) ;
#29838 = CARTESIAN_POINT ( 'NONE',  ( -19.80535357367646654, 19.50875577052770993, 6.600000000000022737 ) ) ;
#29839 = AXIS2_PLACEMENT_3D ( 'NONE', #5118, #12362, #7633 ) ;
#29840 = CARTESIAN_POINT ( 'NONE',  ( -8.699999999718343702, -24.19750589173278499, -27.32947359979484858 ) ) ;
#29841 = ADVANCED_FACE ( 'NONE', ( #6564 ), #18676, .T. ) ;
#29842 = CARTESIAN_POINT ( 'NONE',  ( 25.05552768372066907, -13.58331698798256504, 6.079865069000017996 ) ) ;
#29843 = DIRECTION ( 'NONE',  ( -1.595945597898660305E-12, 0.7071067811865475727, 0.7071067811865475727 ) ) ;
#29844 = ORIENTED_EDGE ( 'NONE', *, *, #23592, .T. ) ;
#29845 = CARTESIAN_POINT ( 'NONE',  ( 1.894269134907880847, -4.501889487458040406, -44.10000000002499121 ) ) ;
#29846 = CARTESIAN_POINT ( 'NONE',  ( 27.50000000000000000, -3.367667472999999580E-15, 136.7190980919999959 ) ) ;
#29847 = EDGE_CURVE ( 'NONE', #25327, #3809, #28512, .T. ) ;
#29848 = CARTESIAN_POINT ( 'NONE',  ( 3.713067847428462631, -3.043557113396612390, -24.93424734059999537 ) ) ;
#29849 = CARTESIAN_POINT ( 'NONE',  ( 27.77990052945810362, 1.357541147587897568, 8.000000000000007105 ) ) ;
#29850 = CARTESIAN_POINT ( 'NONE',  ( 0.000000000000000000, 27.10555629988041204, -61.14106941751904856 ) ) ;
#29851 = CARTESIAN_POINT ( 'NONE',  ( -23.53828869184600592, -14.79220260103408968, 225.3595846784022569 ) ) ;
#29852 = CARTESIAN_POINT ( 'NONE',  ( 5.200437648300224147, 1.853818095060352222, -45.12627377572500365 ) ) ;
#29853 = EDGE_CURVE ( 'NONE', #27919, #2249, #4366, .T. ) ;
#29854 = DIRECTION ( 'NONE',  ( 1.000000000000000000, 0.000000000000000000, 0.000000000000000000 ) ) ;
#29855 = CARTESIAN_POINT ( 'NONE',  ( 8.700000000278096834, -14.92844969908683517, -33.25053330388887218 ) ) ;
#29856 = CARTESIAN_POINT ( 'NONE',  ( -18.19349109261828090, 19.99999252024461072, 230.6834197065497563 ) ) ;
#29857 = CARTESIAN_POINT ( 'NONE',  ( -25.04491701902129819, -9.543388590360489587, 43.21714158838634745 ) ) ;
#29858 = VECTOR ( 'NONE', #21636, 1000.000000000000000 ) ;
#29859 = AXIS2_PLACEMENT_3D ( 'NONE', #11536, #17968, #15622 ) ;
#29860 = CARTESIAN_POINT ( 'NONE',  ( 9.689804814931740395, -24.98716964724288658, 26.94038990441057280 ) ) ;
#29861 = ORIENTED_EDGE ( 'NONE', *, *, #1511, .T. ) ;
#29862 = AXIS2_PLACEMENT_3D ( 'NONE', #21432, #11518, #2080 ) ;
#29863 = CARTESIAN_POINT ( 'NONE',  ( 5.771960588451495511, -1.304678385556235165, -33.78377053309999667 ) ) ;
#29864 = ORIENTED_EDGE ( 'NONE', *, *, #12253, .F. ) ;
#29865 = FACE_BOUND ( 'NONE', #1673, .T. ) ;
#29866 = CARTESIAN_POINT ( 'NONE',  ( 5.363076718300177959, -2.525690298526013677, -52.77872167392499847 ) ) ;
#29867 = ORIENTED_EDGE ( 'NONE', *, *, #2464, .T. ) ;
#29868 = ORIENTED_EDGE ( 'NONE', *, *, #11490, .T. ) ;
#29869 = SHAPE_DEFINITION_REPRESENTATION ( #20370, #3523 ) ;
#29870 = VERTEX_POINT ( 'NONE', #6870 ) ;
#29871 =( REPRESENTATION_RELATIONSHIP ('NONE','NONE', #2712, #25228 ) REPRESENTATION_RELATIONSHIP_WITH_TRANSFORMATION ( #21525 )SHAPE_REPRESENTATION_RELATIONSHIP( ) );
#29872 = EDGE_LOOP ( 'NONE', ( #24167, #1600, #21410, #12267 ) ) ;
#29873 = PRESENTATION_LAYER_ASSIGNMENT (  '', '', ( #12814 ) ) ;
#29874 = ORIENTED_EDGE ( 'NONE', *, *, #25816, .T. ) ;
#29875 = CARTESIAN_POINT ( 'NONE',  ( 24.06826093652101051, -20.50742065841456707, 1.000000000000000888 ) ) ;
#29876 = CARTESIAN_POINT ( 'NONE',  ( -0.4781950147703600273, -27.79606941020783140, 5.495819603435045053 ) ) ;
#29877 = DIRECTION ( 'NONE',  ( 0.000000000000000000, -2.257145581549999994E-12, -1.000000000000000000 ) ) ;
#29878 = CARTESIAN_POINT ( 'NONE',  ( -27.77052805885580966, -0.5052956280425524582, 0.7069222069999991920 ) ) ;
#29879 = CARTESIAN_POINT ( 'NONE',  ( 8.000000000842893755, -13.46643344106513318, -36.10519551497034030 ) ) ;
#29880 = EDGE_CURVE ( 'NONE', #6080, #10105, #5987, .T. ) ;
#29881 = CARTESIAN_POINT ( 'NONE',  ( -3.854342479829299339, 1.502750475587120160, -0.6999999999999992895 ) ) ;
#29882 = CARTESIAN_POINT ( 'NONE',  ( -1.531656806707240248, -4.518636249346831946, 0.3618694872999962397 ) ) ;
#29883 = AXIS2_PLACEMENT_3D ( 'NONE', #23807, #4596, #14203 ) ;
#29884 = CARTESIAN_POINT ( 'NONE',  ( 1.999932741570970673, 0.2648802556752510307, 230.8412452700000017 ) ) ;
#29885 = CARTESIAN_POINT ( 'NONE',  ( 249981.0602220003202, 207571.5434020000394, 379978.1847439997364 ) ) ;
#29886 = CIRCLE ( 'NONE', #27867, 1.926829268289999231 ) ;
#29887 = EDGE_CURVE ( 'NONE', #26129, #28677, #22495, .T. ) ;
#29888 = CARTESIAN_POINT ( 'NONE',  ( 3.550610403408205329, -5.007233058897099021, -12.72388893670000520 ) ) ;
#29889 = CARTESIAN_POINT ( 'NONE',  ( 2.831388952324535691, -5.386915550550475551, -32.60721934059999683 ) ) ;
#29890 = EDGE_CURVE ( 'NONE', #5989, #13375, #12730, .T. ) ;
#29891 = EDGE_CURVE ( 'NONE', #662, #18191, #11627, .T. ) ;
#29892 = DIRECTION ( 'NONE',  ( -0.7071067811865475727, -0.7071067811865475727, 0.000000000000000000 ) ) ;
#29893 = DIRECTION ( 'NONE',  ( 0.000000000000000000, -0.3420201433259318358, 0.9396926207858125046 ) ) ;
#29894 = CARTESIAN_POINT ( 'NONE',  ( -25.77914833267782413, -15.40383343775964065, 8.000000000000007105 ) ) ;
#29895 = DIRECTION ( 'NONE',  ( -1.000000000000000000, 5.687697999151106851E-16, -6.771501495036750356E-12 ) ) ;
#29896 = CARTESIAN_POINT ( 'NONE',  ( -3.834000099192893973, 2.652495916366584439, -25.46779765530001072 ) ) ;
#29897 = CARTESIAN_POINT ( 'NONE',  ( 22.64684861877907451, -14.33122899589083943, 225.2180667916778702 ) ) ;
#29898 = CARTESIAN_POINT ( 'NONE',  ( 9.499999999770000869, 21.70000000000000284, -64.10000000000000853 ) ) ;
#29899 = DIRECTION ( 'NONE',  ( 0.000000000000000000, 0.000000000000000000, -1.000000000000000000 ) ) ;
#29900 = CONICAL_SURFACE ( 'NONE', #19853, 12.22526471199999598, 1.243158134259999770 ) ;
#29901 = ORIENTED_EDGE ( 'NONE', *, *, #21022, .F. ) ;
#29902 = AXIS2_PLACEMENT_3D ( 'NONE', #169, #11808, #9752 ) ;
#29903 = VERTEX_POINT ( 'NONE', #2622 ) ;
#29904 = CARTESIAN_POINT ( 'NONE',  ( 23.35655559247464907, 15.07705663187610945, 5.680691777000007825 ) ) ;
#29905 = CARTESIAN_POINT ( 'NONE',  ( -4.520688084463085232, -31.79175087150127510, -80.44958056140195879 ) ) ;
#29906 = ORIENTED_EDGE ( 'NONE', *, *, #24846, .T. ) ;
#29907 = CARTESIAN_POINT ( 'NONE',  ( -22.88229166409188409, -13.95171381497113039, 224.0862411982057267 ) ) ;
#29908 = CARTESIAN_POINT ( 'NONE',  ( -24.39524108170000360, -13.33235248870000156, 224.0985996330000205 ) ) ;
#29909 = EDGE_LOOP ( 'NONE', ( #5596, #13067, #11957, #17183 ) ) ;
#29910 = CARTESIAN_POINT ( 'NONE',  ( -9.993285220779423383, -25.61999708228226069, 27.46711697431777921 ) ) ;
#29911 = ORIENTED_EDGE ( 'NONE', *, *, #13862, .F. ) ;
#29912 = VERTEX_POINT ( 'NONE', #7348 ) ;
#29913 =( NAMED_UNIT ( * ) SI_UNIT ( $, .STERADIAN. ) SOLID_ANGLE_UNIT ( ) );
#29914 = ORIENTED_EDGE ( 'NONE', *, *, #27794, .T. ) ;
#29915 = CARTESIAN_POINT ( 'NONE',  ( 27.48412515190000249, 9.625371191550000205, 229.0000000000000000 ) ) ;
#29916 = PRODUCT ( 'Drive Pawl', 'Drive Pawl', '', ( #5950 ) ) ;
#29917 = FACE_OUTER_BOUND ( 'NONE', #5908, .T. ) ;
#29918 = CYLINDRICAL_SURFACE ( 'NONE', #16064, 3.500000000000000444 ) ;
#29919 = CARTESIAN_POINT ( 'NONE',  ( 5.361384718770000113, -31.61859215249999977, 222.0000000000000000 ) ) ;
#29920 = CARTESIAN_POINT ( 'NONE',  ( -24.32472894358752313, 13.45989150749028873, 6.099998581000020792 ) ) ;
#29921 = CARTESIAN_POINT ( 'NONE',  ( -24.29460412914614764, -13.51351735463393311, 5.558304235695046280 ) ) ;
#29922 = ORIENTED_EDGE ( 'NONE', *, *, #26073, .F. ) ;
#29923 = FACE_OUTER_BOUND ( 'NONE', #26167, .T. ) ;
#29924 = CARTESIAN_POINT ( 'NONE',  ( -4.072259770650453525, 2.021700601781290629, -57.19877225282498756 ) ) ;
#29925 = CARTESIAN_POINT ( 'NONE',  ( -7.999999999673383044, -13.55640290378411095, -34.79039326168094703 ) ) ;
#29926 = CARTESIAN_POINT ( 'NONE',  ( 1.537204335059164872, 5.727607561491170785, -3.053410702900001716 ) ) ;
#29927 = CARTESIAN_POINT ( 'NONE',  ( 1.771049722044198971, -6.234229536879996481, -21.29535708919999593 ) ) ;
#29928 = DIRECTION ( 'NONE',  ( -5.551115123049999208E-18, 0.000000000000000000, -1.000000000000000000 ) ) ;
#29929 = CARTESIAN_POINT ( 'NONE',  ( -3.441895295100000141, -11.73074823080000151, 232.6627637660000119 ) ) ;
#29930 = CARTESIAN_POINT ( 'NONE',  ( 0.4852863613287607958, -4.020814519287960742, -91.97391714452653844 ) ) ;
#29931 = CARTESIAN_POINT ( 'NONE',  ( -9.700000000005733369, -13.84939817521907734, -36.47165854408401486 ) ) ;
#29932 = CARTESIAN_POINT ( 'NONE',  ( -23.67167941898225791, -13.99714052002833320, 223.9280906791120458 ) ) ;
#29933 = DIRECTION ( 'NONE',  ( 0.3633921898465292122, 0.9316362575375348731, -6.938893903907226800E-15 ) ) ;
#29934 = CARTESIAN_POINT ( 'NONE',  ( 18.35450725729999988, -0.3144534986609999749, 230.6999999999999886 ) ) ;
#29935 = CARTESIAN_POINT ( 'NONE',  ( 23.81569860410000317, -13.75000000000000000, 223.8999999999999773 ) ) ;
#29936 = ORIENTED_EDGE ( 'NONE', *, *, #3201, .T. ) ;
#29937 = CARTESIAN_POINT ( 'NONE',  ( 1.169850847344618083, -6.301966510834352775, -58.74125695792500323 ) ) ;
#29938 = CYLINDRICAL_SURFACE ( 'NONE', #13814, 2.500000000000000888 ) ;
#29939 = ORIENTED_EDGE ( 'NONE', *, *, #10425, .T. ) ;
#29940 = CARTESIAN_POINT ( 'NONE',  ( -4.273751495587445604, 4.364932658710685587, -4.568732180600005854 ) ) ;
#29941 = ORIENTED_EDGE ( 'NONE', *, *, #8095, .F. ) ;
#29942 = CYLINDRICAL_SURFACE ( 'NONE', #28823, 0.9999999999999988898 ) ;
#29943 = CARTESIAN_POINT ( 'NONE',  ( -4.162561055638823504, 0.1692103760920289357, -68.10000000002501963 ) ) ;
#29944 = ORIENTED_EDGE ( 'NONE', *, *, #16598, .T. ) ;
#29945 = EDGE_CURVE ( 'NONE', #8872, #20466, #6729, .T. ) ;
#29946 = VERTEX_POINT ( 'NONE', #31111 ) ;
#29947 = VERTEX_POINT ( 'NONE', #18990 ) ;
#29948 = DIRECTION ( 'NONE',  ( 5.962915006522623408E-16, 0.4383711467890811231, 0.8987940462991652613 ) ) ;
#29949 = ORIENTED_EDGE ( 'NONE', *, *, #29821, .T. ) ;
#29950 = DIRECTION ( 'NONE',  ( -2.764840495839172918E-12, -0.9128796883888953273, 0.4082287037029530552 ) ) ;
#29951 = CARTESIAN_POINT ( 'NONE',  ( -16.83342759559999635, -9.000000000000001776, -0.6999999999999992895 ) ) ;
#29952 = CARTESIAN_POINT ( 'NONE',  ( -5.427432314178970429, 2.515719109140460041, -65.77526299442500601 ) ) ;
#29953 = EDGE_CURVE ( 'NONE', #21389, #21418, #21322, .T. ) ;
#29954 = CARTESIAN_POINT ( 'NONE',  ( -27.79999999999999716, 2.356159711779999785E-11, 229.0000000000000000 ) ) ;
#29955 = CARTESIAN_POINT ( 'NONE',  ( -21.67076946895560852, 17.25020827395983503, -0.6577119969999878357 ) ) ;
#29956 = CARTESIAN_POINT ( 'NONE',  ( 9.450015891510000543, 19.99999999999999645, -44.04981409108790302 ) ) ;
#29957 = CARTESIAN_POINT ( 'NONE',  ( -4.276011752261355880, -9.320059656537083015, -25.35190844156560885 ) ) ;
#29958 = DIRECTION ( 'NONE',  ( -1.000000000000000000, 5.687697958343395332E-16, -6.771501495045879231E-12 ) ) ;
#29959 = ORIENTED_EDGE ( 'NONE', *, *, #22848, .T. ) ;
#29960 = CARTESIAN_POINT ( 'NONE',  ( -0.6370991518874352666, 4.292107257743940529, -10.86772091660000150 ) ) ;
#29961 = DIRECTION ( 'NONE',  ( 0.4353787270609800752, 0.9002473904559571416, 0.000000000000000000 ) ) ;
#29962 = LINE ( 'NONE', #17677, #27566 ) ;
#29963 = ORIENTED_EDGE ( 'NONE', *, *, #4587, .F. ) ;
#29964 = CYLINDRICAL_SURFACE ( 'NONE', #27245, 3.749999999999999556 ) ;
#29965 = DIRECTION ( 'NONE',  ( 0.9316362575375356503, 0.3633921898465274913, 0.000000000000000000 ) ) ;
#29966 = CARTESIAN_POINT ( 'NONE',  ( -21.02347494288676444, 19.26966991725469214, 4.000000085000010586 ) ) ;
#29967 = CARTESIAN_POINT ( 'NONE',  ( 27.79539923781770483, 0.5057481688777585305, 1.000000000000000888 ) ) ;
#29968 = DIRECTION ( 'NONE',  ( 0.000000000000000000, 0.000000000000000000, 1.000000000000000000 ) ) ;
#29969 = CARTESIAN_POINT ( 'NONE',  ( -4.216190498783925378, -2.983089501615236561, -44.28462724592499455 ) ) ;
#29970 = CARTESIAN_POINT ( 'NONE',  ( -10.98966923020000053, -24.66097101990000340, -1.689678586199998334 ) ) ;
#29971 = LINE ( 'NONE', #15349, #4215 ) ;
#29972 = ORIENTED_EDGE ( 'NONE', *, *, #10437, .T. ) ;
#29973 = EDGE_CURVE ( 'NONE', #29523, #17368, #30957, .T. ) ;
#29974 = CARTESIAN_POINT ( 'NONE',  ( 10.69999999999999929, -29.06671945340000107, -26.22544931050000017 ) ) ;
#29975 = CARTESIAN_POINT ( 'NONE',  ( 25.26809621129999783, 12.77001316559999999, 226.2000000000000171 ) ) ;
#29976 = CARTESIAN_POINT ( 'NONE',  ( 0.4806848194628341453, -3.969394140205261490, -68.10000000002499121 ) ) ;
#29977 = CARTESIAN_POINT ( 'NONE',  ( -3.552713678799999608E-15, -3.552713678799999608E-15, 91.66046017469999185 ) ) ;
#29978 = CARTESIAN_POINT ( 'NONE',  ( -24.05209696821570731, 13.94187115378248976, 5.961515049095109653 ) ) ;
#29979 = CARTESIAN_POINT ( 'NONE',  ( 14.84835410051307036, -24.88989065226013153, -32.95556094950757142 ) ) ;
#29980 = CARTESIAN_POINT ( 'NONE',  ( 0.3401257266749637687, 2.989789856715318717, -42.27519293863180394 ) ) ;
#29981 = CARTESIAN_POINT ( 'NONE',  ( 1.387947292976095426, 4.364053279572889465, -60.86492395752500784 ) ) ;
#29982 = ORIENTED_EDGE ( 'NONE', *, *, #24595, .T. ) ;
#29983 = EDGE_CURVE ( 'NONE', #19781, #25596, #14254, .T. ) ;
#29984 = CARTESIAN_POINT ( 'NONE',  ( -8.699999999731023337, -27.70368077816327101, -25.45737431350073265 ) ) ;
#29985 = ORIENTED_EDGE ( 'NONE', *, *, #6805, .F. ) ;
#29986 = CARTESIAN_POINT ( 'NONE',  ( 27.98121187870611593, -9.706323496128696604, 1.000000000000000888 ) ) ;
#29987 = ORIENTED_EDGE ( 'NONE', *, *, #16182, .F. ) ;
#29988 = CARTESIAN_POINT ( 'NONE',  ( -9.500000000000000000, 20.99999999999999645, -60.10000000019999788 ) ) ;
#29989 = CARTESIAN_POINT ( 'NONE',  ( 5.361384718760000112, -31.61859215249999977, 229.0000000000000000 ) ) ;
#29990 = CARTESIAN_POINT ( 'NONE',  ( 0.01829671460970255098, 3.547951512854722100, 0.000000000000000000 ) ) ;
#29991 = CARTESIAN_POINT ( 'NONE',  ( -26.79566689313578109, 10.13197864253886848, 8.000000000000007105 ) ) ;
#29992 = CARTESIAN_POINT ( 'NONE',  ( -12.75378086759999796, -22.00000000000000000, -31.28675134614999820 ) ) ;
#29993 = CARTESIAN_POINT ( 'NONE',  ( 1.127732790480000080, -28.47784299079999926, 225.0000014190000002 ) ) ;
#29994 = EDGE_LOOP ( 'NONE', ( #7785, #25117, #23662, #24812 ) ) ;
#29995 = CARTESIAN_POINT ( 'NONE',  ( -14.60916135985672071, 28.04296594682689658, 8.000000000000007105 ) ) ;
#29996 = ADVANCED_FACE ( 'NONE', ( #17242 ), #26849, .F. ) ;
#29997 = CARTESIAN_POINT ( 'NONE',  ( 28.35924375250000296, -2.370246001849999498E-14, 229.7625741969999922 ) ) ;
#29998 = CIRCLE ( 'NONE', #14943, 27.69999999999999929 ) ;
#29999 = EDGE_CURVE ( 'NONE', #15620, #25870, #30004, .T. ) ;
#30000 = CARTESIAN_POINT ( 'NONE',  ( -2.393497562785666055, 2.854340613466038512, 230.7151724862272602 ) ) ;
#30001 = CARTESIAN_POINT ( 'NONE',  ( -7.999999999718343524, -24.19750589173343869, -27.32947359979155166 ) ) ;
#30002 = PLANE ( 'NONE',  #13500 ) ;
#30003 = AXIS2_PLACEMENT_3D ( 'NONE', #13955, #4041, #27793 ) ;
#30004 = B_SPLINE_CURVE_WITH_KNOTS ( 'NONE', 3,
 ( #21513, #9551, #27458, #30427, #22286, #10631, #3233, #17852, #19926, #20225, #13577, #17693, #12522, #29819, #16092, #27311, #7949, #5594, #29514, #5901, #591, #12676, #10173, #24646, #892, #5750 ),
 .UNSPECIFIED., .F., .F.,
 ( 4, 2, 2, 2, 1, 1, 1, 1, 1, 1, 2, 2, 2, 2, 2, 4 ),
 ( 0.000000000000000000, 0.2499999999999633626, 0.3749999999999450440, 0.4374999999999361067, 0.4687499999999313882, 0.4843749999999291123, 0.4921874999999278910, 0.4960937499999271139, 0.4980468749999268363, 0.4990234374999269473, 0.4995117187499270583, 0.4999999999999272804, 0.6249999999999453770, 0.7499999999999634737, 0.8749999999999817923, 1.000000000000000000 ),
 .UNSPECIFIED. ) ;
#30005 = CARTESIAN_POINT ( 'NONE',  ( 10.00000000070000183, -30.00000000000000000, -28.40000000000000213 ) ) ;
#30006 = CARTESIAN_POINT ( 'NONE',  ( 0.9837925379835922302, -27.78276979301110572, 224.5041803965649763 ) ) ;
#30007 = CARTESIAN_POINT ( 'NONE',  ( 4.545032752014871669, -0.3361547907463971474, -49.12442242802499237 ) ) ;
#30008 = EDGE_CURVE ( 'NONE', #16461, #20682, #2985, .T. ) ;
#30009 = CARTESIAN_POINT ( 'NONE',  ( -16.85878449349630870, 12.10909424796742329, -1.400000000000002132 ) ) ;
#30010 = FACE_BOUND ( 'NONE', #17628, .T. ) ;
#30011 = CARTESIAN_POINT ( 'NONE',  ( -18.32656039618751009, 20.00000276249100395, 230.6693274794374986 ) ) ;
#30012 = CARTESIAN_POINT ( 'NONE',  ( -24.31247271682645206, -11.33627354958356825, 43.21714158842222986 ) ) ;
#30013 = B_SPLINE_CURVE_WITH_KNOTS ( 'NONE', 3,
 ( #1331, #8386, #8549, #1646, #20519, #6359 ),
 .UNSPECIFIED., .F., .F.,
 ( 4, 2, 4 ),
 ( 0.000000000000000000, 0.4999999999999997780, 1.000000000000000000 ),
 .UNSPECIFIED. ) ;
#30014 = CARTESIAN_POINT ( 'NONE',  ( 23.86403265435992083, -13.66628296921426156, 226.0999999999988859 ) ) ;
#30015 = VERTEX_POINT ( 'NONE', #25704 ) ;
#30016 = CARTESIAN_POINT ( 'NONE',  ( -6.074876045044606876, 0.8789665559579967757, -34.25783976329999092 ) ) ;
#30017 = VECTOR ( 'NONE', #27367, 1000.000000000000114 ) ;
#30018 = EDGE_CURVE ( 'NONE', #18284, #17478, #4498, .T. ) ;
#30019 = EDGE_LOOP ( 'NONE', ( #5407, #25316, #18941, #20424 ) ) ;
#30020 = DIRECTION ( 'NONE',  ( -0.9880370573969196046, 0.1542166437529879086, -5.551115123125782071E-14 ) ) ;
#30021 = CARTESIAN_POINT ( 'NONE',  ( 4.101176313917077820, -1.931410228222282921, -52.29872167392500160 ) ) ;
#30022 = ORIENTED_EDGE ( 'NONE', *, *, #5775, .T. ) ;
#30023 = VECTOR ( 'NONE', #21533, 1000.000000000000114 ) ;
#30024 = APPLICATION_PROTOCOL_DEFINITION ( 'draft international standard', 'automotive_design', 1998, #29691 ) ;
#30025 = B_SPLINE_CURVE_WITH_KNOTS ( 'NONE', 3,
 ( #2724, #683, #536, #9645, #29146, #22080, #24438, #19406, #28994, #2873, #12320, #22231, #16717, #17347, #21930, #14995, #12465, #5079, #26951, #14535, #377, #12619, #17038, #24129, #21766, #4783 ),
 .UNSPECIFIED., .F., .F.,
 ( 4, 2, 2, 1, 1, 2, 2, 2, 2, 2, 1, 1, 2, 2, 4 ),
 ( 0.000000000000000000, 0.1250000000000019984, 0.1875000000000021927, 0.2187500000000021372, 0.2343750000000012768, 0.2421875000000015266, 0.2500000000000017764, 0.4999999999999836797, 0.6249999999999745759, 0.6874999999999700240, 0.7187499999999678035, 0.7343749999999679146, 0.7421874999999686917, 0.7499999999999694689, 1.000000000000000000 ),
 .UNSPECIFIED. ) ;
#30026 = VERTEX_POINT ( 'NONE', #23183 ) ;
#30027 = AXIS2_PLACEMENT_3D ( 'NONE', #3029, #12622, #22233 ) ;
#30028 = EDGE_LOOP ( 'NONE', ( #26628, #24730, #10265, #14603 ) ) ;
#30029 = CARTESIAN_POINT ( 'NONE',  ( -17.93031264004542891, -9.094488044133550275, 0.000000000000000000 ) ) ;
#30030 = EDGE_CURVE ( 'NONE', #21281, #4391, #13858, .T. ) ;
#30031 = CARTESIAN_POINT ( 'NONE',  ( -0.6094664100040195764, -28.49364619262437870, 4.999998581000003384 ) ) ;
#30032 = CARTESIAN_POINT ( 'NONE',  ( -17.04621913067799710, -32.00000000058999916, -25.51324865459000080 ) ) ;
#30033 = CARTESIAN_POINT ( 'NONE',  ( 27.79999999980000069, -7.282770092339999835, 222.0000000000000000 ) ) ;
#30034 = CARTESIAN_POINT ( 'NONE',  ( 24.09856112909999837, -15.21545593799999985, 225.0000014190000002 ) ) ;
#30035 = CARTESIAN_POINT ( 'NONE',  ( -4.600743226517092666, 1.661770424157335224, -0.6999999999999992895 ) ) ;
#30036 = CARTESIAN_POINT ( 'NONE',  ( -5.478535709405480958, -2.209361269785813153, 0.002802565500000658849 ) ) ;
#30037 = CARTESIAN_POINT ( 'NONE',  ( 1.601210460384887568, 1.226419552957089820, 230.8412452700000301 ) ) ;
#30038 = CARTESIAN_POINT ( 'NONE',  ( 10.14902473071355793, -26.01926976408358527, 42.06031501460000044 ) ) ;
#30039 = EDGE_LOOP ( 'NONE', ( #24501, #15549, #3784, #8866, #21026 ) ) ;
#30040 = CIRCLE ( 'NONE', #31067, 3.000000000000001332 ) ;
#30041 = CARTESIAN_POINT ( 'NONE',  ( -4.363437395929424589, 0.1294788321584636748, -13.68304957890000750 ) ) ;
#30042 = CARTESIAN_POINT ( 'NONE',  ( 3.155489075140828437, 3.034105443485042741, -35.32341724620001600 ) ) ;
#30043 = CARTESIAN_POINT ( 'NONE',  ( -1.630907768819999992, -5.558498092260000689, 226.6412452697800006 ) ) ;
#30044 = CARTESIAN_POINT ( 'NONE',  ( 9.000000000000000000, -130.0000000000000000, -42.39999999999999858 ) ) ;
#30045 = DIRECTION ( 'NONE',  ( 1.000000000000000000, 0.000000000000000000, 0.000000000000000000 ) ) ;
#30046 = CARTESIAN_POINT ( 'NONE',  ( 0.03443198226909999909, -27.80021999669999744, 226.1000014189999945 ) ) ;
#30047 = CARTESIAN_POINT ( 'NONE',  ( -17.49199711315135986, -29.39779533043000015, -32.78913491261000246 ) ) ;
#30048 = AXIS2_PLACEMENT_3D ( 'NONE', #14213, #26171, #9799 ) ;
#30049 = CARTESIAN_POINT ( 'NONE',  ( 19.80538173989999962, 19.50875420239999869, 228.5999999789999890 ) ) ;
#30050 = CARTESIAN_POINT ( 'NONE',  ( -8.699999999666752970, -13.44080163377184256, -35.27486921256096508 ) ) ;
#30051 = CARTESIAN_POINT ( 'NONE',  ( 0.6686231747119999458, -28.49266848160000265, 224.0990955869999937 ) ) ;
#30052 = VECTOR ( 'NONE', #18580, 1000.000000000000000 ) ;
#30053 = B_SPLINE_CURVE_WITH_KNOTS ( 'NONE', 1,
 ( #14314, #27715 ),
 .UNSPECIFIED., .F., .F.,
 ( 2, 2 ),
 ( -2.556023926959999973E-06, 0.7000000000009999335 ),
 .UNSPECIFIED. ) ;
#30054 = VERTEX_POINT ( 'NONE', #16862 ) ;
#30055 = ORIENTED_EDGE ( 'NONE', *, *, #3875, .F. ) ;
#30056 = CARTESIAN_POINT ( 'NONE',  ( 23.94466869970572986, 15.45669658583985751, 5.680691777000007825 ) ) ;
#30057 = FACE_OUTER_BOUND ( 'NONE', #11440, .T. ) ;
#30058 = EDGE_LOOP ( 'NONE', ( #1978, #24048, #3711, #10159 ) ) ;
#30059 = CARTESIAN_POINT ( 'NONE',  ( 14.39562240800000126, -9.581487064249998298, 5.000000000000000000 ) ) ;
#30060 = APPLICATION_CONTEXT ( 'automotive_design' ) ;
#30061 = CARTESIAN_POINT ( 'NONE',  ( -24.60699806910000120, -12.93667933180000063, 225.0000014190000002 ) ) ;
#30062 = EDGE_CURVE ( 'NONE', #6137, #25637, #5226, .T. ) ;
#30063 = EDGE_LOOP ( 'NONE', ( #27045, #5332, #30729, #21101 ) ) ;
#30064 = CARTESIAN_POINT ( 'NONE',  ( -1.071233646927975736, -26.77863814329466052, 4.711903514136000837 ) ) ;
#30065 = ORIENTED_EDGE ( 'NONE', *, *, #30062, .F. ) ;
#30066 = ORIENTED_EDGE ( 'NONE', *, *, #6301, .F. ) ;
#30067 = AXIS2_PLACEMENT_3D ( 'NONE', #21113, #4579, #28184 ) ;
#30068 = ADVANCED_FACE ( 'NONE', ( #9155 ), #19075, .F. ) ;
#30069 = ORIENTED_EDGE ( 'NONE', *, *, #9821, .F. ) ;
#30070 = CARTESIAN_POINT ( 'NONE',  ( 3.728365721074163197, -0.5735620887561410086, -35.69999999999999574 ) ) ;
#30071 = ADVANCED_FACE ( 'NONE', ( #26009 ), #4762, .T. ) ;
#30072 = ORIENTED_EDGE ( 'NONE', *, *, #20474, .F. ) ;
#30073 = B_SPLINE_CURVE_WITH_KNOTS ( 'NONE', 5,
 ( #22401, #848, #19889, #2585, #29470, #7455, #26653, #29159, #7309, #7906, #27116, #5091 ),
 .UNSPECIFIED., .F., .F.,
 ( 6, 3, 3, 6 ),
 ( -1.429360140840000071, -1.143488112685019376, -0.5717440563530578057, -0.2292465842890714089 ),
 .UNSPECIFIED. ) ;
#30074 = AXIS2_PLACEMENT_3D ( 'NONE', #18801, #28409, #7580 ) ;
#30075 = CARTESIAN_POINT ( 'NONE',  ( -10.69999999999999929, -24.87867968679999819, -26.27867968680000033 ) ) ;
#30076 = CARTESIAN_POINT ( 'NONE',  ( 21.16705260770000052, -21.30254494060000070, 222.0000000000000000 ) ) ;
#30077 = SURFACE_SIDE_STYLE ('',( #8190 ) ) ;
#30078 = CARTESIAN_POINT ( 'NONE',  ( -6.676371816449358398, 5.924696735301250961, -40.36883684629870572 ) ) ;
#30079 = AXIS2_PLACEMENT_3D ( 'NONE', #13194, #13519, #20599 ) ;
#30080 = CARTESIAN_POINT ( 'NONE',  ( -7.097978819962594166, -5.572998883415808180, -27.02754848611320071 ) ) ;
#30081 = CARTESIAN_POINT ( 'NONE',  ( -10.69999999997017248, -29.92209366267258019, -29.18485145335326436 ) ) ;
#30082 = CARTESIAN_POINT ( 'NONE',  ( 23.77684695985370311, -14.40559418229910449, 4.854156763425871546 ) ) ;
#30083 = ORIENTED_EDGE ( 'NONE', *, *, #23107, .F. ) ;
#30084 = CARTESIAN_POINT ( 'NONE',  ( -3.885731905334995684, 2.027028853511404272, -1.918764356300002305 ) ) ;
#30085 = CARTESIAN_POINT ( 'NONE',  ( -4.663991843195165465, -3.413757688390889555, -18.27254627009999766 ) ) ;
#30086 = DIRECTION ( 'NONE',  ( -1.000000000000000000, -5.289357741729999318E-17, 0.000000000000000000 ) ) ;
#30087 = CARTESIAN_POINT ( 'NONE',  ( 10.69999999999999929, -24.90230198360000102, -26.25506235030000113 ) ) ;
#30088 = CARTESIAN_POINT ( 'NONE',  ( -0.6309877232518290580, -4.042619772830049918, -91.86228428259488510 ) ) ;
#30089 = CARTESIAN_POINT ( 'NONE',  ( -21.39843895140000285, 17.14751838560000152, 230.6999999999999886 ) ) ;
#30090 = CARTESIAN_POINT ( 'NONE',  ( -26.02053815395284175, 12.91565460411935895, 1.000000000000000888 ) ) ;
#30091 = DIRECTION ( 'NONE',  ( 1.000000000000000000, -0.000000000000000000, -2.257150022439999944E-12 ) ) ;
#30092 = AXIS2_PLACEMENT_3D ( 'NONE', #29657, #20371, #18154 ) ;
#30093 = CARTESIAN_POINT ( 'NONE',  ( 5.229687933670000177, -30.84198039099999633, 229.0000000000000000 ) ) ;
#30094 = CARTESIAN_POINT ( 'NONE',  ( -19.60939915890000051, -18.53226158640000065, 230.6999999999999886 ) ) ;
#30095 = CARTESIAN_POINT ( 'NONE',  ( 10.92933985129999996, -24.70409753159999866, -1.761594278200002917 ) ) ;
#30096 = ORIENTED_EDGE ( 'NONE', *, *, #15572, .F. ) ;
#30097 = CARTESIAN_POINT ( 'NONE',  ( 4.003591150705129387, -2.204345408526039218, -58.30843849682500490 ) ) ;
#30098 = FACE_OUTER_BOUND ( 'NONE', #23470, .T. ) ;
#30099 = ORIENTED_EDGE ( 'NONE', *, *, #17883, .T. ) ;
#30100 = CARTESIAN_POINT ( 'NONE',  ( -5.837703056366890131, -0.5751183411571159088, -1.146254077200002719 ) ) ;
#30101 = VERTEX_POINT ( 'NONE', #4452 ) ;
#30102 = CARTESIAN_POINT ( 'NONE',  ( -23.77308074856162889, 14.41182440783502550, 4.853949414814223040 ) ) ;
#30103 = VECTOR ( 'NONE', #28892, 1000.000000000000000 ) ;
#30104 = CARTESIAN_POINT ( 'NONE',  ( 24.08872333959831380, -11.87645233066226069, 186.7828584119999960 ) ) ;
#30105 = ORIENTED_EDGE ( 'NONE', *, *, #14186, .F. ) ;
#30106 = DIRECTION ( 'NONE',  ( 1.075528555106586974E-13, 0.9622309798138365400, 0.2722343503059523884 ) ) ;
#30107 = ORIENTED_EDGE ( 'NONE', *, *, #29853, .F. ) ;
#30108 = ORIENTED_EDGE ( 'NONE', *, *, #3047, .F. ) ;
#30109 = CARTESIAN_POINT ( 'NONE',  ( 18.13191322229999969, 10.47263190749999495, -0.7999999992999995424 ) ) ;
#30110 = EDGE_CURVE ( 'NONE', #18767, #25637, #29836, .T. ) ;
#30111 = EDGE_LOOP ( 'NONE', ( #26939, #19096, #11266, #4726 ) ) ;
#30112 = FACE_OUTER_BOUND ( 'NONE', #15678, .T. ) ;
#30113 = EDGE_CURVE ( 'NONE', #25714, #20192, #22888, .T. ) ;
#30114 = FACE_BOUND ( 'NONE', #28474, .T. ) ;
#30115 = CARTESIAN_POINT ( 'NONE',  ( -3.112296099710462727, 3.758517760630103233, -62.99933298492499034 ) ) ;
#30116 = DIRECTION ( 'NONE',  ( 0.000000000000000000, 0.000000000000000000, 1.000000000000000000 ) ) ;
#30117 = CARTESIAN_POINT ( 'NONE',  ( -0.9891023348422632866, -26.78175549063930205, 224.5133938523520385 ) ) ;
#30118 = DIRECTION ( 'NONE',  ( -0.2815395311429195746, -0.9595496299847261490, 0.000000000000000000 ) ) ;
#30119 = CARTESIAN_POINT ( 'NONE',  ( 6.830207510690000570E-10, 8.201972434560000246E-11, 230.0000000000000000 ) ) ;
#30120 = CARTESIAN_POINT ( 'NONE',  ( -25.12046394328327281, 13.46291001840482160, 3.957489296000010981 ) ) ;
#30121 = PRODUCT_DEFINITION_CONTEXT ( 'detailed design', #3966, 'design' ) ;
#30122 = AXIS2_PLACEMENT_3D ( 'NONE', #8350, #3482, #13393 ) ;
#30123 = CARTESIAN_POINT ( 'NONE',  ( 4.310466091822805268, 1.786666325167808544, -11.49261350019999739 ) ) ;
#30124 = CARTESIAN_POINT ( 'NONE',  ( 24.37165445055180157, -14.77472140295711434, 4.895781291000017355 ) ) ;
#30125 = CARTESIAN_POINT ( 'NONE',  ( 19.56378028550000181, 19.56885116670000357, 229.4995147189999898 ) ) ;
#30126 = ORIENTED_EDGE ( 'NONE', *, *, #886, .F. ) ;
#30127 = CARTESIAN_POINT ( 'NONE',  ( 17.14656078599760392, 12.09981795542235439, -1.000005633855494125E-09 ) ) ;
#30128 = CARTESIAN_POINT ( 'NONE',  ( -22.74641636049597793, -14.17229404738486132, 4.366512952753266674 ) ) ;
#30129 = CARTESIAN_POINT ( 'NONE',  ( 8.000000000000000000, -17.74403716370463968, -75.33663091226621589 ) ) ;
#30130 = CARTESIAN_POINT ( 'NONE',  ( 24.63996007208032779, 13.90215428157462263, 0.5514267500000280542 ) ) ;
#30131 = CARTESIAN_POINT ( 'NONE',  ( 7.999999999977091214, -107.4273096626279482, 14.66297538114749344 ) ) ;
#30132 = CARTESIAN_POINT ( 'NONE',  ( -10.32522729140000095, -24.73114799960000099, -1.399999999999998579 ) ) ;
#30133 = CARTESIAN_POINT ( 'NONE',  ( -2.486939662212003466, -15.93335509046200826, -109.1271631200378351 ) ) ;
#30134 = EDGE_LOOP ( 'NONE', ( #13060, #22154, #4732, #13412, #6652 ) ) ;
#30135 = CARTESIAN_POINT ( 'NONE',  ( 24.27467683999808301, -13.55001166052597128, 3.904029272000009154 ) ) ;
#30136 = CARTESIAN_POINT ( 'NONE',  ( 26.95545381250000361, 8.667969360479998997, 223.3999999999999773 ) ) ;
#30137 = EDGE_CURVE ( 'NONE', #90, #29694, #10126, .T. ) ;
#30138 = CARTESIAN_POINT ( 'NONE',  ( 2.235634928214019990, -3.593586099038730275, -68.10000000002501963 ) ) ;
#30139 = B_SPLINE_CURVE_WITH_KNOTS ( 'NONE', 5,
 ( #833, #15139, #5385, #3025, #22541, #10576, #12618, #20170, #29761, #8191, #17795, #8664, #18261, #17942, #27555 ),
 .UNSPECIFIED., .F., .F.,
 ( 6, 3, 3, 3, 6 ),
 ( 0.000000000000000000, 0.09999999999828219910, 0.3999999999988547716, 0.6999999999999999556, 1.000000000000000000 ),
 .UNSPECIFIED. ) ;
#30140 = CARTESIAN_POINT ( 'NONE',  ( -12.77820031340000106, 20.99999999999999645, -56.10000000020000499 ) ) ;
#30141 = CARTESIAN_POINT ( 'NONE',  ( -4.194654192376331636, 0.4516430622356696900, -44.10000000002499831 ) ) ;
#30142 = DIRECTION ( 'NONE',  ( 0.000000000000000000, 0.000000000000000000, 1.000000000000000000 ) ) ;
#30143 = DIRECTION ( 'NONE',  ( 0.000000000000000000, 0.000000000000000000, 1.000000000000000000 ) ) ;
#30144 = CARTESIAN_POINT ( 'NONE',  ( 24.07552037900000030, -13.90000980950000020, 226.1000014189999945 ) ) ;
#30145 = CARTESIAN_POINT ( 'NONE',  ( 2.833778097863423717, 3.583098331959791771, -64.03768011632499224 ) ) ;
#30146 = VERTEX_POINT ( 'NONE', #6961 ) ;
#30147 = FACE_OUTER_BOUND ( 'NONE', #12571, .T. ) ;
#30148 = ORIENTED_EDGE ( 'NONE', *, *, #18675, .F. ) ;
#30149 = CARTESIAN_POINT ( 'NONE',  ( -20.20536873837831493, -21.08852116449837766, 0.5514282400000125595 ) ) ;
#30150 = ORIENTED_EDGE ( 'NONE', *, *, #20847, .F. ) ;
#30151 = CARTESIAN_POINT ( 'NONE',  ( -11.63809019400000011, -24.14124255240000139, -0.6999999999999992895 ) ) ;
#30152 = DIRECTION ( 'NONE',  ( 0.000000000000000000, 0.000000000000000000, -1.000000000000000000 ) ) ;
#30153 = CARTESIAN_POINT ( 'NONE',  ( 25.41286869299526074, -12.90211872965451079, 4.492873455000018446 ) ) ;
#30154 = CARTESIAN_POINT ( 'NONE',  ( -23.55444264242456498, 16.04540112444970390, 8.000000000000007105 ) ) ;
#30155 = CARTESIAN_POINT ( 'NONE',  ( -24.72757892072304742, 14.23267199169132979, 8.000000000000007105 ) ) ;
#30156 = CARTESIAN_POINT ( 'NONE',  ( 7.476504230907038639, -15.91356728955108046, -74.67039436335275582 ) ) ;
#30157 = CARTESIAN_POINT ( 'NONE',  ( -0.06887222117169999880, -27.80017212539999960, 223.9013489249999793 ) ) ;
#30158 = ORIENTED_EDGE ( 'NONE', *, *, #4629, .F. ) ;
#30159 = CARTESIAN_POINT ( 'NONE',  ( -0.5400457538399249247, -3.901550194262492610, -44.10000000002499121 ) ) ;
#30160 = CARTESIAN_POINT ( 'NONE',  ( 1.060521003860056405E-06, 19.99999999974424725, -0.6999999999999784173 ) ) ;
#30161 = CARTESIAN_POINT ( 'NONE',  ( 1.099998580829999906, -27.77839262550000043, 225.0000014190000002 ) ) ;
#30162 = EDGE_CURVE ( 'NONE', #18133, #7840, #212, .T. ) ;
#30163 = CARTESIAN_POINT ( 'NONE',  ( -4.041451884379999804, 9.156941871420000667E-11, 230.5235986622430175 ) ) ;
#30164 = FACE_OUTER_BOUND ( 'NONE', #860, .T. ) ;
#30165 = CARTESIAN_POINT ( 'NONE',  ( 0.000000000000000000, 4.811145170119999648, -67.12721591429999535 ) ) ;
#30166 = DIRECTION ( 'NONE',  ( 0.7198537139083028835, -0.6941258031311204890, 0.000000000000000000 ) ) ;
#30167 = CONICAL_SURFACE ( 'NONE', #11085, 0.9999999999991042721, 0.7853981633970000820 ) ;
#30168 = CARTESIAN_POINT ( 'NONE',  ( -26.66783967069105898, -7.507193849635574345, 0.000000000000000000 ) ) ;
#30169 = CARTESIAN_POINT ( 'NONE',  ( 4.432674687120906398, 4.607520344841867121, -48.69426496242499525 ) ) ;
#30170 = EDGE_CURVE ( 'NONE', #22531, #1522, #22816, .T. ) ;
#30171 = PRODUCT_DEFINITION_SHAPE ( 'NONE', 'NONE',  #7911 ) ;
#30172 = CARTESIAN_POINT ( 'NONE',  ( 26.93696268452645626, 0.4901285798022169127, 0.000000000000000000 ) ) ;
#30173 = CARTESIAN_POINT ( 'NONE',  ( -20.21685729201897175, 19.99998469724611283, 229.4596784481962288 ) ) ;
#30174 = CARTESIAN_POINT ( 'NONE',  ( 2.451696673680768157, -2.753086555842796379, 230.7286668686129190 ) ) ;
#30175 = CARTESIAN_POINT ( 'NONE',  ( -10.49791847189999849, 19.99999999999999645, -3.602081527999998034 ) ) ;
#30176 = AXIS2_PLACEMENT_3D ( 'NONE', #15911, #11504, #21107 ) ;
#30177 = VERTEX_POINT ( 'NONE', #23964 ) ;
#30178 = CARTESIAN_POINT ( 'NONE',  ( 3.996952828541906033, 3.843200228390037498, -36.32341724620000889 ) ) ;
#30179 = ORIENTED_EDGE ( 'NONE', *, *, #6074, .T. ) ;
#30180 = EDGE_CURVE ( 'NONE', #22622, #23040, #4595, .T. ) ;
#30181 = CARTESIAN_POINT ( 'NONE',  ( 4.692739937114380311, 0.5303478879429834869, -55.01771407622499765 ) ) ;
#30182 = ORIENTED_EDGE ( 'NONE', *, *, #17902, .T. ) ;
#30183 = ADVANCED_FACE ( 'NONE', ( #9627 ), #11839, .F. ) ;
#30184 = APPLICATION_PROTOCOL_DEFINITION ( 'draft international standard', 'automotive_design', 1998, #9379 ) ;
#30185 = ORIENTED_EDGE ( 'NONE', *, *, #19785, .T. ) ;
#30186 = ORIENTED_EDGE ( 'NONE', *, *, #27698, .T. ) ;
#30187 = CARTESIAN_POINT ( 'NONE',  ( 14.75111860152108534, -30.63528571087327634, -24.72562157583271514 ) ) ;
#30188 = DIRECTION ( 'NONE',  ( 0.000000000000000000, 1.000000000000000000, 0.000000000000000000 ) ) ;
#30189 = FILL_AREA_STYLE_COLOUR ( '', #19969 ) ;
#30190 = PRODUCT_RELATED_PRODUCT_CATEGORY ( 'part', '', ( #13934 ) ) ;
#30191 = AXIS2_PLACEMENT_3D ( 'NONE', #9611, #21728, #9764 ) ;
#30192 = CARTESIAN_POINT ( 'NONE',  ( -8.699999999985950083, -116.8589940772574920, 11.34037319969351643 ) ) ;
#30193 = CARTESIAN_POINT ( 'NONE',  ( 7.707106507606773960, -115.2381290211091738, 21.69251943803729787 ) ) ;
#30194 = FACE_OUTER_BOUND ( 'NONE', #13069, .T. ) ;
#30195 = CARTESIAN_POINT ( 'NONE',  ( -5.440024667461782037, 2.837840394948672351, -1.418764356299999418 ) ) ;
#30196 = CARTESIAN_POINT ( 'NONE',  ( 1.948929461725908752, -0.5207266838928901187, 230.8412452700000301 ) ) ;
#30197 = CARTESIAN_POINT ( 'NONE',  ( 27.79999999999999716, -2.355626804729999831E-11, 222.0000000000000000 ) ) ;
#30198 = CARTESIAN_POINT ( 'NONE',  ( 1.526412975746457290, -4.524531468931415112, -16.20164732020000287 ) ) ;
#30199 = CARTESIAN_POINT ( 'NONE',  ( -4.901082056047598279, -4.330235462250267453, -33.83447003409999354 ) ) ;
#30200 = EDGE_CURVE ( 'NONE', #12805, #9943, #7229, .T. ) ;
#30201 = CARTESIAN_POINT ( 'NONE',  ( 4.054393030549999999, 4.288653550920000335, 226.6412452697800006 ) ) ;
#30202 = CARTESIAN_POINT ( 'NONE',  ( -8.000000000319866800, -28.58317312641834462, -30.97832802812172659 ) ) ;
#30203 = CARTESIAN_POINT ( 'NONE',  ( -19.68703433251029722, 19.53817007346649248, 0.6302326600000074386 ) ) ;
#30204 = CARTESIAN_POINT ( 'NONE',  ( -20.59280845669432836, -19.92816138975910434, 8.000000000000007105 ) ) ;
#30205 = CARTESIAN_POINT ( 'NONE',  ( -17.19683899162122387, -27.45185958154430850, -33.91262144105893839 ) ) ;
#30206 = CARTESIAN_POINT ( 'NONE',  ( 25.21071572825679752, 14.22418740194451914, 0.2374258030000131470 ) ) ;
#30207 = CARTESIAN_POINT ( 'NONE',  ( 2.020725942159999899, 3.500000000000000000, 227.9588918784999976 ) ) ;
#30208 = DIRECTION ( 'NONE',  ( 0.000000000000000000, 1.000000000000000000, 0.000000000000000000 ) ) ;
#30209 = ORIENTED_EDGE ( 'NONE', *, *, #30982, .F. ) ;
#30210 = EDGE_CURVE ( 'NONE', #15161, #17525, #20973, .T. ) ;
#30211 = CARTESIAN_POINT ( 'NONE',  ( 23.39354070784786543, 15.01969649483752001, 5.760134169000008519 ) ) ;
#30212 = DIRECTION ( 'NONE',  ( -1.881554647690000340E-09, 1.000000000000000000, 0.000000000000000000 ) ) ;
#30213 = AXIS2_PLACEMENT_3D ( 'NONE', #23332, #3971, #14042 ) ;
#30214 = VERTEX_POINT ( 'NONE', #11989 ) ;
#30215 = CARTESIAN_POINT ( 'NONE',  ( 3.040504021322313122, 1.733590290792417887, -0.5999999999999894307 ) ) ;
#30216 = CARTESIAN_POINT ( 'NONE',  ( -10.00000000000000000, 19.99999999999999645, -42.39999999999999858 ) ) ;
#30217 = CARTESIAN_POINT ( 'NONE',  ( 0.2196031082797668954, -26.79904496338328812, 3.912378621952441016 ) ) ;
#30218 = ORIENTED_EDGE ( 'NONE', *, *, #11703, .F. ) ;
#30219 = DIRECTION ( 'NONE',  ( 0.000000000000000000, 0.000000000000000000, -1.000000000000000000 ) ) ;
#30220 = ORIENTED_EDGE ( 'NONE', *, *, #20477, .T. ) ;
#30221 = ORIENTED_EDGE ( 'NONE', *, *, #12352, .T. ) ;
#30222 = FILL_AREA_STYLE ('',( #6460 ) ) ;
#30223 = EDGE_LOOP ( 'NONE', ( #16748, #24145, #18849 ) ) ;
#30224 = CARTESIAN_POINT ( 'NONE',  ( 22.54750148980000191, 18.07861229629999755, 229.0000000000000000 ) ) ;
#30225 = EDGE_CURVE ( 'NONE', #11948, #15558, #16243, .T. ) ;
#30226 = ORIENTED_EDGE ( 'NONE', *, *, #5119, .T. ) ;
#30227 = CARTESIAN_POINT ( 'NONE',  ( -8.699999999000075590, -28.07052640020997458, -25.59750589178178259 ) ) ;
#30228 = PRODUCT_DEFINITION ( 'UNKNOWN', '', #1295, #24476 ) ;
#30229 = CARTESIAN_POINT ( 'NONE',  ( -28.49999999970000175, -10.47094308429999998, 222.0000000000000000 ) ) ;
#30230 = CARTESIAN_POINT ( 'NONE',  ( 1.169668886176895350, 3.927335417484261182, -35.70000000000000284 ) ) ;
#30231 = CARTESIAN_POINT ( 'NONE',  ( -0.5716039300045591132, -28.49445895580208443, 4.689815098000011062 ) ) ;
#30232 = CARTESIAN_POINT ( 'NONE',  ( 11.20000000009999930, -22.55999999999999872, -28.39999999989999679 ) ) ;
#30233 = CARTESIAN_POINT ( 'NONE',  ( -26.80000000000000071, 1.776356839399999804E-15, -2.842170943039999687E-14 ) ) ;
#30234 = CARTESIAN_POINT ( 'NONE',  ( -1.015151870880000029, -28.48229306780000059, 225.5064930660000186 ) ) ;
#30235 = ORIENTED_EDGE ( 'NONE', *, *, #19030, .F. ) ;
#30236 = AXIS2_PLACEMENT_3D ( 'NONE', #115, #271, #21664 ) ;
#30237 = CARTESIAN_POINT ( 'NONE',  ( 2.445722248254770026, -3.773326582131152573, -1.103439388299995549 ) ) ;
#30238 = CARTESIAN_POINT ( 'NONE',  ( 5.195105410215491659, 3.969764343816663210, -23.36727430110000014 ) ) ;
#30239 = DIRECTION ( 'NONE',  ( 0.7071067811865475727, 0.7071067811865475727, 0.000000000000000000 ) ) ;
#30240 = EDGE_CURVE ( 'NONE', #24241, #17421, #8850, .T. ) ;
#30241 = CARTESIAN_POINT ( 'NONE',  ( 24.32472724076343695, -13.45989056521276872, 6.099998581000020792 ) ) ;
#30242 = AXIS2_PLACEMENT_3D ( 'NONE', #26172, #28824, #18769 ) ;
#30243 = CARTESIAN_POINT ( 'NONE',  ( 2.816533608213001916, -3.950362352052525061, -94.91462932778338768 ) ) ;
#30244 = CARTESIAN_POINT ( 'NONE',  ( -28.50000000000000000, -5.504861435589999933E-14, 229.0000000000000000 ) ) ;
#30245 = AXIS2_PLACEMENT_3D ( 'NONE', #26027, #18774, #28381 ) ;
#30246 = CARTESIAN_POINT ( 'NONE',  ( -2.945834232371903116, -0.7246911579439561102, -97.21305981300695009 ) ) ;
#30247 = DIRECTION ( 'NONE',  ( 0.3633921898465291567, 0.9316362575375349842, -5.551115123125783333E-14 ) ) ;
#30248 = ADVANCED_FACE ( 'NONE', ( #17327 ), #197, .F. ) ;
#30249 = CARTESIAN_POINT ( 'NONE',  ( -27.79999999999999716, 2.355804440410000085E-11, 229.0000000000000000 ) ) ;
#30250 = CARTESIAN_POINT ( 'NONE',  ( 17.91346439750000386, -3.648009858620000045, 230.6999999999999886 ) ) ;
#30251 = FACE_OUTER_BOUND ( 'NONE', #3127, .T. ) ;
#30252 = EDGE_LOOP ( 'NONE', ( #30995, #513, #11035, #11338, #25070 ) ) ;
#30253 = CARTESIAN_POINT ( 'NONE',  ( 1.815007998551255941, 5.706838904126064094, -60.46492395752500215 ) ) ;
#30254 = CARTESIAN_POINT ( 'NONE',  ( -7.534632680830988249, -6.582071621095836100, -34.26887834079445128 ) ) ;
#30255 = ORIENTED_EDGE ( 'NONE', *, *, #5615, .T. ) ;
#30256 = EDGE_CURVE ( 'NONE', #16606, #30101, #360, .T. ) ;
#30257 = CARTESIAN_POINT ( 'NONE',  ( 3.550610403408205329, -5.007233058897099021, -12.12388893670000201 ) ) ;
#30258 = EDGE_LOOP ( 'NONE', ( #778, #14680, #25412, #16440 ) ) ;
#30259 = FACE_OUTER_BOUND ( 'NONE', #27207, .T. ) ;
#30260 = AXIS2_PLACEMENT_3D ( 'NONE', #12079, #21686, #9401 ) ;
#30261 = CARTESIAN_POINT ( 'NONE',  ( -3.552713678799999608E-15, 0.000000000000000000, 93.60555127549999099 ) ) ;
#30263 = EDGE_LOOP ( 'NONE', ( #25121, #12, #30724, #6027 ) ) ;
#30262 = VECTOR ( 'NONE', #8016, 1000.000000000000000 ) ;
#30264 = CARTESIAN_POINT ( 'NONE',  ( 14.40197535836999876, -22.00000000000000000, -25.51324865394999719 ) ) ;
#30265 = EDGE_LOOP ( 'NONE', ( #14921, #8501, #28355, #22102 ) ) ;
#30266 = ORIENTED_EDGE ( 'NONE', *, *, #3084, .F. ) ;
#30267 = DIRECTION ( 'NONE',  ( 0.000000000000000000, 0.000000000000000000, 1.000000000000000000 ) ) ;
#30268 = B_SPLINE_CURVE_WITH_KNOTS ( 'NONE', 3,
 ( #25771, #3730, #1541, #11446, #10976, #30001 ),
 .UNSPECIFIED., .F., .F.,
 ( 4, 2, 4 ),
 ( 0.000000000000000000, 0.5000000000000000000, 1.000000000000000000 ),
 .UNSPECIFIED. ) ;
#30269 = ORIENTED_EDGE ( 'NONE', *, *, #30256, .F. ) ;
#30270 = PLANE ( 'NONE',  #2919 ) ;
#30271 = DIRECTION ( 'NONE',  ( -5.551115123049999208E-18, 0.000000000000000000, -1.000000000000000000 ) ) ;
#30272 = CARTESIAN_POINT ( 'NONE',  ( -4.475180390489594373, -2.644424941261572126, -67.57382590962500046 ) ) ;
#30273 = CARTESIAN_POINT ( 'NONE',  ( 26.80000000000000071, -5.684341886079999373E-14, 230.0000000000000000 ) ) ;
#30274 = DIRECTION ( 'NONE',  ( -5.962915006522622422E-16, -0.4383711467890810676, -0.8987940462991651502 ) ) ;
#30275 = CARTESIAN_POINT ( 'NONE',  ( -27.79999999999999716, 2.355410854109999913E-11, 222.0000000000000000 ) ) ;
#30276 = CARTESIAN_POINT ( 'NONE',  ( -23.45268582408035485, -12.96920632950135754, 5.993195173463121250 ) ) ;
#30277 = ORIENTED_EDGE ( 'NONE', *, *, #6584, .T. ) ;
#30278 = FACE_OUTER_BOUND ( 'NONE', #30666, .T. ) ;
#30279 = CARTESIAN_POINT ( 'NONE',  ( 4.945711323160860928, -2.526642934800090945, -10.91474735219999204 ) ) ;
#30280 = CARTESIAN_POINT ( 'NONE',  ( 0.000000000000000000, 0.000000000000000000, -2.842170943039999687E-14 ) ) ;
#30281 = ADVANCED_FACE ( 'NONE', ( #29280 ), #27083, .T. ) ;
#30282 = CARTESIAN_POINT ( 'NONE',  ( -4.861312627776431583, -9.716283825163692711, -32.74022090983473987 ) ) ;
#30283 = AXIS2_PLACEMENT_3D ( 'NONE', #28233, #14235, #23995 ) ;
#30284 = ORIENTED_EDGE ( 'NONE', *, *, #19819, .F. ) ;
#30285 = CARTESIAN_POINT ( 'NONE',  ( 25.08428924680000094, -13.52916357279999993, 224.2398747240000034 ) ) ;
#30286 = CARTESIAN_POINT ( 'NONE',  ( 0.000000000000000000, 0.000000000000000000, 115.0000000000000000 ) ) ;
#30287 = CARTESIAN_POINT ( 'NONE',  ( -27.79999999180000358, -2.354738626309999853E-11, 222.0000000000000000 ) ) ;
#30288 = CARTESIAN_POINT ( 'NONE',  ( 24.22335707914676206, 13.66710489523639716, 0.08279771000002655867 ) ) ;
#30289 = LINE ( 'NONE', #10937, #3984 ) ;
#30290 = ADVANCED_FACE ( 'NONE', ( #29593 ), #29344, .F. ) ;
#30291 = CARTESIAN_POINT ( 'NONE',  ( -3.982632971385688947, -19.71206033698065596, -27.86495495700036784 ) ) ;
#30292 = CARTESIAN_POINT ( 'NONE',  ( -23.23955040174346465, -15.25661106733265981, 5.208368890000008911 ) ) ;
#30294 = EDGE_CURVE ( 'NONE', #3623, #16606, #1729, .T. ) ;
#30293 = CARTESIAN_POINT ( 'NONE',  ( 8.700000000277906764, -15.94902145836247342, -35.53273252485295330 ) ) ;
#30295 = EDGE_LOOP ( 'NONE', ( #168, #28556, #23691, #14580 ) ) ;
#30296 = DIRECTION ( 'NONE',  ( -0.9880370573969197157, 0.1542166437529879364, 0.000000000000000000 ) ) ;
#30297 = CARTESIAN_POINT ( 'NONE',  ( 25.26809617030000155, 12.77001320659999983, 227.5999999999999943 ) ) ;
#30298 = B_SPLINE_CURVE_WITH_KNOTS ( 'NONE', 3,
 ( #4933, #2575, #2730, #21934, #28540, #24445 ),
 .UNSPECIFIED., .F., .F.,
 ( 4, 2, 4 ),
 ( 0.000000000000000000, 0.5000000000000000000, 1.000000000000000000 ),
 .UNSPECIFIED. ) ;
#30299 = CARTESIAN_POINT ( 'NONE',  ( 2.566301578609887279, -3.483224111942909040, -68.10000000002499121 ) ) ;
#30300 = DIRECTION ( 'NONE',  ( -1.000000000000000000, 0.000000000000000000, 0.000000000000000000 ) ) ;
#30301 = CARTESIAN_POINT ( 'NONE',  ( -4.278771218549574762, 1.040277833517747164, -44.10000000002499121 ) ) ;
#30302 =( NAMED_UNIT ( * ) SI_UNIT ( $, .STERADIAN. ) SOLID_ANGLE_UNIT ( ) );
#30303 = DIRECTION ( 'NONE',  ( -1.000000000000000000, 5.687698019339887572E-16, -6.771501495046482653E-12 ) ) ;
#30304 = DIRECTION ( 'NONE',  ( 0.6087614290101102110, -0.7775626432770559315, -0.1574987565968895831 ) ) ;
#30305 = CIRCLE ( 'NONE', #16724, 1.500000000000000222 ) ;
#30306 = CARTESIAN_POINT ( 'NONE',  ( -5.427432314178970429, 2.515719109140460041, -65.77526299442500601 ) ) ;
#30307 = ORIENTED_EDGE ( 'NONE', *, *, #19236, .T. ) ;
#30308 = CARTESIAN_POINT ( 'NONE',  ( 20.14371221788036692, 19.99999315982380210, 229.6128283330888848 ) ) ;
#30309 = B_SPLINE_CURVE_WITH_KNOTS ( 'NONE', 5,
 ( #28175, #11347, #18726, #22996, #30070, #30394 ),
 .UNSPECIFIED., .F., .F.,
 ( 6, 6 ),
 ( 0.000000000000000000, 2.893232387900000813 ),
 .UNSPECIFIED. ) ;
#30310 = ORIENTED_EDGE ( 'NONE', *, *, #16635, .T. ) ;
#30311 = CARTESIAN_POINT ( 'NONE',  ( -19.80526744909999692, 19.50877353739999975, 229.0000000010000178 ) ) ;
#30312 = ORIENTED_EDGE ( 'NONE', *, *, #5119, .F. ) ;
#30313 = CARTESIAN_POINT ( 'NONE',  ( -10.49243769149999927, -24.66097101990000340, -1.192453596599994725 ) ) ;
#30314 = ADVANCED_FACE ( 'NONE', ( #14516 ), #9941, .T. ) ;
#30315 = CARTESIAN_POINT ( 'NONE',  ( -7.797918471980000099, 19.99999999999999645, -43.60208152801600079 ) ) ;
#30316 = EDGE_CURVE ( 'NONE', #2709, #2704, #24113, .T. ) ;
#30317 = DIRECTION ( 'NONE',  ( 1.000000000000000000, 0.000000000000000000, 0.000000000000000000 ) ) ;
#30318 = DIRECTION ( 'NONE',  ( 1.595945597898660305E-12, 0.7071067811865475727, 0.7071067811865475727 ) ) ;
#30319 = CARTESIAN_POINT ( 'NONE',  ( -10.69999999999999929, -24.61475988249999958, -26.57332276320000020 ) ) ;
#30320 = CARTESIAN_POINT ( 'NONE',  ( -19.80535357377644701, 19.50875577052588739, 3.000000106999994642 ) ) ;
#30321 = CARTESIAN_POINT ( 'NONE',  ( -17.04621913067799710, -22.00000000000000000, -25.51324865357000249 ) ) ;
#30322 = ORIENTED_EDGE ( 'NONE', *, *, #6805, .T. ) ;
#30323 = CARTESIAN_POINT ( 'NONE',  ( 9.414213562409999625, -15.31419272936388687, -74.45223986426802298 ) ) ;
#30324 = AXIS2_PLACEMENT_3D ( 'NONE', #6636, #6331, #14043 ) ;
#30325 = CARTESIAN_POINT ( 'NONE',  ( 24.49999999589999788, -3.000285566359999846E-15, 190.0000000000000000 ) ) ;
#30326 = AXIS2_PLACEMENT_3D ( 'NONE', #31070, #9511, #16437 ) ;
#30327 = CARTESIAN_POINT ( 'NONE',  ( -28.49530731802708416, -0.5184832703812605192, 8.000000000000007105 ) ) ;
#30328 = CARTESIAN_POINT ( 'NONE',  ( -16.04158896040112126, -9.763537949678049443, 0.000000000000000000 ) ) ;
#30329 = CARTESIAN_POINT ( 'NONE',  ( -24.22223838309999877, -15.01863363589999878, 225.6808321819999890 ) ) ;
#30330 =( GEOMETRIC_REPRESENTATION_CONTEXT ( 3 ) GLOBAL_UNCERTAINTY_ASSIGNED_CONTEXT ( ( #10314 ) ) GLOBAL_UNIT_ASSIGNED_CONTEXT ( ( #12528, #18719, #10178 ) ) REPRESENTATION_CONTEXT ( 'NONE', 'WORKASPACE' ) );
#30331 = CARTESIAN_POINT ( 'NONE',  ( -10.82908725742657730, -27.76276047461854191, 86.78285841159998881 ) ) ;
#30332 = VECTOR ( 'NONE', #16652, 1000.000000000000000 ) ;
#30333 = CARTESIAN_POINT ( 'NONE',  ( 12.41983200457754322, 21.70000000000019469, -55.86851685976566273 ) ) ;
#30334 = FACE_OUTER_BOUND ( 'NONE', #22645, .T. ) ;
#30335 = CARTESIAN_POINT ( 'NONE',  ( -5.473571180597741836, 3.247285761689575168, -50.35267869292499654 ) ) ;
#30336 = CARTESIAN_POINT ( 'NONE',  ( 14.68395928812249807, -22.95674027903807257, -24.96087439630253968 ) ) ;
#30337 = DIRECTION ( 'NONE',  ( 0.9595496299847263710, -0.2815395311429191305, 0.000000000000000000 ) ) ;
#30338 = CARTESIAN_POINT ( 'NONE',  ( 3.303595366871416417, -1.277580108374672951, 230.8124249489373199 ) ) ;
#30339 = DIRECTION ( 'NONE',  ( 0.000000000000000000, -1.000000000000000000, 0.000000000000000000 ) ) ;
#30340 = EDGE_LOOP ( 'NONE', ( #12450, #11269, #9598, #5416 ) ) ;
#30341 = CARTESIAN_POINT ( 'NONE',  ( 0.07512830594655582617, -4.346272141329937888, -33.91110030500001216 ) ) ;
#30342 = AXIS2_PLACEMENT_3D ( 'NONE', #26127, #4257, #9 ) ;
#30343 = ORIENTED_EDGE ( 'NONE', *, *, #19157, .F. ) ;
#30344 = ADVANCED_FACE ( 'NONE', ( #12445 ), #19997, .F. ) ;
#30345 = CARTESIAN_POINT ( 'NONE',  ( -3.882843611323257615, 4.424263292022076577, -54.78587006832498219 ) ) ;
#30346 = VECTOR ( 'NONE', #2974, 1000.000000000000000 ) ;
#30347 = EDGE_LOOP ( 'NONE', ( #16398, #1561, #9557, #11215 ) ) ;
#30348 = CIRCLE ( 'NONE', #16767, 27.69999999999999929 ) ;
#30349 = EDGE_CURVE ( 'NONE', #19387, #8936, #6567, .T. ) ;
#30350 = APPLICATION_PROTOCOL_DEFINITION ( 'draft international standard', 'automotive_design', 1998, #21852 ) ;
#30351 = VECTOR ( 'NONE', #30267, 1000.000000000000000 ) ;
#30352 = VERTEX_POINT ( 'NONE', #19857 ) ;
#30353 = ORIENTED_EDGE ( 'NONE', *, *, #28804, .F. ) ;
#30354 = FACE_OUTER_BOUND ( 'NONE', #1116, .T. ) ;
#30355 = EDGE_CURVE ( 'NONE', #25829, #26031, #17476, .T. ) ;
#30356 = CARTESIAN_POINT ( 'NONE',  ( 4.041451884329999800, 2.220446049249999755E-16, 230.5235986622430175 ) ) ;
#30357 = CARTESIAN_POINT ( 'NONE',  ( -17.49227491161517278, -29.11870801639694406, -23.84973395190160161 ) ) ;
#30358 = CARTESIAN_POINT ( 'NONE',  ( -5.112571995710000650, -10.85828497149999983, 231.9999991140000191 ) ) ;
#30359 = CARTESIAN_POINT ( 'NONE',  ( -16.70716219490313392, -7.897520476984252191, -0.6999999999999784173 ) ) ;
#30360 = CARTESIAN_POINT ( 'NONE',  ( -2.825020644939634007, -4.425443225455641283, -0.6999999999999992895 ) ) ;
#30361 = CARTESIAN_POINT ( 'NONE',  ( -3.510061880997908279, 5.032561185093348044, -1.027651354100003633 ) ) ;
#30362 = FACE_OUTER_BOUND ( 'NONE', #20264, .T. ) ;
#30363 = CARTESIAN_POINT ( 'NONE',  ( 25.26019821377178687, -13.19871658671780246, 5.889015030805896167 ) ) ;
#30364 = CARTESIAN_POINT ( 'NONE',  ( 1.942707423728255778, -5.758494596869851989, -15.86414732020000784 ) ) ;
#30365 = CARTESIAN_POINT ( 'NONE',  ( 3.123710955063051298, -2.074832491810060020, -35.95875473020000612 ) ) ;
#30366 = AXIS2_PLACEMENT_3D ( 'NONE', #12481, #393, #4800 ) ;
#30367 = DIRECTION ( 'NONE',  ( 0.000000000000000000, 0.000000000000000000, 1.000000000000000000 ) ) ;
#30368 = EDGE_CURVE ( 'NONE', #21919, #10856, #1710, .T. ) ;
#30369 = CARTESIAN_POINT ( 'NONE',  ( 24.15916138403057190, 13.75451189100735050, 4.118302008711519413 ) ) ;
#30370 = CARTESIAN_POINT ( 'NONE',  ( 0.07063658732710000054, -28.50016343120000073, 223.9013487590000011 ) ) ;
#30371 = PRESENTATION_LAYER_ASSIGNMENT (  '', '', ( #8240 ) ) ;
#30372 = CARTESIAN_POINT ( 'NONE',  ( 21.99937703061004513, -17.24463697064632228, 8.000000000000007105 ) ) ;
#30373 = CARTESIAN_POINT ( 'NONE',  ( -2.952483221433048310, 1.886467326085379925, 227.6463841914517729 ) ) ;
#30374 = VECTOR ( 'NONE', #13376, 1000.000000000000000 ) ;
#30375 = VECTOR ( 'NONE', #2884, 1000.000000000000000 ) ;
#30376 = CIRCLE ( 'NONE', #9773, 4.000000004070001225 ) ;
#30377 = CARTESIAN_POINT ( 'NONE',  ( 23.16113320640637241, -13.48374052559371350, 226.0999999999989143 ) ) ;
#30378 = CARTESIAN_POINT ( 'NONE',  ( 8.700000000289733748, -15.05693637256081097, -37.86809127166881694 ) ) ;
#30379 = CARTESIAN_POINT ( 'NONE',  ( -17.80451178537096979, 11.53640331829313581, -4.336808689942018722E-16 ) ) ;
#30380 = EDGE_CURVE ( 'NONE', #5036, #20819, #22325, .T. ) ;
#30381 = FACE_OUTER_BOUND ( 'NONE', #8472, .T. ) ;
#30382 = ORIENTED_EDGE ( 'NONE', *, *, #2867, .T. ) ;
#30383 = CARTESIAN_POINT ( 'NONE',  ( -0.3083106916347965742, -3.499999999999999556, 227.6466876223823874 ) ) ;
#30384 = CARTESIAN_POINT ( 'NONE',  ( 9.799999999987905497, -15.94902145823454198, -35.53273252495090873 ) ) ;
#30385 = CARTESIAN_POINT ( 'NONE',  ( 1.100000000000000755, -26.77741585740001184, 4.902938919652013894 ) ) ;
#30386 =( GEOMETRIC_REPRESENTATION_CONTEXT ( 3 ) GLOBAL_UNCERTAINTY_ASSIGNED_CONTEXT ( ( #29179 ) ) GLOBAL_UNIT_ASSIGNED_CONTEXT ( ( #4494, #2136, #21329 ) ) REPRESENTATION_CONTEXT ( 'NONE', 'WORKASPACE' ) );
#30387 = VERTEX_POINT ( 'NONE', #12138 ) ;
#30388 = CARTESIAN_POINT ( 'NONE',  ( 3.248659393266396300, -2.157825791482658850, -43.75875473022500728 ) ) ;
#30389 = EDGE_LOOP ( 'NONE', ( #2274, #8420, #19475, #6849 ) ) ;
#30390 = AXIS2_PLACEMENT_3D ( 'NONE', #18160, #12834, #27765 ) ;
#30391 = VERTEX_POINT ( 'NONE', #26618 ) ;
#30392 = ORIENTED_EDGE ( 'NONE', *, *, #18259, .F. ) ;
#30393 = B_SPLINE_CURVE_WITH_KNOTS ( 'NONE', 5,
 ( #12329, #21936, #14856, #9971, #24285, #12473, #3033, #10127, #9815 ),
 .UNSPECIFIED., .F., .F.,
 ( 6, 3, 6 ),
 ( 0.000000000000000000, 2.405120303199999920, 3.339306056609999906 ),
 .UNSPECIFIED. ) ;
#30394 = CARTESIAN_POINT ( 'NONE',  ( 3.746497173757565413, -0.1670055334890632737, -35.69999999999999574 ) ) ;
#30395 = VECTOR ( 'NONE', #17473, 1000.000000000000114 ) ;
#30396 = VERTEX_POINT ( 'NONE', #14671 ) ;
#30398 = CARTESIAN_POINT ( 'NONE',  ( -24.60699806910000120, -12.93667933180000063, 225.0000014190000002 ) ) ;
#30397 = TOROIDAL_SURFACE ( 'NONE', #14806, 24.50000000000000000, 4.000000000000000000 ) ;
#30399 = LINE ( 'NONE', #26598, #1714 ) ;
#30400 = EDGE_CURVE ( 'NONE', #1828, #15932, #20848, .T. ) ;
#30401 = FACE_OUTER_BOUND ( 'NONE', #14139, .T. ) ;
#30402 = VECTOR ( 'NONE', #1423, 1000.000000000000000 ) ;
#30403 = CARTESIAN_POINT ( 'NONE',  ( -4.879522228196710110, 6.461977963245837842, -40.63088641039196602 ) ) ;
#30404 = DIRECTION ( 'NONE',  ( 1.000000000000000000, -0.000000000000000000, -3.489272357540000343E-15 ) ) ;
#30405 = CARTESIAN_POINT ( 'NONE',  ( -18.95046173579999760, -18.95046173579999760, -2.842170943039999687E-14 ) ) ;
#30406 = CARTESIAN_POINT ( 'NONE',  ( -2.020725942159999899, 3.500000000000000000, 230.8412452700000017 ) ) ;
#30407 = CARTESIAN_POINT ( 'NONE',  ( -0.9973419271877559389, -5.413498265897602302, -4.525234013000000388 ) ) ;
#30408 = CARTESIAN_POINT ( 'NONE',  ( -5.340187987486594068, -1.400932219821331870, -24.04656121680001135 ) ) ;
#30409 = FACE_OUTER_BOUND ( 'NONE', #24383, .T. ) ;
#30410 = CIRCLE ( 'NONE', #14822, 26.80000000000000071 ) ;
#30411 = CARTESIAN_POINT ( 'NONE',  ( 3.472061922019873403, -0.4504971303802423610, -91.21022354329026882 ) ) ;
#30412 = ADVANCED_FACE ( 'NONE', ( #27688 ), #1114, .F. ) ;
#30413 = CARTESIAN_POINT ( 'NONE',  ( 18.00000000000000000, 0.000000000000000000, 230.6412452697800006 ) ) ;
#30414 = CARTESIAN_POINT ( 'NONE',  ( 7.000000000115440102, -60.75400889061052112, -3.446705952631804681 ) ) ;
#30415 = CARTESIAN_POINT ( 'NONE',  ( 26.80000000000000071, 7.105427357599999217E-15, 0.000000000000000000 ) ) ;
#30416 = EDGE_CURVE ( 'NONE', #15903, #21635, #4744, .T. ) ;
#30417 = CARTESIAN_POINT ( 'NONE',  ( 20.64716981389999972, -20.77933506589999979, 229.0000000000000000 ) ) ;
#30418 = CARTESIAN_POINT ( 'NONE',  ( 0.9758793681798838549, -27.78334643822867633, 6.002515439000016606 ) ) ;
#30419 = CARTESIAN_POINT ( 'NONE',  ( -26.22090100435761784, -5.650641260081752826, -1.399999999999999023 ) ) ;
#30420 = ORIENTED_EDGE ( 'NONE', *, *, #7023, .T. ) ;
#30421 = CARTESIAN_POINT ( 'NONE',  ( -1.494970809075166329, -6.161113191638062148, -61.94311227092499195 ) ) ;
#30422 = FACE_OUTER_BOUND ( 'NONE', #14981, .T. ) ;
#30423 = ORIENTED_EDGE ( 'NONE', *, *, #17874, .T. ) ;
#30424 = CIRCLE ( 'NONE', #16762, 27.92857142840000151 ) ;
#30425 = EDGE_LOOP ( 'NONE', ( #9847, #16785, #28441, #24084 ) ) ;
#30426 = EDGE_CURVE ( 'NONE', #28570, #16475, #20293, .T. ) ;
#30427 = CARTESIAN_POINT ( 'NONE',  ( -26.11394584979204225, -6.088596733047862308, 93.21714158835003161 ) ) ;
#30428 = CARTESIAN_POINT ( 'NONE',  ( -4.555585884337687297, -4.059738318096004939, -24.84101932450000305 ) ) ;
#30429 = ORIENTED_EDGE ( 'NONE', *, *, #4678, .F. ) ;
#30430 = LINE ( 'NONE', #13899, #4795 ) ;
#30431 = CARTESIAN_POINT ( 'NONE',  ( -2.098441946322436635, -3.287561928151557122, -68.10000000002500542 ) ) ;
#30432 = EDGE_LOOP ( 'NONE', ( #20508, #12828, #29987, #12723 ) ) ;
#30433 = EDGE_LOOP ( 'NONE', ( #8175, #19202, #10725, #6653 ) ) ;
#30434 = ORIENTED_EDGE ( 'NONE', *, *, #30577, .F. ) ;
#30435 = ORIENTED_EDGE ( 'NONE', *, *, #3129, .T. ) ;
#30436 = CARTESIAN_POINT ( 'NONE',  ( -12.30000000018107009, -28.61158073718687689, -31.19611644274446149 ) ) ;
#30437 = EDGE_CURVE ( 'NONE', #6463, #16921, #10559, .T. ) ;
#30438 = CIRCLE ( 'NONE', #1272, 1.099999999570000497 ) ;
#30439 = CARTESIAN_POINT ( 'NONE',  ( -4.884981308350000102E-15, -2.100000000000000089, 226.6412452697800006 ) ) ;
#30440 = CARTESIAN_POINT ( 'NONE',  ( 4.117846205589234643, 1.989599136607407504, -66.85315453642499506 ) ) ;
#30441 = CARTESIAN_POINT ( 'NONE',  ( 24.50094951250000008, -14.04160150939999951, 230.0000000000000000 ) ) ;
#30442 = LINE ( 'NONE', #18467, #8618 ) ;
#30443 = CARTESIAN_POINT ( 'NONE',  ( 19.20441074659999714, -21.26949966540000148, 222.0000000000000000 ) ) ;
#30444 = DIRECTION ( 'NONE',  ( 0.7730139489027949562, -0.6343890248118320141, 0.000000000000000000 ) ) ;
#30445 = EDGE_LOOP ( 'NONE', ( #30096, #9243, #27395, #18647 ) ) ;
#30446 = EDGE_CURVE ( 'NONE', #14782, #20501, #6135, .T. ) ;
#30447 = CARTESIAN_POINT ( 'NONE',  ( -22.63996212553987064, -14.34127312896723971, 225.1459679062982673 ) ) ;
#30448 = CARTESIAN_POINT ( 'NONE',  ( -1.184025259985578948, -4.532227402022654061, -12.05022317840000845 ) ) ;
#30449 = CARTESIAN_POINT ( 'NONE',  ( 14.76964124820000102, 19.99999999999999645, -1.399999999999998579 ) ) ;
#30450 = CARTESIAN_POINT ( 'NONE',  ( -10.69999999969433269, -30.11701243199135902, -29.23701053811106476 ) ) ;
#30451 = ORIENTED_EDGE ( 'NONE', *, *, #29103, .F. ) ;
#30452 = DIRECTION ( 'NONE',  ( 0.000000000000000000, -0.3420201433259318913, 0.9396926207858126157 ) ) ;
#30453 = CARTESIAN_POINT ( 'NONE',  ( -1.127665019380000189, -28.47796022459999676, 225.0000014190000002 ) ) ;
#30454 = CARTESIAN_POINT ( 'NONE',  ( 28.50000000000000000, -1.056438886989999914E-13, 222.0000000000000000 ) ) ;
#30455 = CARTESIAN_POINT ( 'NONE',  ( 27.08859402333795785, 0.4928875713623736554, 0.02487529600000981667 ) ) ;
#30456 = CARTESIAN_POINT ( 'NONE',  ( 22.63992238019999803, -14.34133587289999845, 5.000000000000000000 ) ) ;
#30457 = B_SPLINE_CURVE_WITH_KNOTS ( 'NONE', 3,
 ( #11380, #30102, #13580, #20821, #23506, #30582, #25229, #9009, #6648, #23031 ),
 .UNSPECIFIED., .F., .F.,
 ( 4, 2, 2, 2, 4 ),
 ( 0.000000000000000000, 0.2500000000000000000, 0.5000000000000000000, 0.7500000000000000000, 1.000000000000000000 ),
 .UNSPECIFIED. ) ;
#30458 = CARTESIAN_POINT ( 'NONE',  ( -2.158984558600606007, 5.217364672555318883, -57.14652090042499566 ) ) ;
#30459 = FACE_OUTER_BOUND ( 'NONE', #4681, .T. ) ;
#30460 = CARTESIAN_POINT ( 'NONE',  ( -4.084346732781014566, 1.529807325146986807, -38.22530605782345958 ) ) ;
#30461 = EDGE_LOOP ( 'NONE', ( #30546, #3631, #5216, #9750 ) ) ;
#30462 = PRESENTATION_STYLE_ASSIGNMENT (( #20864 ) ) ;
#30463 = CARTESIAN_POINT ( 'NONE',  ( 8.350000000381330167, -5.981227587133004064, -27.94042817442931792 ) ) ;
#30464 = CARTESIAN_POINT ( 'NONE',  ( 1.201297883400354261, -3.884613871942808050, -68.10000000002501963 ) ) ;
#30465 = B_SPLINE_CURVE_WITH_KNOTS ( 'NONE', 3,
 ( #430, #116, #17084, #4976, #7638, #9695, #22276, #17235 ),
 .UNSPECIFIED., .F., .F.,
 ( 4, 2, 2, 4 ),
 ( 0.000000000000000000, 0.2500000000000001665, 0.5000000000000003331, 1.000000000000000000 ),
 .UNSPECIFIED. ) ;
#30466 = CARTESIAN_POINT ( 'NONE',  ( 14.00000000000000000, 20.99999999999999645, -62.80809897700000022 ) ) ;
#30467 = CARTESIAN_POINT ( 'NONE',  ( -4.335682707025502403, 1.120073662811198689, -44.10000000002499121 ) ) ;
#30468 = ORIENTED_EDGE ( 'NONE', *, *, #6531, .T. ) ;
#30469 = CARTESIAN_POINT ( 'NONE',  ( 27.76135143639999825, -3.399672735949999729E-15, 37.66141409829999986 ) ) ;
#30470 = EDGE_CURVE ( 'NONE', #3623, #18002, #13062, .T. ) ;
#30471 = CARTESIAN_POINT ( 'NONE',  ( 1.082264403401735020, -4.420062499635217357, -64.70397119102501904 ) ) ;
#30472 = VERTEX_POINT ( 'NONE', #25031 ) ;
#30473 = DIRECTION ( 'NONE',  ( 0.9316362575375349842, -0.3633921898465292122, 0.000000000000000000 ) ) ;
#30474 = ADVANCED_FACE ( 'NONE', ( #3785 ), #7527, .T. ) ;
#30475 = ORIENTED_EDGE ( 'NONE', *, *, #7893, .T. ) ;
#30476 = EDGE_CURVE ( 'NONE', #5911, #27858, #21325, .T. ) ;
#30477 = CARTESIAN_POINT ( 'NONE',  ( -27.11420065481265951, -7.632847749032011464, 0.08279779300002232389 ) ) ;
#30478 = EDGE_CURVE ( 'NONE', #11286, #26133, #30605, .T. ) ;
#30479 = VERTEX_POINT ( 'NONE', #16900 ) ;
#30480 = CARTESIAN_POINT ( 'NONE',  ( 10.60826873110000079, -25.00000000000000000, -1.605882352700004123 ) ) ;
#30481 = B_SPLINE_CURVE_WITH_KNOTS ( 'NONE', 5,
 ( #5095, #17515, #3344, #20187, #852, #21945 ),
 .UNSPECIFIED., .F., .F.,
 ( 6, 6 ),
 ( 65.40639850639999509, 88.32365686489998780 ),
 .UNSPECIFIED. ) ;
#30482 = CARTESIAN_POINT ( 'NONE',  ( -23.29312071521372118, -15.17488101142239643, 4.493007575000013354 ) ) ;
#30483 = CARTESIAN_POINT ( 'NONE',  ( 27.54391552379999908, -3.373045395939999845E-15, 42.95625301639999805 ) ) ;
#30484 = CARTESIAN_POINT ( 'NONE',  ( -15.73360964037622622, -8.979988381802643360, -0.6999999989999727834 ) ) ;
#30485 = UNCERTAINTY_MEASURE_WITH_UNIT (LENGTH_MEASURE( 1.000000000000000082E-05 ), #24196, 'distance_accuracy_value', 'NONE');
#30486 = CARTESIAN_POINT ( 'NONE',  ( 0.4368970292349217965, -27.79681690464249044, 3.901345920999998995 ) ) ;
#30487 = CARTESIAN_POINT ( 'NONE',  ( -16.81341597784800967, -10.09981795476353739, 0.000000000000000000 ) ) ;
#30488 = CARTESIAN_POINT ( 'NONE',  ( -22.97593529893700648, 15.65128280014837081, 8.000000000000007105 ) ) ;
#30489 = ORIENTED_EDGE ( 'NONE', *, *, #8678, .T. ) ;
#30490 = FACE_OUTER_BOUND ( 'NONE', #30263, .T. ) ;
#30491 = CARTESIAN_POINT ( 'NONE',  ( -8.699999999718343702, -24.19750589173278499, -27.32947359979484858 ) ) ;
#30492 = DIRECTION ( 'NONE',  ( 1.000000000000000000, 0.000000000000000000, 0.000000000000000000 ) ) ;
#30493 = CARTESIAN_POINT ( 'NONE',  ( -17.93302393987574206, -8.945477793833122249, 0.000000000000000000 ) ) ;
#30494 = CARTESIAN_POINT ( 'NONE',  ( -10.69999999999999929, -27.00000000000000000, -28.40000000000000213 ) ) ;
#30495 = CARTESIAN_POINT ( 'NONE',  ( -0.8259893078309999970, -28.48844349870000059, 225.7596419580000315 ) ) ;
#30496 = DIRECTION ( 'NONE',  ( 0.000000000000000000, 0.000000000000000000, -1.000000000000000000 ) ) ;
#30497 = CARTESIAN_POINT ( 'NONE',  ( -15.96459051028835674, -8.309720466557573459, -0.6999999999999784173 ) ) ;
#30498 = CARTESIAN_POINT ( 'NONE',  ( -0.7556487780321572423, 4.453147011089724217, -51.25792092402500089 ) ) ;
#30499 = CARTESIAN_POINT ( 'NONE',  ( -23.70578532278555528, -13.93854223031271999, 6.087706803517302312 ) ) ;
#30500 = CARTESIAN_POINT ( 'NONE',  ( -20.19118766868406212, 19.99999867976873702, 229.5201436231253354 ) ) ;
#30501 = FACE_OUTER_BOUND ( 'NONE', #27903, .T. ) ;
#30502 = LINE ( 'NONE', #13973, #9738 ) ;
#30503 = ORIENTED_EDGE ( 'NONE', *, *, #20477, .F. ) ;
#30504 = CARTESIAN_POINT ( 'NONE',  ( 4.051823674760409943, -0.6775361292690254000, -35.74517599850000948 ) ) ;
#30505 = ORIENTED_EDGE ( 'NONE', *, *, #23099, .F. ) ;
#30506 = CARTESIAN_POINT ( 'NONE',  ( 2.752605500610148859, 3.655072764496607007, -54.62619010302499589 ) ) ;
#30507 = ORIENTED_EDGE ( 'NONE', *, *, #2509, .T. ) ;
#30508 = APPLICATION_PROTOCOL_DEFINITION ( 'draft international standard', 'automotive_design', 1998, #15825 ) ;
#30509 = EDGE_LOOP ( 'NONE', ( #9356, #15155 ) ) ;
#30510 = DIRECTION ( 'NONE',  ( -1.000000000000000000, 0.000000000000000000, 0.000000000000000000 ) ) ;
#30511 = PRODUCT ( 'Rivet', 'Rivet', '', ( #17447 ) ) ;
#30512 = ADVANCED_FACE ( 'NONE', ( #26505 ), #19295, .F. ) ;
#30513 = ORIENTED_EDGE ( 'NONE', *, *, #7721, .F. ) ;
#30514 = CARTESIAN_POINT ( 'NONE',  ( -10.69999999999999929, -24.00000000000000000, -28.40000000000000213 ) ) ;
#30515 = CARTESIAN_POINT ( 'NONE',  ( 2.100000000000000089, -1.998401444330000344E-15, 226.6412452697800006 ) ) ;
#30516 = CARTESIAN_POINT ( 'NONE',  ( -23.55406855550000245, 16.04544956020000157, 222.0000000000000000 ) ) ;
#30517 = VECTOR ( 'NONE', #25597, 1000.000000000000000 ) ;
#30518 = CARTESIAN_POINT ( 'NONE',  ( -23.55406855550000245, 16.04544956020000157, 222.0000000000000000 ) ) ;
#30519 = CARTESIAN_POINT ( 'NONE',  ( -18.95046173589999938, -18.95046173589999938, 230.0000000000000000 ) ) ;
#30520 = CARTESIAN_POINT ( 'NONE',  ( 8.699999999551790708, -9.149979919791583427, -35.02638174844071983 ) ) ;
#30521 = CARTESIAN_POINT ( 'NONE',  ( -6.505526340832360255, -0.4164809035307331930, -3.548838774899996995 ) ) ;
#30522 = CARTESIAN_POINT ( 'NONE',  ( -23.57419247189999822, -20.83845762109999811, 229.7625741969999922 ) ) ;
#30523 = ORIENTED_EDGE ( 'NONE', *, *, #28904, .T. ) ;
#30524 = LINE ( 'NONE', #3924, #2942 ) ;
#30525 = CARTESIAN_POINT ( 'NONE',  ( -3.057389860650357338, 5.459897439232808125, -16.67761783620000315 ) ) ;
#30526 = CARTESIAN_POINT ( 'NONE',  ( 3.996952828541906033, 3.843200228390037498, -34.32341724620000889 ) ) ;
#30527 = CARTESIAN_POINT ( 'NONE',  ( 23.96481830933180035, 14.09066012006225854, 3.927868778737001243 ) ) ;
#30528 = CARTESIAN_POINT ( 'NONE',  ( -19.29841003509485375, 19.63499152630128108, 0.3044381840000276451 ) ) ;
#30529 = CARTESIAN_POINT ( 'NONE',  ( -10.23626208557738515, -26.01105658336103943, 8.000000000000007105 ) ) ;
#30530 = CARTESIAN_POINT ( 'NONE',  ( -17.43404799080784429, -28.61456981395415511, -33.24133037538724267 ) ) ;
#30531 = B_SPLINE_SURFACE_WITH_KNOTS ( 'NONE', 5, 5, ( 
 ( #6033, #19904, #3672, #20361, #20202, #27135, #22575, #8544, #29954 ),
 ( #3840, #29794, #27437, #25407, #8382, #5569, #8226, #5873, #13272 ),
 ( #15483, #15170, #10308, #23046, #13428, #22885, #29486, #1327, #18144 ),
 ( #17528, #6194, #15795, #7925, #24775, #12818, #22422, #11231, #6508 ),
 ( #23362, #1642, #16108, #6820, #18930, #18619, #20836, #1490, #28217 ),
 ( #16569, #28380, #20677, #21145, #9170, #23199, #16416, #25877, #18772 ),
 ( #30441, #11698, #25720, #28064, #2104, #23670, #1952, #13748, #4153 ),
 ( #14218, #25560, #11081, #27914, #8861, #1801, #8701, #21299, #9021 ),
 ( #30273, #18309, #3997, #30901, #30740, #26175, #15952, #13908, #13594 ) ),
 .UNSPECIFIED., .F., .F., .F.,
 ( 6, 3, 6 ),
 ( 6, 3, 6 ),
 ( 0.000000000000000000, 53.20205529499999386, 91.13698440880000362 ),
 ( 8.011061266649999624, 8.831591450809998634, 9.652121634960000307 ),
 .UNSPECIFIED. ) ;
#30532 = CARTESIAN_POINT ( 'NONE',  ( 27.21969913503883731, 9.853839689487985609, 0.2374258030000131470 ) ) ;
#30533 = CARTESIAN_POINT ( 'NONE',  ( -23.63627835177424075, -12.63201688151322699, 4.333923913749079482 ) ) ;
#30534 = CARTESIAN_POINT ( 'NONE',  ( -22.03724970760471180, 17.02913761663678827, 6.333333369000054169 ) ) ;
#30535 = EDGE_CURVE ( 'NONE', #14788, #27320, #9739, .T. ) ;
#30536 = AXIS2_PLACEMENT_3D ( 'NONE', #12541, #22149, #27329 ) ;
#30537 = CARTESIAN_POINT ( 'NONE',  ( 24.50000001620000134, -3.000285568839999855E-15, 189.9999999960000139 ) ) ;
#30538 = VERTEX_POINT ( 'NONE', #12033 ) ;
#30539 = VECTOR ( 'NONE', #22003, 1000.000000000000000 ) ;
#30540 = CARTESIAN_POINT ( 'NONE',  ( 7.000000000115440102, -60.75400889061052112, -3.446705952631804681 ) ) ;
#30541 = CARTESIAN_POINT ( 'NONE',  ( -10.88910015670000142, 20.99999999999999645, -56.10000000020000499 ) ) ;
#30542 = CARTESIAN_POINT ( 'NONE',  ( 10.00000000070000183, -43.95328087560000085, -27.24755286599999948 ) ) ;
#30543 = ORIENTED_EDGE ( 'NONE', *, *, #28604, .T. ) ;
#30544 = CARTESIAN_POINT ( 'NONE',  ( 8.903108651239925564, -22.82508830966962421, 40.00000000000000000 ) ) ;
#30545 = ORIENTED_EDGE ( 'NONE', *, *, #815, .T. ) ;
#30546 = ORIENTED_EDGE ( 'NONE', *, *, #20838, .F. ) ;
#30547 = EDGE_LOOP ( 'NONE', ( #30066, #3320, #14524, #11844 ) ) ;
#30548 = DIRECTION ( 'NONE',  ( 0.000000000000000000, 0.000000000000000000, -1.000000000000000000 ) ) ;
#30549 = ORIENTED_EDGE ( 'NONE', *, *, #24471, .F. ) ;
#30550 = LINE ( 'NONE', #30227, #7525 ) ;
#30551 = CARTESIAN_POINT ( 'NONE',  ( 23.69427943123108093, 14.54081805611945910, 3.920145809000019632 ) ) ;
#30552 = CARTESIAN_POINT ( 'NONE',  ( 10.69999999999999929, -130.0000000000000000, -41.24671599790000442 ) ) ;
#30553 = CARTESIAN_POINT ( 'NONE',  ( -10.00000000050000004, -27.56998452010000022, -25.39999999999999858 ) ) ;
#30554 = CARTESIAN_POINT ( 'NONE',  ( 2.115765021644385069, -4.593406295380427551, -94.17120874163683197 ) ) ;
#30555 = AXIS2_PLACEMENT_3D ( 'NONE', #3052, #14876, #17524 ) ;
#30556 = CARTESIAN_POINT ( 'NONE',  ( 26.57440914490000239, -3.469982507400000582, -1.399999999999998579 ) ) ;
#30557 = CARTESIAN_POINT ( 'NONE',  ( -10.69999999997255991, -29.40012576568826574, -30.24240556185885254 ) ) ;
#30558 = EDGE_CURVE ( 'NONE', #22416, #18028, #9979, .T. ) ;
#30559 = CARTESIAN_POINT ( 'NONE',  ( -19.90459424020000156, 20.00000653480000068, 229.9504594400000030 ) ) ;
#30560 = ORIENTED_EDGE ( 'NONE', *, *, #7464, .T. ) ;
#30561 = AXIS2_PLACEMENT_3D ( 'NONE', #27399, #24731, #13072 ) ;
#30562 = CARTESIAN_POINT ( 'NONE',  ( -0.7873752056533345201, -4.273814420472608511, -3.525234013000005717 ) ) ;
#30563 = CARTESIAN_POINT ( 'NONE',  ( -3.253989917302559043, -2.899813084402115049, -24.84101932450000305 ) ) ;
#30564 = CARTESIAN_POINT ( 'NONE',  ( 14.40197535836999876, -26.99999999999984368, -34.17350269180000311 ) ) ;
#30565 = CIRCLE ( 'NONE', #16981, 18.00000000000000000 ) ;
#30566 = CARTESIAN_POINT ( 'NONE',  ( 23.35113490838396189, -13.15228900088872521, 226.0721256962708878 ) ) ;
#30567 = CARTESIAN_POINT ( 'NONE',  ( 0.8978302376703681809, 3.499838689518511625, 227.7116136946774247 ) ) ;
#30568 = CARTESIAN_POINT ( 'NONE',  ( -25.07525407549810836, 13.54704386626776547, 6.073823031254199201 ) ) ;
#30569 = CARTESIAN_POINT ( 'NONE',  ( -23.52673845780000050, -14.81058795080000046, 225.3106464589999973 ) ) ;
#30570 = CARTESIAN_POINT ( 'NONE',  ( 24.32472724076343695, -13.45989056521276872, 6.099998581000020792 ) ) ;
#30571 = DIRECTION ( 'NONE',  ( 0.000000000000000000, 0.000000000000000000, 1.000000000000000000 ) ) ;
#30572 = CARTESIAN_POINT ( 'NONE',  ( 0.000000000000000000, 0.000000000000000000, 0.000000000000000000 ) ) ;
#30573 = VERTEX_POINT ( 'NONE', #2590 ) ;
#30574 = CARTESIAN_POINT ( 'NONE',  ( -4.240613917342964889, -1.711409762446096439, -58.98491726642500055 ) ) ;
#30575 = DIRECTION ( 'NONE',  ( 0.000000000000000000, 0.000000000000000000, 1.000000000000000000 ) ) ;
#30576 = ORIENTED_EDGE ( 'NONE', *, *, #10797, .T. ) ;
#30577 = EDGE_CURVE ( 'NONE', #29133, #1473, #5067, .T. ) ;
#30578 = ORIENTED_EDGE ( 'NONE', *, *, #3926, .F. ) ;
#30579 = CARTESIAN_POINT ( 'NONE',  ( 1.814857447021396585E-10, -110.9401521129946389, -1.050525799519145487 ) ) ;
#30580 = CARTESIAN_POINT ( 'NONE',  ( 4.657610845611275252, 3.324676482552371581, -35.37908769469999726 ) ) ;
#30581 = ORIENTED_EDGE ( 'NONE', *, *, #11958, .T. ) ;
#30582 = CARTESIAN_POINT ( 'NONE',  ( -23.99220715881088495, 14.04440917687116475, 4.117401770955998686 ) ) ;
#30583 = DIRECTION ( 'NONE',  ( 0.7071067811834158556, -0.6355433650310500227, 0.3099752105724556395 ) ) ;
#30584 = VERTEX_POINT ( 'NONE', #16096 ) ;
#30585 = ORIENTED_EDGE ( 'NONE', *, *, #21872, .F. ) ;
#30586 = ORIENTED_EDGE ( 'NONE', *, *, #18429, .F. ) ;
#30587 = ORIENTED_EDGE ( 'NONE', *, *, #20089, .F. ) ;
#30588 = CARTESIAN_POINT ( 'NONE',  ( 24.81746042555073117, -14.01353061617342455, 6.079865098000015067 ) ) ;
#30589 = AXIS2_PLACEMENT_3D ( 'NONE', #23604, #26419, #7059 ) ;
#30590 = DIRECTION ( 'NONE',  ( 1.000000000000000000, 0.000000000000000000, 0.000000000000000000 ) ) ;
#30591 = EDGE_CURVE ( 'NONE', #27477, #18256, #18454, .T. ) ;
#30592 = CARTESIAN_POINT ( 'NONE',  ( -4.617404660156336327, 1.522451704138575668, -67.99019511502500279 ) ) ;
#30593 = CARTESIAN_POINT ( 'NONE',  ( 28.50000000000000000, 1.065814103639999922E-14, 229.0000000000000000 ) ) ;
#30594 = ADVANCED_FACE ( 'NONE', ( #3985 ), #18132, .T. ) ;
#30595 = B_SPLINE_CURVE_WITH_KNOTS ( 'NONE', 3,
 ( #22967, #20139, #20598, #22806, #10854, #30037, #27832, #1414, #29884, #6435, #30196, #6283, #10689, #15884, #20283, #25487, #3923, #13517 ),
 .UNSPECIFIED., .F., .F.,
 ( 4, 2, 2, 2, 2, 2, 2, 2, 4 ),
 ( 0.000000000000000000, 0.1250000000000000000, 0.2500000000000000000, 0.3750000000000000000, 0.5000000000000000000, 0.6250000000000000000, 0.7500000000000000000, 0.8750000000000000000, 1.000000000000000000 ),
 .UNSPECIFIED. ) ;
#30596 = CARTESIAN_POINT ( 'NONE',  ( -18.87720858757026576, 21.16361474422994604, 0.2374258030000131470 ) ) ;
#30597 = CARTESIAN_POINT ( 'NONE',  ( -12.43585889439999903, -25.03430743100000200, 222.0000000000000000 ) ) ;
#30598 = CARTESIAN_POINT ( 'NONE',  ( -17.40441589016016266, -23.42021493853068037, -24.69329539672489204 ) ) ;
#30599 = ORIENTED_EDGE ( 'NONE', *, *, #27, .F. ) ;
#30600 = CARTESIAN_POINT ( 'NONE',  ( -20.06472444662395560, 19.99998854834754525, 0.2590520886679497647 ) ) ;
#30601 = VECTOR ( 'NONE', #650, 1000.000000000000000 ) ;
#30602 = EDGE_CURVE ( 'NONE', #18191, #30960, #25548, .T. ) ;
#30603 = CARTESIAN_POINT ( 'NONE',  ( -4.335484423225056005, -2.064402852395420318, -12.03905742010000246 ) ) ;
#30604 = CARTESIAN_POINT ( 'NONE',  ( 5.114250173089999407, 17.43050732989999929, 230.0000000000000000 ) ) ;
#30605 = B_SPLINE_CURVE_WITH_KNOTS ( 'NONE', 3,
 ( #23696, #24297, #19582, #14709, #17058, #21480, #21788, #16739, #26053, #26203 ),
 .UNSPECIFIED., .F., .F.,
 ( 4, 2, 2, 2, 4 ),
 ( 0.000000000000000000, 0.2499999999999996669, 0.4999999999999993339, 0.7499999999999996669, 1.000000000000000000 ),
 .UNSPECIFIED. ) ;
#30606 = CARTESIAN_POINT ( 'NONE',  ( 12.18129165770028166, -1.906344006863165630, 232.6627636338612888 ) ) ;
#30607 = ORIENTED_EDGE ( 'NONE', *, *, #18793, .T. ) ;
#30608 = CARTESIAN_POINT ( 'NONE',  ( 26.75124393581684146, 1.948321199505564705, -1.399999999999998801 ) ) ;
#30609 = FACE_OUTER_BOUND ( 'NONE', #13285, .T. ) ;
#30610 = CARTESIAN_POINT ( 'NONE',  ( -8.699999999684971286, -15.55237326750320825, -33.04280034228838048 ) ) ;
#30611 = CARTESIAN_POINT ( 'NONE',  ( 7.000000000000000000, -15.86465192213301556, -74.65259062561435144 ) ) ;
#30612 = B_SPLINE_CURVE_WITH_KNOTS ( 'NONE', 3,
 ( #21816, #4830, #6712, #9223, #18982, #14274, #11747, #6865, #7341, #19143, #2008 ),
 .UNSPECIFIED., .F., .F.,
 ( 4, 1, 1, 1, 2, 2, 4 ),
 ( 0.000000000000000000, 0.2500000000000190958, 0.3750000000000267564, 0.4375000000000288658, 0.4687500000000298095, 0.5000000000000307532, 1.000000000000000000 ),
 .UNSPECIFIED. ) ;
#30613 = CARTESIAN_POINT ( 'NONE',  ( 22.92405521622628939, -13.88330634250967144, 4.042547418791329505 ) ) ;
#30614 = CARTESIAN_POINT ( 'NONE',  ( -1.293561172433232986, -6.216321778783836294, -52.92706695232499925 ) ) ;
#30615 = ADVANCED_FACE ( 'NONE', ( #16247 ), #9010, .T. ) ;
#30616 = CARTESIAN_POINT ( 'NONE',  ( 5.638687372243864182, -5.597492073914120070, -34.74908987243544090 ) ) ;
#30617 = CARTESIAN_POINT ( 'NONE',  ( 16.19686700502921539, 11.53824530203521448, -0.6999999999999785283 ) ) ;
#30618 = EDGE_LOOP ( 'NONE', ( #19552, #14368 ) ) ;
#30619 =( NAMED_UNIT ( * ) SI_UNIT ( $, .STERADIAN. ) SOLID_ANGLE_UNIT ( ) );
#30620 = CARTESIAN_POINT ( 'NONE',  ( -28.49999999970000175, 7.466149641070000342, 229.0000000000000000 ) ) ;
#30621 = CARTESIAN_POINT ( 'NONE',  ( 2.743523579834141746, -3.445032478160675371, -68.10000000002501963 ) ) ;
#30622 = EDGE_CURVE ( 'NONE', #9238, #27093, #1791, .T. ) ;
#30623 = CARTESIAN_POINT ( 'NONE',  ( 0.2188333036866983439, 2.694277338339796657, -67.89769279494433363 ) ) ;
#30624 = CARTESIAN_POINT ( 'NONE',  ( -4.094000917768401138, -0.2590052599951323531, -44.10000000002498410 ) ) ;
#30625 = ORIENTED_EDGE ( 'NONE', *, *, #6230, .T. ) ;
#30626 = DIRECTION ( 'NONE',  ( 0.000000000000000000, 0.000000000000000000, -1.000000000000000000 ) ) ;
#30627 = CARTESIAN_POINT ( 'NONE',  ( 1.415268835064556363, -5.780081730213937341, -64.70397119102500483 ) ) ;
#30628 = ORIENTED_EDGE ( 'NONE', *, *, #18161, .F. ) ;
#30629 = CARTESIAN_POINT ( 'NONE',  ( 24.73369734551975085, -12.69281744145431290, 4.322410792677205293 ) ) ;
#30630 = CIRCLE ( 'NONE', #3471, 4.276011752367109509 ) ;
#30631 = EDGE_CURVE ( 'NONE', #16796, #14059, #25709, .T. ) ;
#30632 = CARTESIAN_POINT ( 'NONE',  ( -27.39555917266975982, -7.712052243925962891, 0.2686740700000300741 ) ) ;
#30633 = ORIENTED_EDGE ( 'NONE', *, *, #20031, .F. ) ;
#30634 = CARTESIAN_POINT ( 'NONE',  ( -5.899424784609999861, -0.1656472027220000087, 226.6412452697800006 ) ) ;
#30635 = AXIS2_PLACEMENT_3D ( 'NONE', #17495, #682, #5231 ) ;
#30636 = DIRECTION ( 'NONE',  ( 0.000000000000000000, 0.000000000000000000, -1.000000000000000000 ) ) ;
#30637 = LINE ( 'NONE', #15844, #9472 ) ;
#30638 = CARTESIAN_POINT ( 'NONE',  ( -1.758512962375676780, 3.081546181689937658, 0.000000000000000000 ) ) ;
#30639 = CARTESIAN_POINT ( 'NONE',  ( 0.03549436698350039859, -27.80040766163043031, 3.997479608999987555 ) ) ;
#30640 = CARTESIAN_POINT ( 'NONE',  ( -7.861312627708255896, 2.804450004377710304, -42.18479665268674950 ) ) ;
#30641 = LINE ( 'NONE', #23714, #11522 ) ;
#30642 = ORIENTED_EDGE ( 'NONE', *, *, #8473, .F. ) ;
#30643 = CARTESIAN_POINT ( 'NONE',  ( 8.000000000277404766, -5.572998883593017538, -27.02754848640722329 ) ) ;
#30644 = CARTESIAN_POINT ( 'NONE',  ( 3.063879268240000009, 1.673804873600000187, 230.8412452700000017 ) ) ;
#30645 = CARTESIAN_POINT ( 'NONE',  ( 2.382250895449999906, 11.80689512960000087, 231.9999989789999972 ) ) ;
#30646 = CARTESIAN_POINT ( 'NONE',  ( -2.590102362109455658, -2.513801395391271676, 230.7730491447685210 ) ) ;
#30647 = CYLINDRICAL_SURFACE ( 'NONE', #9138, 1.000000000000001110 ) ;
#30648 = CARTESIAN_POINT ( 'NONE',  ( 2.525646774360000180, -11.92010449670000050, 230.6412452697800006 ) ) ;
#30649 = EDGE_CURVE ( 'NONE', #4540, #24004, #23472, .T. ) ;
#30650 = CARTESIAN_POINT ( 'NONE',  ( -16.06988921239048551, -8.208160914692745891, -0.6999999989999727834 ) ) ;
#30651 = CARTESIAN_POINT ( 'NONE',  ( -2.020725942159999899, -3.500000000000000000, 230.8412452700000017 ) ) ;
#30652 = CARTESIAN_POINT ( 'NONE',  ( 5.782578939028539367, 2.564649547393091478, -51.87998794302499306 ) ) ;
#30653 = ADVANCED_FACE ( 'NONE', ( #15781 ), #21136, .T. ) ;
#30654 = AXIS2_PLACEMENT_3D ( 'NONE', #29410, #21183, #9060 ) ;
#30655 = CARTESIAN_POINT ( 'NONE',  ( 8.999999999770000869, 20.99999999999999645, -51.10000000000000142 ) ) ;
#30656 = LINE ( 'NONE', #25778, #10798 ) ;
#30657 = DIRECTION ( 'NONE',  ( 1.000000000000000000, -3.981005269678786617E-12, 1.941197879946729322E-12 ) ) ;
#30658 = CARTESIAN_POINT ( 'NONE',  ( -9.993285220779425160, -25.61999708228226069, 27.99999999999999645 ) ) ;
#30659 = SHAPE_REPRESENTATION ( 'Drive Pawl', ( #17722 ), #14795 ) ;
#30660 = CARTESIAN_POINT ( 'NONE',  ( -23.51354662350000169, -14.83147814589999847, 224.7915671760000009 ) ) ;
#30661 = ORIENTED_EDGE ( 'NONE', *, *, #1903, .F. ) ;
#30662 = CARTESIAN_POINT ( 'NONE',  ( -5.939015604524707115, -0.1501891088408410790, -53.55673954922500002 ) ) ;
#30663 = ORIENTED_EDGE ( 'NONE', *, *, #9957, .F. ) ;
#30664 = ORIENTED_EDGE ( 'NONE', *, *, #25827, .F. ) ;
#30665 = CARTESIAN_POINT ( 'NONE',  ( -8.699999999730072986, -28.07050130677435362, -25.59757157925566773 ) ) ;
#30666 = EDGE_LOOP ( 'NONE', ( #16112, #14350, #23617, #5218, #25274, #8372 ) ) ;
#30667 = DIRECTION ( 'NONE',  ( -2.764840495839172918E-12, -0.9128796883888953273, 0.4082287037029531107 ) ) ;
#30668 = DIRECTION ( 'NONE',  ( 0.7071067811865475727, -0.7071067811865475727, 0.000000000000000000 ) ) ;
#30669 = FACE_OUTER_BOUND ( 'NONE', #11061, .T. ) ;
#30670 = AXIS2_PLACEMENT_3D ( 'NONE', #13856, #6767, #16363 ) ;
#30671 = CARTESIAN_POINT ( 'NONE',  ( 1.645560275461343203, -28.45273235261698019, 4.999998581000003384 ) ) ;
#30672 = CARTESIAN_POINT ( 'NONE',  ( -26.93696268452645981, -0.4901285798020276196, 0.000000000000000000 ) ) ;
#30673 = CARTESIAN_POINT ( 'NONE',  ( 27.92857142860000152, 3.552713678799999608E-15, 92.06031501460000754 ) ) ;
#30674 = CARTESIAN_POINT ( 'NONE',  ( -3.357947603668644199, 3.429589946161242242, -3.631232180600004966 ) ) ;
#30675 = CARTESIAN_POINT ( 'NONE',  ( -27.04041630550000264, -9.934689828449998927, 230.6999999999999886 ) ) ;
#30676 = ORIENTED_EDGE ( 'NONE', *, *, #8704, .F. ) ;
#30677 = CARTESIAN_POINT ( 'NONE',  ( 25.33388806075444322, -13.05639290569185285, 5.735287129097097925 ) ) ;
#30678 = CARTESIAN_POINT ( 'NONE',  ( 2.326244606069572285, 3.379075471592549729, -17.71259163650000446 ) ) ;
#30679 = CARTESIAN_POINT ( 'NONE',  ( 4.373195337096333013, -2.904765488536246387, -35.95875473020000612 ) ) ;
#30680 = CARTESIAN_POINT ( 'NONE',  ( 27.03594125075309762, 0.4919295335571094996, -0.6999999999999784173 ) ) ;
#30681 = CARTESIAN_POINT ( 'NONE',  ( -24.07583586439999834, -13.90018868249999962, 223.9000014189999774 ) ) ;
#30682 = CARTESIAN_POINT ( 'NONE',  ( -7.999999999628196967, -15.17858304667434233, -40.45432020020274422 ) ) ;
#30683 = CARTESIAN_POINT ( 'NONE',  ( -20.30403093138962234, 20.00000000003553424, 1.000000000000000888 ) ) ;
#30684 = DIRECTION ( 'NONE',  ( 0.9002473904559572526, -0.4353787270609801308, 0.000000000000000000 ) ) ;
#30685 = CARTESIAN_POINT ( 'NONE',  ( 8.700000000284820345, -13.66682223737197610, -36.55330428411850363 ) ) ;
#30686 = CARTESIAN_POINT ( 'NONE',  ( 0.2655682516278248806, -27.79918151443105856, 3.920205022000022854 ) ) ;
#30687 = ADVANCED_FACE ( 'NONE', ( #1941 ), #1478, .T. ) ;
#30688 = CYLINDRICAL_SURFACE ( 'NONE', #15265, 0.9999999999999988898 ) ;
#30689 = EDGE_LOOP ( 'NONE', ( #6611, #12727, #28290, #20083, #13757, #20633, #7773, #23734 ) ) ;
#30690 = CARTESIAN_POINT ( 'NONE',  ( 22.97559295455008765, 15.65128684778802715, 8.000000000000007105 ) ) ;
#30691 = FILL_AREA_STYLE_COLOUR ( '', #26310 ) ;
#30692 = CARTESIAN_POINT ( 'NONE',  ( -0.4642112451548723873, -5.194573592496900538, -0.7000356040109552147 ) ) ;
#30693 = ORIENTED_EDGE ( 'NONE', *, *, #20838, .T. ) ;
#30694 = CARTESIAN_POINT ( 'NONE',  ( -5.162912894389027230, 3.035924517800103750, -45.32354844312499864 ) ) ;
#30695 = ORIENTED_EDGE ( 'NONE', *, *, #14909, .F. ) ;
#30696 = ORIENTED_EDGE ( 'NONE', *, *, #11306, .F. ) ;
#30697 = CIRCLE ( 'NONE', #28693, 1.656072167390155281 ) ;
#30698 = ORIENTED_EDGE ( 'NONE', *, *, #4464, .T. ) ;
#30699 = CARTESIAN_POINT ( 'NONE',  ( -1.089818731940000118, -28.47945802909999813, 224.6898005070000011 ) ) ;
#30700 = VERTEX_POINT ( 'NONE', #25230 ) ;
#30701 = CARTESIAN_POINT ( 'NONE',  ( -27.79999999999999716, -2.360778239559999931E-11, 229.0000000000000000 ) ) ;
#30702 = SURFACE_STYLE_USAGE ( .BOTH. , #11350 ) ;
#30703 = CARTESIAN_POINT ( 'NONE',  ( 11.69999999989999928, 19.99999999999999645, -1.049999999600002898 ) ) ;
#30704 = DIRECTION ( 'NONE',  ( 1.000000000000000000, 0.000000000000000000, 0.000000000000000000 ) ) ;
#30705 = B_SPLINE_CURVE_WITH_KNOTS ( 'NONE', 3,
 ( #9166, #8858, #23195, #23041, #6504, #18768 ),
 .UNSPECIFIED., .F., .F.,
 ( 4, 2, 4 ),
 ( 0.000000000000000000, 0.5000000000000000000, 1.000000000000000000 ),
 .UNSPECIFIED. ) ;
#30706 = CARTESIAN_POINT ( 'NONE',  ( -1.691925696239311883, -4.899391353707211572, -93.28167488203875735 ) ) ;
#30707 = CARTESIAN_POINT ( 'NONE',  ( 14.73807200698136910, -22.00000000000000711, -26.99929886424486014 ) ) ;
#30708 = CARTESIAN_POINT ( 'NONE',  ( 3.430769921896569929, -1.057732186200032176, 227.6978496355009725 ) ) ;
#30709 = FACE_OUTER_BOUND ( 'NONE', #12360, .T. ) ;
#30710 = ORIENTED_EDGE ( 'NONE', *, *, #10606, .T. ) ;
#30711 = ADVANCED_FACE ( 'NONE', ( #1316 ), #12283, .F. ) ;
#30712 = CARTESIAN_POINT ( 'NONE',  ( 2.521631941452523229, 3.946033397249450125, -5.200967428500000267 ) ) ;
#30713 = CARTESIAN_POINT ( 'NONE',  ( -4.637531673247329955, -1.216599033067103264, -24.10906121680000069 ) ) ;
#30714 = CARTESIAN_POINT ( 'NONE',  ( 27.14999999970000033, -1.044534738649999915E-13, 0.000000000000000000 ) ) ;
#30715 = CARTESIAN_POINT ( 'NONE',  ( -23.73988791507445484, -12.43614577693665879, 224.8540320935318846 ) ) ;
#30716 = LINE ( 'NONE', #3970, #21344 ) ;
#30717 = CARTESIAN_POINT ( 'NONE',  ( 4.638687372303289536, 6.462009008183451364, -40.63090155201975762 ) ) ;
#30718 = CARTESIAN_POINT ( 'NONE',  ( -10.14902473054660348, -26.01926976365539090, 187.9396849849999853 ) ) ;
#30719 = STYLED_ITEM ( 'NONE', ( #350 ), #20809 ) ;
#30721 = CARTESIAN_POINT ( 'NONE',  ( 23.91557559422898649, -14.17419444102282000, 5.732984736081180976 ) ) ;
#30720 = B_SPLINE_CURVE_WITH_KNOTS ( 'NONE', 3,
 ( #25104, #1189, #20077, #8250, #24947, #22742, #25429, #25262, #3694, #3379 ),
 .UNSPECIFIED., .F., .F.,
 ( 4, 2, 2, 2, 4 ),
 ( 0.000000000000000000, 0.2500000000000000000, 0.5000000000000000000, 0.7500000000000000000, 1.000000000000000000 ),
 .UNSPECIFIED. ) ;
#30722 = DIRECTION ( 'NONE',  ( -1.000000000000000000, 0.000000000000000000, 0.000000000000000000 ) ) ;
#30723 = CARTESIAN_POINT ( 'NONE',  ( -4.175165894169885483, -119.7166638525666826, -43.39999999999999858 ) ) ;
#30724 = ORIENTED_EDGE ( 'NONE', *, *, #27575, .F. ) ;
#30725 = CARTESIAN_POINT ( 'NONE',  ( -0.8884012486115674401, 4.851036559086118416, -59.50324387862499265 ) ) ;
#30726 = CARTESIAN_POINT ( 'NONE',  ( -0.2762902765781530823, -2.099999999790001404, 226.6412452697800859 ) ) ;
#30727 = CARTESIAN_POINT ( 'NONE',  ( -8.903108651239966420, -22.82508830966961000, 190.0000000000000000 ) ) ;
#30728 = CARTESIAN_POINT ( 'NONE',  ( -1.484924240490000047, -1.484924240490000047, 226.6412452697800006 ) ) ;
#30729 = ORIENTED_EDGE ( 'NONE', *, *, #6321, .F. ) ;
#30730 = CARTESIAN_POINT ( 'NONE',  ( -19.80535357377644701, 19.50875577052588739, 3.000000106999994642 ) ) ;
#30731 = DIRECTION ( 'NONE',  ( 1.000000000000000000, -1.843431230200084908E-12, 2.650498504963248473E-12 ) ) ;
#30732 = ORIENTED_EDGE ( 'NONE', *, *, #29808, .F. ) ;
#30733 = VERTEX_POINT ( 'NONE', #20666 ) ;
#30734 = ORIENTED_EDGE ( 'NONE', *, *, #27545, .F. ) ;
#30735 = ORIENTED_EDGE ( 'NONE', *, *, #13556, .T. ) ;
#30736 = CARTESIAN_POINT ( 'NONE',  ( -12.30000000011639827, -27.83759322994970375, -31.51671256534945087 ) ) ;
#30737 = CARTESIAN_POINT ( 'NONE',  ( 26.79556473285982321, 0.4875557887249851730, -0.6999999999999784173 ) ) ;
#30738 = CARTESIAN_POINT ( 'NONE',  ( -5.167095691178253070, 1.703695954683749125, -67.94019511502500563 ) ) ;
#30739 = EDGE_CURVE ( 'NONE', #11537, #19543, #21286, .T. ) ;
#30740 = CARTESIAN_POINT ( 'NONE',  ( 27.53132593009999951, 1.219291334560000045E-11, 229.7313259299999686 ) ) ;
#30741 = AXIS2_PLACEMENT_3D ( 'NONE', #2613, #30794, #12060 ) ;
#30742 = CARTESIAN_POINT ( 'NONE',  ( -0.2892544267695482674, -26.79878419693495317, 223.9285094851671261 ) ) ;
#30743 = CARTESIAN_POINT ( 'NONE',  ( -23.11028700030000138, -15.72531859329999726, 222.0000000000000000 ) ) ;
#30744 = CARTESIAN_POINT ( 'NONE',  ( 1.644581066898457955, -4.845992769441807013, -0.7000398998402457273 ) ) ;
#30745 = ORIENTED_EDGE ( 'NONE', *, *, #7073, .T. ) ;
#30746 = ADVANCED_FACE ( 'NONE', ( #16703 ), #14370, .F. ) ;
#30747 = CARTESIAN_POINT ( 'NONE',  ( -18.65448805331473991, 19.99991030667355218, -0.6087647090073780021 ) ) ;
#30748 = PRODUCT_DEFINITION_CONTEXT ( 'detailed design', #1352, 'design' ) ;
#30749 = CARTESIAN_POINT ( 'NONE',  ( 0.7763070146520680836, 4.277613328189620923, -14.02400681850000197 ) ) ;
#30750 = CARTESIAN_POINT ( 'NONE',  ( 27.23548387100000312, -3.552713678799999608E-15, 38.33953982530000104 ) ) ;
#30751 = CARTESIAN_POINT ( 'NONE',  ( -10.69999999968908355, -24.20408354487524605, -30.01220480028783655 ) ) ;
#30752 = EDGE_LOOP ( 'NONE', ( #11615, #6697, #23027, #26109 ) ) ;
#30753 = CARTESIAN_POINT ( 'NONE',  ( 26.71519619425450642, -2.391783224228639870, -1.399999999999998579 ) ) ;
#30754 = CARTESIAN_POINT ( 'NONE',  ( 1.605176535610508326, -27.75389821387976852, 4.895940783000013674 ) ) ;
#30755 = CARTESIAN_POINT ( 'NONE',  ( 26.05511440549999946, -14.93230011260000012, 222.0000000000000000 ) ) ;
#30756 = CARTESIAN_POINT ( 'NONE',  ( 9.594426947539483663, -25.77213547066686772, 25.40809952595784793 ) ) ;
#30757 = ORIENTED_EDGE ( 'NONE', *, *, #5098, .F. ) ;
#30758 = CARTESIAN_POINT ( 'NONE',  ( 22.69912944684746137, -14.24746549195691436, 4.513393846468806814 ) ) ;
#30759 = FACE_OUTER_BOUND ( 'NONE', #22609, .T. ) ;
#30760 = DIRECTION ( 'NONE',  ( 1.000000000000000000, 0.000000000000000000, 0.000000000000000000 ) ) ;
#30761 = VERTEX_POINT ( 'NONE', #7276 ) ;
#30762 = EDGE_CURVE ( 'NONE', #24086, #10417, #11843, .T. ) ;
#30763 = CARTESIAN_POINT ( 'NONE',  ( 26.95545383900000047, 8.667969224290001051, 229.0000000000000000 ) ) ;
#30764 = PLANE ( 'NONE',  #23677 ) ;
#30765 = AXIS2_PLACEMENT_3D ( 'NONE', #19764, #22436, #10011 ) ;
#30766 = CARTESIAN_POINT ( 'NONE',  ( 2.707138150663993326, -3.848833623503777446, -68.10000000002500542 ) ) ;
#30767 = PRODUCT_DEFINITION_SHAPE ( 'NONE', 'NONE',  #24622 ) ;
#30768 = DIRECTION ( 'NONE',  ( 1.000000000000000000, -1.843431230200084908E-12, 2.650498504963248473E-12 ) ) ;
#30769 = CARTESIAN_POINT ( 'NONE',  ( -4.734981018114883256, 0.5816554918100906857, -44.10000000002498410 ) ) ;
#30770 = SURFACE_SIDE_STYLE ('',( #11576 ) ) ;
#30771 = EDGE_LOOP ( 'NONE', ( #12565, #15125, #28520, #10100, #18639, #25612 ) ) ;
#30772 = LINE ( 'NONE', #21331, #26026 ) ;
#30773 = CARTESIAN_POINT ( 'NONE',  ( 3.225090657556859419, -3.689912930009636938, -65.24605006312501132 ) ) ;
#30774 = EDGE_LOOP ( 'NONE', ( #23369, #27796, #11770, #16097, #21475, #4998, #13221 ) ) ;
#30775 = CYLINDRICAL_SURFACE ( 'NONE', #13935, 2.926829268290000119 ) ;
#30776 = B_SPLINE_CURVE_WITH_KNOTS ( 'NONE', 3,
 ( #14080, #2281, #4793, #16726, #7301, #7143, #9033, #4478, #30913, #6830, #18942, #6672 ),
 .UNSPECIFIED., .F., .F.,
 ( 4, 2, 2, 2, 2, 4 ),
 ( 0.000000000000000000, 0.2500000000000006661, 0.5000000000000013323, 0.6250000000000016653, 0.7500000000000019984, 1.000000000000000000 ),
 .UNSPECIFIED. ) ;
#30777 = B_SPLINE_CURVE_WITH_KNOTS ( 'NONE', 3,
 ( #18567, #1117, #3789, #13379, #1433, #15900, #25034, #29907, #11028, #20617, #8647, #25506 ),
 .UNSPECIFIED., .F., .F.,
 ( 4, 2, 2, 2, 2, 4 ),
 ( 0.000000000000000000, 0.2500000000000128786, 0.3750000000000193179, 0.5000000000000257572, 0.7500000000000128786, 1.000000000000000000 ),
 .UNSPECIFIED. ) ;
#30778 = CARTESIAN_POINT ( 'NONE',  ( -2.098672137722010334, -3.287437779826620776, -44.10000000002499121 ) ) ;
#30779 = ORIENTED_EDGE ( 'NONE', *, *, #9801, .T. ) ;
#30780 = CARTESIAN_POINT ( 'NONE',  ( 20.30405755279999980, 20.00000000000000000, 229.0000000000000000 ) ) ;
#30781 = CARTESIAN_POINT ( 'NONE',  ( -23.83861932771936765, -15.61961844720760340, 4.689445057000002137 ) ) ;
#30782 = CARTESIAN_POINT ( 'NONE',  ( 9.963156062430000404, 19.99999999999999645, -42.69473902060000370 ) ) ;
#30783 = ADVANCED_FACE ( 'NONE', ( #16557 ), #17070, .F. ) ;
#30784 = B_SPLINE_SURFACE_WITH_KNOTS ( 'NONE', 5, 1, ( 
 ( #5888, #1032 ),
 ( #15495, #10935 ),
 ( #6049, #10621 ),
 ( #20216, #25099 ),
 ( #3532, #22736 ),
 ( #13127, #15646 ),
 ( #25257, #30755 ),
 ( #23213, #16272 ),
 ( #25731, #30454 ) ),
 .UNSPECIFIED., .F., .F., .F.,
 ( 6, 3, 6 ),
 ( 2, 2 ),
 ( 0.000000000000000000, 55.31395627319999875, 94.75474476520000167 ),
 ( -3.500000000000000000, 3.500000000000000000 ),
 .UNSPECIFIED. ) ;
#30785 = UNCERTAINTY_MEASURE_WITH_UNIT (LENGTH_MEASURE( 1.000000000000000082E-05 ), #28244, 'distance_accuracy_value', 'NONE');
#30786 = CARTESIAN_POINT ( 'NONE',  ( -17.40775135787469807, -23.43820796653147553, -32.11710110277844876 ) ) ;
#30787 = CARTESIAN_POINT ( 'NONE',  ( 6.000000000000000000, -29.96004123392021157, -79.78289277550334191 ) ) ;
#30788 = CARTESIAN_POINT ( 'NONE',  ( 8.700000000244243026, -28.90935745820462088, -30.74712106076765394 ) ) ;
#30789 = VERTEX_POINT ( 'NONE', #2405 ) ;
#30790 = LINE ( 'NONE', #14422, #13475 ) ;
#30791 = CARTESIAN_POINT ( 'NONE',  ( 24.66410523950000311, -14.28055064019999953, 226.1000014189999945 ) ) ;
#30792 = DIRECTION ( 'NONE',  ( 0.000000000000000000, 1.000000000000000000, 0.000000000000000000 ) ) ;
#30793 = DIRECTION ( 'NONE',  ( 1.000000000000000000, 0.000000000000000000, 0.000000000000000000 ) ) ;
#30794 = DIRECTION ( 'NONE',  ( 1.000000000000000000, 5.998481157687279274E-24, -2.257150022441830001E-12 ) ) ;
#30795 = CARTESIAN_POINT ( 'NONE',  ( 9.502613819369999604, -7.533418146770000767, 230.6412452697800006 ) ) ;
#30796 = ADVANCED_FACE ( 'NONE', ( #5066 ), #26471, .T. ) ;
#30797 = FACE_OUTER_BOUND ( 'NONE', #17410, .T. ) ;
#30798 = CARTESIAN_POINT ( 'NONE',  ( 23.56856306074712037, -14.74329105725733946, 225.4958374175672304 ) ) ;
#30799 = CARTESIAN_POINT ( 'NONE',  ( 5.053719932302922935, 0.5711438793038403627, -54.26771407622499765 ) ) ;
#30800 = EDGE_CURVE ( 'NONE', #30026, #18612, #30986, .T. ) ;
#30801 = EDGE_CURVE ( 'NONE', #29409, #23194, #17791, .T. ) ;
#30802 = DIRECTION ( 'NONE',  ( 0.000000000000000000, -2.257145581549999994E-12, -1.000000000000000000 ) ) ;
#30803 = CARTESIAN_POINT ( 'NONE',  ( -7.534632680830988249, -6.582071621271182060, -34.26887834115397169 ) ) ;
#30804 = CARTESIAN_POINT ( 'NONE',  ( -17.59696597919420213, 10.20816091468181774, 0.000000000000000000 ) ) ;
#30805 = CONICAL_SURFACE ( 'NONE', #17221, 2.500000000105226938, 0.7853981633974418397 ) ;
#30806 = DIRECTION ( 'NONE',  ( 0.000000000000000000, -0.9396926207858125046, -0.3420201433259318358 ) ) ;
#30807 = EDGE_CURVE ( 'NONE', #9747, #20099, #10687, .T. ) ;
#30808 = CARTESIAN_POINT ( 'NONE',  ( 10.69999999997516760, -26.60546859447386581, -31.39999999999999147 ) ) ;
#30809 = CARTESIAN_POINT ( 'NONE',  ( -5.473210459068893918, -0.1384095709066185120, -54.35673954922499718 ) ) ;
#30810 = VERTEX_POINT ( 'NONE', #52 ) ;
#30811 = VERTEX_POINT ( 'NONE', #19232 ) ;
#30813 = EDGE_CURVE ( 'NONE', #170, #14439, #29082, .T. ) ;
#30812 = LINE ( 'NONE', #15590, #26230 ) ;
#30814 = ORIENTED_EDGE ( 'NONE', *, *, #15559, .T. ) ;
#30815 = CARTESIAN_POINT ( 'NONE',  ( 14.72975346148849241, -28.24357319906857455, -23.34478253265713832 ) ) ;
#30816 = CARTESIAN_POINT ( 'NONE',  ( -8.000000000054376059, -115.1185614904100447, 21.95989595794526039 ) ) ;
#30817 = CARTESIAN_POINT ( 'NONE',  ( -27.07233446881437899, 8.380004974182886812, 6.600000000000022737 ) ) ;
#30818 = ADVANCED_FACE ( 'NONE', ( #14057 ), #23661, .F. ) ;
#30819 = VECTOR ( 'NONE', #22528, 1000.000000000000000 ) ;
#30820 = CARTESIAN_POINT ( 'NONE',  ( -21.02335142420000125, 19.26967309480000168, 226.0000000000000000 ) ) ;
#30821 = CARTESIAN_POINT ( 'NONE',  ( 27.98121187870611593, -9.706323496128696604, 1.000000000000000888 ) ) ;
#30822 = CARTESIAN_POINT ( 'NONE',  ( -16.85343921394901301, 12.09981795542885585, -1.000005633855494125E-09 ) ) ;
#30823 = CARTESIAN_POINT ( 'NONE',  ( -6.277996069133942925, 1.777976852108807737, -6.710827254899999872 ) ) ;
#30824 = AXIS2_PLACEMENT_3D ( 'NONE', #17770, #27846, #20149 ) ;
#30825 = CARTESIAN_POINT ( 'NONE',  ( -23.69119896560000171, -20.94188573509999785, 229.2404163060000144 ) ) ;
#30826 = ORIENTED_EDGE ( 'NONE', *, *, #8126, .T. ) ;
#30827 = CARTESIAN_POINT ( 'NONE',  ( -24.15901410609999900, -15.12012600329999934, 224.4928788709999878 ) ) ;
#30828 = EDGE_CURVE ( 'NONE', #8540, #11113, #10775, .T. ) ;
#30829 = CARTESIAN_POINT ( 'NONE',  ( 2.946576500976501478, 4.280162264036399655, -18.21259163650000090 ) ) ;
#30830 = CARTESIAN_POINT ( 'NONE',  ( 24.92257222434601616, 14.03654374138045213, 8.000000000000007105 ) ) ;
#30831 = CARTESIAN_POINT ( 'NONE',  ( 0.9711900386741275648, -16.47311334361725343, -109.1271631200178689 ) ) ;
#30832 = CARTESIAN_POINT ( 'NONE',  ( 28.68577476828162531, -9.950727360111285336, 0.7595836940000044724 ) ) ;
#30833 = CARTESIAN_POINT ( 'NONE',  ( -19.56375666326936269, 19.56885676738829005, 0.5004811919999962999 ) ) ;
#30834 = CARTESIAN_POINT ( 'NONE',  ( -3.313783883474008984, -27.85733552065744334, 8.000000000000007105 ) ) ;
#30835 = CARTESIAN_POINT ( 'NONE',  ( -1.557622931652909104, -4.259165208650869339, -43.98640794712500224 ) ) ;
#30836 = CARTESIAN_POINT ( 'NONE',  ( 26.95478617150206802, 4.952129227130185107, -0.6999999999999784173 ) ) ;
#30837 = CARTESIAN_POINT ( 'NONE',  ( -2.556415643314931874, -2.434303047057058134, 226.6412452697750837 ) ) ;
#30838 = DIRECTION ( 'NONE',  ( -2.249415931299125355E-12, 0.9431856258987900699, 0.3322662713817151059 ) ) ;
#30839 = VECTOR ( 'NONE', #28131, 1000.000000000000000 ) ;
#30840 = CONICAL_SURFACE ( 'NONE', #3200, 1.120011618224791450, 0.0001253086068439055573 ) ;
#30841 = CARTESIAN_POINT ( 'NONE',  ( -13.12132034329999897, 21.69999999990000106, -69.22132034359999864 ) ) ;
#30842 = EDGE_LOOP ( 'NONE', ( #5606, #16019, #14201, #27242 ) ) ;
#30843 = AXIS2_PLACEMENT_3D ( 'NONE', #22880, #15626, #20983 ) ;
#30844 = CARTESIAN_POINT ( 'NONE',  ( 8.700000000281329804, -5.981227587278358016, -27.94042817480098506 ) ) ;
#30845 = CARTESIAN_POINT ( 'NONE',  ( -9.000000000229999131, 21.70000000000000284, -48.10000000000000142 ) ) ;
#30846 = B_SPLINE_CURVE_WITH_KNOTS ( 'NONE', 5,
 ( #6161, #21546, #13401, #16809, #14466, #1461 ),
 .UNSPECIFIED., .F., .F.,
 ( 6, 6 ),
 ( 64.89339659389999326, 88.69760957229999576 ),
 .UNSPECIFIED. ) ;
#30847 = CARTESIAN_POINT ( 'NONE',  ( -0.8587415393533248675, -5.153862915431827396, -0.7000227180819994510 ) ) ;
#30848 = EDGE_LOOP ( 'NONE', ( #9613, #28925, #17706, #18470 ) ) ;
#30849 = CARTESIAN_POINT ( 'NONE',  ( 0.5921542527409766610, -4.847825725916151463, -44.53057807742500529 ) ) ;
#30850 = ORIENTED_EDGE ( 'NONE', *, *, #15014, .F. ) ;
#30851 = EDGE_LOOP ( 'NONE', ( #1087, #4568, #10487, #28829, #14398, #29325 ) ) ;
#30852 = ORIENTED_EDGE ( 'NONE', *, *, #27366, .F. ) ;
#30853 = CARTESIAN_POINT ( 'NONE',  ( -0.6685465369699999938, -28.49273882800000024, 224.0990923460000204 ) ) ;
#30854 = ADVANCED_FACE ( 'NONE', ( #3159 ), #12760, .F. ) ;
#30855 = VERTEX_POINT ( 'NONE', #7875 ) ;
#30856 = FACE_OUTER_BOUND ( 'NONE', #18287, .T. ) ;
#30857 = CARTESIAN_POINT ( 'NONE',  ( 23.35655559247464907, 15.07705663187610945, 4.319305385000027364 ) ) ;
#30858 = CARTESIAN_POINT ( 'NONE',  ( -353541.5905939771328, -322767.6580554517568, 144295.1095977958466 ) ) ;
#30859 = CARTESIAN_POINT ( 'NONE',  ( -10.82908725742657730, -27.76276047461854901, 36.78285841159999592 ) ) ;
#30860 = EDGE_CURVE ( 'NONE', #20463, #5036, #19320, .T. ) ;
#30861 = EDGE_CURVE ( 'NONE', #21756, #28017, #3952, .T. ) ;
#30862 = CARTESIAN_POINT ( 'NONE',  ( 19.39238560432175973, 20.00003183196481871, -0.3307242700730367857 ) ) ;
#30863 = EDGE_CURVE ( 'NONE', #26866, #4259, #25035, .T. ) ;
#30864 = DIRECTION ( 'NONE',  ( -1.000000000000000000, 6.565028073413479156E-24, -2.257144471327815248E-12 ) ) ;
#30865 = DIRECTION ( 'NONE',  ( 1.000000000000000000, 0.000000000000000000, 0.000000000000000000 ) ) ;
#30866 = CIRCLE ( 'NONE', #2230, 3.200000000000000178 ) ;
#30867 = CARTESIAN_POINT ( 'NONE',  ( -8.999999999710000864, 20.70710678120000381, -44.39289321881399530 ) ) ;
#30868 = EDGE_LOOP ( 'NONE', ( #10215, #21710, #21134, #22294 ) ) ;
#30869 = AXIS2_PLACEMENT_3D ( 'NONE', #24836, #5937, #10664 ) ;
#30870 = CARTESIAN_POINT ( 'NONE',  ( 3.530284718056032833, 5.524446756132658898, -5.200967428500000267 ) ) ;
#30871 = CARTESIAN_POINT ( 'NONE',  ( -6.202057249109299342, 1.908294659314309305, -21.72289663400001203 ) ) ;
#30872 = AXIS2_PLACEMENT_3D ( 'NONE', #5926, #20564, #13012 ) ;
#30873 = CARTESIAN_POINT ( 'NONE',  ( -1.790201522669007561, -3.063245535112757434, 0.000000000000000000 ) ) ;
#30874 = CARTESIAN_POINT ( 'NONE',  ( -3.005466662781860698, -2.712465827810011110, -92.40868836340081316 ) ) ;
#30875 = CARTESIAN_POINT ( 'NONE',  ( 0.000000000000000000, 0.000000000000000000, 43.60555127639999995 ) ) ;
#30876 = DIRECTION ( 'NONE',  ( -0.000000000000000000, -0.000000000000000000, -1.000000000000000000 ) ) ;
#30877 = CARTESIAN_POINT ( 'NONE',  ( -24.55841378230000061, -14.46270012129999927, 226.0798679369999888 ) ) ;
#30878 = CARTESIAN_POINT ( 'NONE',  ( -353541.5905929750297, -345962.9896101437625, -72978.28499981865752 ) ) ;
#30879 = CARTESIAN_POINT ( 'NONE',  ( 1.645560275461343203, -28.45273235261698019, 4.999998581000003384 ) ) ;
#30880 = CARTESIAN_POINT ( 'NONE',  ( -16.39980503796714828, -21.22523991776962404, -1.399999999999998579 ) ) ;
#30881 = VERTEX_POINT ( 'NONE', #27087 ) ;
#30882 = STYLED_ITEM ( 'NONE', ( #24302 ), #12524 ) ;
#30883 = CARTESIAN_POINT ( 'NONE',  ( -21.32009893540000078, 17.08474177209999922, 230.0000000000000000 ) ) ;
#30884 = ORIENTED_EDGE ( 'NONE', *, *, #2441, .F. ) ;
#30885 = CARTESIAN_POINT ( 'NONE',  ( -2.595987296770100095, -16.63200279373747392, -109.8342699011499946 ) ) ;
#30886 = CARTESIAN_POINT ( 'NONE',  ( 3.430850994441077439, -5.010772104901466406, -27.13292313650000764 ) ) ;
#30887 = ORIENTED_EDGE ( 'NONE', *, *, #21740, .T. ) ;
#30888 = CARTESIAN_POINT ( 'NONE',  ( -3.552713678799999608E-15, 0.000000000000000000, 143.2171415880000040 ) ) ;
#30889 = DIRECTION ( 'NONE',  ( -0.3090169943750401549, -0.9510565162951233331, 0.000000000000000000 ) ) ;
#30890 = CIRCLE ( 'NONE', #9260, 27.92857142860000152 ) ;
#30891 = EDGE_LOOP ( 'NONE', ( #21754, #18760, #16412, #5219 ) ) ;
#30892 = ORIENTED_EDGE ( 'NONE', *, *, #9046, .T. ) ;
#30893 = ORIENTED_EDGE ( 'NONE', *, *, #3749, .T. ) ;
#30894 = AXIS2_PLACEMENT_3D ( 'NONE', #15309, #5701, #24911 ) ;
#30895 = SURFACE_STYLE_USAGE ( .BOTH. , #2261 ) ;
#30896 = CIRCLE ( 'NONE', #4689, 27.50000000000000000 ) ;
#30897 = ORIENTED_EDGE ( 'NONE', *, *, #9235, .T. ) ;
#30898 = CARTESIAN_POINT ( 'NONE',  ( -12.30000000028043416, -29.55893389567417273, -30.36654950393055685 ) ) ;
#30899 = DIRECTION ( 'NONE',  ( 0.000000000000000000, 0.000000000000000000, -1.000000000000000000 ) ) ;
#30900 = CARTESIAN_POINT ( 'NONE',  ( 2.708949881112989289, 3.684664522020659305, -66.24226422532500180 ) ) ;
#30901 = CARTESIAN_POINT ( 'NONE',  ( 27.24857305730000334, 4.341416115490000300E-12, 229.9172022069999741 ) ) ;
#30902 =( REPRESENTATION_RELATIONSHIP ('NONE','NONE', #2712, #527 ) REPRESENTATION_RELATIONSHIP_WITH_TRANSFORMATION ( #9872 )SHAPE_REPRESENTATION_RELATIONSHIP( ) );
#30903 = DIRECTION ( 'NONE',  ( 0.000000000000000000, 0.000000000000000000, 1.000000000000000000 ) ) ;
#30904 = CARTESIAN_POINT ( 'NONE',  ( 28.01995124469999965, -5.907569749770000378, 222.0000000000000000 ) ) ;
#30905 = VECTOR ( 'NONE', #27631, 1000.000000000000000 ) ;
#30906 = CARTESIAN_POINT ( 'NONE',  ( 3.823514640232639206, -2.731196763342798484, -0.7000558027893447610 ) ) ;
#30907 = VERTEX_POINT ( 'NONE', #17174 ) ;
#30908 = CARTESIAN_POINT ( 'NONE',  ( -20.22090452287337925, 20.00040987029326800, 0.5517657372802144966 ) ) ;
#30909 = CARTESIAN_POINT ( 'NONE',  ( 3.316815470610420924, 4.395877990916175371, -13.22796858840000134 ) ) ;
#30910 = CARTESIAN_POINT ( 'NONE',  ( 2.131628207279999844E-14, -1.704192342799999938E-14, 231.6999999999999886 ) ) ;
#30911 = CARTESIAN_POINT ( 'NONE',  ( 11.49589634081054434, 4.456723487524678617, 232.6627635931969280 ) ) ;
#30912 = ORIENTED_EDGE ( 'NONE', *, *, #23117, .F. ) ;
#30913 = CARTESIAN_POINT ( 'NONE',  ( -23.29644702443709292, -15.16961937508697922, 4.504162582432789996 ) ) ;
#30914 = PLANE ( 'NONE',  #16285 ) ;
#30915 = CIRCLE ( 'NONE', #26399, 27.23548387080000310 ) ;
#30916 = CARTESIAN_POINT ( 'NONE',  ( -23.61125025500000163, 15.96150951279999930, 222.0000000000000000 ) ) ;
#30917 = DIRECTION ( 'NONE',  ( 0.000000000000000000, 1.000000000000000000, 0.000000000000000000 ) ) ;
#30918 = CARTESIAN_POINT ( 'NONE',  ( 5.762915210551160072, -2.052471225477275674, -67.23341453912500754 ) ) ;
#30919 = CARTESIAN_POINT ( 'NONE',  ( 12.55799324160000019, 20.99999999999999645, -55.95247857500000066 ) ) ;
#30920 = DIRECTION ( 'NONE',  ( 0.000000000000000000, -0.3420201433259318913, 0.9396926207858126157 ) ) ;
#30921 = ORIENTED_EDGE ( 'NONE', *, *, #15083, .T. ) ;
#30922 = ADVANCED_FACE ( 'NONE', ( #364 ), #3012, .T. ) ;
#30923 = CARTESIAN_POINT ( 'NONE',  ( -12.37231291232859043, -23.57340789884118593, -24.60484118030849032 ) ) ;
#30924 = CARTESIAN_POINT ( 'NONE',  ( 16.10061776502996622, -9.307365792519414427, -0.6999999999999784173 ) ) ;
#30925 = B_SPLINE_CURVE_WITH_KNOTS ( 'NONE', 3,
 ( #13639, #23244, #30788, #23872, #9213, #6552 ),
 .UNSPECIFIED., .F., .F.,
 ( 4, 2, 4 ),
 ( 0.000000000000000000, 0.5000000000000000000, 1.000000000000000000 ),
 .UNSPECIFIED. ) ;
#30926 = FACE_BOUND ( 'NONE', #10408, .T. ) ;
#30927 = CARTESIAN_POINT ( 'NONE',  ( -4.792751602502305808, 0.3708384435674089152, -68.10000000002500542 ) ) ;
#30928 = VECTOR ( 'NONE', #23486, 1000.000000000000000 ) ;
#30929 = AXIS2_PLACEMENT_3D ( 'NONE', #23626, #21718, #2060 ) ;
#30930 = EDGE_CURVE ( 'NONE', #17294, #13677, #15734, .T. ) ;
#30931 = LINE ( 'NONE', #26205, #5451 ) ;
#30932 = ORIENTED_EDGE ( 'NONE', *, *, #20661, .F. ) ;
#30933 = CARTESIAN_POINT ( 'NONE',  ( -17.49199711315135986, -29.39779533043000015, -32.78913491261000246 ) ) ;
#30934 = CARTESIAN_POINT ( 'NONE',  ( 0.2444022557069348567, 3.892334458579129297, -69.75875473022499307 ) ) ;
#30935 = ORIENTED_EDGE ( 'NONE', *, *, #3884, .F. ) ;
#30936 = DIRECTION ( 'NONE',  ( 6.181422929335961825E-12, -0.4082287037029531107, -0.9128796883888953273 ) ) ;
#30937 = CARTESIAN_POINT ( 'NONE',  ( -4.072259770650454413, 2.021700601781299511, -56.79877225282499609 ) ) ;
#30938 = VERTEX_POINT ( 'NONE', #5373 ) ;
#30939 = CARTESIAN_POINT ( 'NONE',  ( -2.504034607669999968, -5.302315698040000136, 226.6412452697800006 ) ) ;
#30940 = CARTESIAN_POINT ( 'NONE',  ( -19.80535397421925481, 19.50875616500616871, 0.9999999989999952543 ) ) ;
#30941 = LINE ( 'NONE', #26068, #22555 ) ;
#30942 = CARTESIAN_POINT ( 'NONE',  ( -10.69999999999999929, -24.34033515279999804, -26.95726941919999931 ) ) ;
#30943 = LINE ( 'NONE', #16459, #8919 ) ;
#30944 = DIRECTION ( 'NONE',  ( 0.000000000000000000, 0.000000000000000000, 1.000000000000000000 ) ) ;
#30945 = ADVANCED_FACE ( 'NONE', ( #3465 ), #27804, .T. ) ;
#30946 = ORIENTED_EDGE ( 'NONE', *, *, #12673, .F. ) ;
#30947 = FACE_OUTER_BOUND ( 'NONE', #30111, .T. ) ;
#30948 = CARTESIAN_POINT ( 'NONE',  ( -9.738910687886855655, -24.96785170200598714, 86.78285841159998881 ) ) ;
#30949 = CARTESIAN_POINT ( 'NONE',  ( 20.25363919059999773, 20.00000851029999893, 229.3819260790000101 ) ) ;
#30950 = LINE ( 'NONE', #9544, #5712 ) ;
#30951 = CARTESIAN_POINT ( 'NONE',  ( 8.700000000231774777, -28.77591908717043268, -25.95027189104346732 ) ) ;
#30952 = CARTESIAN_POINT ( 'NONE',  ( -1.100001419170000050, -27.77850706310000106, 225.0000014190000002 ) ) ;
#30953 = CYLINDRICAL_SURFACE ( 'NONE', #150, 1.099999999999999201 ) ;
#30954 = CARTESIAN_POINT ( 'NONE',  ( -25.32653162617393861, 13.07087917251410403, 4.239730451999990102 ) ) ;
#30955 = CARTESIAN_POINT ( 'NONE',  ( 0.2617993877991457441, -2.000000000000001332, 227.6412452703546592 ) ) ;
#30956 = CARTESIAN_POINT ( 'NONE',  ( -0.9891938378274514054, -4.753657830815118501, -52.52706695232500067 ) ) ;
#30957 = LINE ( 'NONE', #19461, #8745 ) ;
#30958 = CARTESIAN_POINT ( 'NONE',  ( 14.00000000000000000, 20.99999999996851940, -58.04643232978019540 ) ) ;
#30959 = CARTESIAN_POINT ( 'NONE',  ( 18.05873143885011345, 10.34054669329053944, -0.6999999999999783062 ) ) ;
#30960 = VERTEX_POINT ( 'NONE', #15279 ) ;
#30961 = EDGE_CURVE ( 'NONE', #6970, #28945, #9945, .T. ) ;
#30962 = DIRECTION ( 'NONE',  ( -0.8775825618903718706, 0.4794255386042047262, 0.000000000000000000 ) ) ;
#30963 = ORIENTED_EDGE ( 'NONE', *, *, #11762, .F. ) ;
#30964 = CARTESIAN_POINT ( 'NONE',  ( -24.34159889609999894, -14.82483853620000147, 224.0986003170000060 ) ) ;
#30965 = CARTESIAN_POINT ( 'NONE',  ( -3.855177830964256813, -4.571422008809257420, -59.17407541852499975 ) ) ;
#30966 = ORIENTED_EDGE ( 'NONE', *, *, #19986, .F. ) ;
#30967 = EDGE_LOOP ( 'NONE', ( #20943, #10270, #1943, #23778, #16668 ) ) ;
#30968 = CARTESIAN_POINT ( 'NONE',  ( -9.999999999969999109, -24.00000000000000000, -28.40000000000000213 ) ) ;
#30969 = ORIENTED_EDGE ( 'NONE', *, *, #25565, .F. ) ;
#30970 = EDGE_CURVE ( 'NONE', #29654, #11652, #8446, .T. ) ;
#30971 = CARTESIAN_POINT ( 'NONE',  ( 1.680165880436631509, 1.289604810889001030, 226.6412452697800006 ) ) ;
#30972 = CARTESIAN_POINT ( 'NONE',  ( -8.699999999635686265, -13.70503196073122965, -39.86243280111477105 ) ) ;
#30973 = CARTESIAN_POINT ( 'NONE',  ( -27.87609112763809449, 3.928995115440388375, 8.000000000000007105 ) ) ;
#30974 = ADVANCED_FACE ( 'NONE', ( #29132 ), #691, .T. ) ;
#30975 = CARTESIAN_POINT ( 'NONE',  ( 0.4086195922400000513, -12.10538642919999930, 231.9999991140000191 ) ) ;
#30976 = CARTESIAN_POINT ( 'NONE',  ( -27.79539923781770483, -0.5057481688778081574, 1.000000000000000888 ) ) ;
#30977 = PLANE ( 'NONE',  #13938 ) ;
#30978 = CARTESIAN_POINT ( 'NONE',  ( -4.932711197237716227, 1.396981812416056457, -6.373327254900004846 ) ) ;
#30979 = CARTESIAN_POINT ( 'NONE',  ( -28.45771199730000234, 1.065814103639999922E-14, 229.4982322489999831 ) ) ;
#30980 = ORIENTED_EDGE ( 'NONE', *, *, #16479, .T. ) ;
#30981 = CARTESIAN_POINT ( 'NONE',  ( -24.68204616399999907, -14.25020164319999871, 223.9000014189999774 ) ) ;
#30982 = EDGE_CURVE ( 'NONE', #3651, #14873, #3550, .T. ) ;
#30983 = CARTESIAN_POINT ( 'NONE',  ( -3.117834729128555971, -4.866792379758847709, -18.70544088820000184 ) ) ;
#30984 = CARTESIAN_POINT ( 'NONE',  ( 28.34729902996195250, 3.134625972213187062, 8.000000000000007105 ) ) ;
#30985 = CARTESIAN_POINT ( 'NONE',  ( 24.35797964201644561, -13.39969403546014703, 6.098655031999994591 ) ) ;
#30986 = B_SPLINE_CURVE_WITH_KNOTS ( 'NONE', 5,
 ( #21443, #4914, #2095, #11686, #28816, #9793, #12143, #31041, #26165, #21751, #4599, #28674, #7118, #26320, #24118 ),
 .UNSPECIFIED., .F., .F.,
 ( 6, 3, 3, 3, 6 ),
 ( 0.000000000000000000, 0.1000000000045810078, 0.4000000000011452173, 0.7000000000005727196, 1.000000000000000000 ),
 .UNSPECIFIED. ) ;
#30987 = CARTESIAN_POINT ( 'NONE',  ( -11.34419785439999906, 4.447397017599999280, 230.6412452697800006 ) ) ;
#30988 = CARTESIAN_POINT ( 'NONE',  ( -15.73360964098195147, -8.979988381493612337, 0.000000000000000000 ) ) ;
#30989 = CARTESIAN_POINT ( 'NONE',  ( 0.5921542527520354815, -4.847825725899490124, -43.03057807742499818 ) ) ;
#30990 = DIRECTION ( 'NONE',  ( 0.000000000000000000, 0.000000000000000000, 1.000000000000000000 ) ) ;
#30991 = CARTESIAN_POINT ( 'NONE',  ( -23.67274795584174285, -12.56353887392313062, 4.451031837395022173 ) ) ;
#30992 = DIRECTION ( 'NONE',  ( 0.000000000000000000, -1.000000000000000000, 0.000000000000000000 ) ) ;
#30993 = EDGE_CURVE ( 'NONE', #22535, #528, #26856, .T. ) ;
#30994 = DIRECTION ( 'NONE',  ( 1.000000000000000000, -1.224606353820000075E-16, 0.000000000000000000 ) ) ;
#30995 = ORIENTED_EDGE ( 'NONE', *, *, #17385, .T. ) ;
#30996 = CARTESIAN_POINT ( 'NONE',  ( -10.00000000020000002, 19.99999999999999645, -2.208382156699995047 ) ) ;
#30997 = CARTESIAN_POINT ( 'NONE',  ( -7.105427357599999217E-15, 0.000000000000000000, 86.78285841159998881 ) ) ;
#30998 = VERTEX_POINT ( 'NONE', #11340 ) ;
#30999 = CARTESIAN_POINT ( 'NONE',  ( -2.220446049249999755E-16, -0.1455297029551360921, -71.05965357398815740 ) ) ;
#31000 = CARTESIAN_POINT ( 'NONE',  ( 0.000000000000000000, 0.000000000000000000, 40.00000000000000000 ) ) ;
#31001 = VERTEX_POINT ( 'NONE', #6139 ) ;
#31002 = EDGE_CURVE ( 'NONE', #2248, #24939, #25797, .T. ) ;
#31003 = ORIENTED_EDGE ( 'NONE', *, *, #26704, .T. ) ;
#31004 = AXIS2_PLACEMENT_3D ( 'NONE', #9839, #14569, #568 ) ;
#31005 = DIRECTION ( 'NONE',  ( 1.000000000000000000, 0.000000000000000000, 0.000000000000000000 ) ) ;
#31006 = ORIENTED_EDGE ( 'NONE', *, *, #7815, .F. ) ;
#31007 = CARTESIAN_POINT ( 'NONE',  ( -17.12044415977894474, -10.06939460809101305, 0.000000000000000000 ) ) ;
#31008 = VERTEX_POINT ( 'NONE', #20306 ) ;
#31009 = CARTESIAN_POINT ( 'NONE',  ( -2.664535259099999568E-14, -26.80000000000000071, 223.8999999999999773 ) ) ;
#31010 = CARTESIAN_POINT ( 'NONE',  ( 23.47637528925400474, 14.89020703987135086, 4.098700193000015091 ) ) ;
#31011 = CARTESIAN_POINT ( 'NONE',  ( -7.999999999628359504, -14.95611408987656965, -40.37595097054163773 ) ) ;
#31012 = CARTESIAN_POINT ( 'NONE',  ( 0.3623765971425356724, 4.318009531214683783, -35.69999999999999574 ) ) ;
#31013 = CARTESIAN_POINT ( 'NONE',  ( 18.62931254531553549, 19.99998787143272949, -0.6145042232417567973 ) ) ;
#31014 = CARTESIAN_POINT ( 'NONE',  ( 9.499999999789963567, -17.13335861488235423, -37.56236078282699253 ) ) ;
#31015 = FACE_OUTER_BOUND ( 'NONE', #28537, .T. ) ;
#31016 = CARTESIAN_POINT ( 'NONE',  ( -19.99487511799999950, 20.00000620269999985, 229.8488538259999814 ) ) ;
#31017 = ORIENTED_EDGE ( 'NONE', *, *, #7371, .F. ) ;
#31018 = B_SPLINE_CURVE_WITH_KNOTS ( 'NONE', 3,
 ( #12908, #26926, #5362, #17617, #17766, #14967 ),
 .UNSPECIFIED., .F., .F.,
 ( 4, 2, 4 ),
 ( 0.000000000000000000, 0.5000000000000000000, 1.000000000000000000 ),
 .UNSPECIFIED. ) ;
#31019 = CARTESIAN_POINT ( 'NONE',  ( -3.010188847181571870, -5.300177381000955812, -6.685065142700001850 ) ) ;
#31020 = CARTESIAN_POINT ( 'NONE',  ( 6.118976883090258667, 2.212479739890888197, -25.91249766019999967 ) ) ;
#31021 = DIRECTION ( 'NONE',  ( 0.5000000000001894040, 0.8660254037843291286, 0.000000000000000000 ) ) ;
#31022 =( BOUNDED_SURFACE ( )  B_SPLINE_SURFACE ( 5, 3, ( 
 ( #23016, #30411, #20804, #11054 ),
 ( #3334, #15923, #25533, #3643 ),
 ( #27562, #6162, #18274, #30243 ),
 ( #20646, #22551, #5699, #8357 ),
 ( #1139, #20179, #10732, #6008 ),
 ( #20332, #8202, #20488, #15306 ),
 ( #15606, #13239, #29930, #22856 ),
 ( #1302, #10896, #30088, #8514 ),
 ( #15764, #10585, #25378, #12943 ),
 ( #8674, #13566, #29770, #27413 ),
 ( #23172, #16080, #30874, #23642 ),
 ( #11517, #11831, #23488, #4285 ),
 ( #1926, #21589, #9304, #11671 ),
 ( #18904, #28034, #8993, #8831 ),
 ( #6947, #6478, #11977, #2079 ) ),
 .UNSPECIFIED., .F., .F., .T. ) 
 B_SPLINE_SURFACE_WITH_KNOTS ( ( 6, 3, 3, 3, 6 ),
 ( 4, 4 ),
 ( 10.99557428763625744, 13.78013078440000072, 16.56468728109999944, 19.34924377789999994, 22.13380027456373966 ),
 ( 0.000000000000000000, 1.000000000000000000 ),
 .UNSPECIFIED. ) 
 GEOMETRIC_REPRESENTATION_ITEM ( )  RATIONAL_B_SPLINE_SURFACE ( (
 ( 1.000000000000000000, 0.9492530301840010898, 0.9492530301840010898, 1.000000000000000000),
 ( 1.000000000000000000, 0.9492530301840010898, 0.9492530301840010898, 1.000000000000000000),
 ( 1.000000000000000000, 0.9492530301840010898, 0.9492530301840010898, 1.000000000000000000),
 ( 1.000000000000000000, 0.9492530301840010898, 0.9492530301840010898, 1.000000000000000000),
 ( 1.000000000000000000, 0.9492530301840010898, 0.9492530301840010898, 1.000000000000000000),
 ( 1.000000000000000000, 0.9492530301840010898, 0.9492530301840010898, 1.000000000000000000),
 ( 1.000000000000000000, 0.9492530301840010898, 0.9492530301840010898, 1.000000000000000000),
 ( 1.000000000000000000, 0.9492530301840010898, 0.9492530301840010898, 1.000000000000000000),
 ( 1.000000000000000000, 0.9492530301840010898, 0.9492530301840010898, 1.000000000000000000),
 ( 1.000000000000000000, 0.9492530301840010898, 0.9492530301840010898, 1.000000000000000000),
 ( 1.000000000000000000, 0.9492530301840010898, 0.9492530301840010898, 1.000000000000000000),
 ( 1.000000000000000000, 0.9492530301840010898, 0.9492530301840010898, 1.000000000000000000),
 ( 1.000000000000000000, 0.9492530301840010898, 0.9492530301840010898, 1.000000000000000000),
 ( 1.000000000000000000, 0.9492530301840010898, 0.9492530301840010898, 1.000000000000000000),
 ( 1.000000000000000000, 0.9492530301840010898, 0.9492530301840010898, 1.000000000000000000) ) ) 
 REPRESENTATION_ITEM ( '' )  SURFACE ( )  );
#31023 = FACE_OUTER_BOUND ( 'NONE', #3613, .T. ) ;
#31024 = CARTESIAN_POINT ( 'NONE',  ( 0.7404173758804706296, 3.499814327640350609, 227.6907824390132760 ) ) ;
#31025 = CARTESIAN_POINT ( 'NONE',  ( -23.81569860410000317, -13.75000000000000000, 226.0999999999999943 ) ) ;
#31026 = CARTESIAN_POINT ( 'NONE',  ( -3.052679639724400928, 3.117809041995142749, -4.568732180599999637 ) ) ;
#31027 = VECTOR ( 'NONE', #7850, 1000.000000000000000 ) ;
#31028 = AXIS2_PLACEMENT_3D ( 'NONE', #23751, #24359, #19329 ) ;
#31029 = LINE ( 'NONE', #21125, #7171 ) ;
#31030 = CARTESIAN_POINT ( 'NONE',  ( 7.312007425309012376, -6.582071621330287670, -34.26887834112514497 ) ) ;
#31031 = CARTESIAN_POINT ( 'NONE',  ( 2.020725942159999899, -3.500000000000000000, 230.5235986622430175 ) ) ;
#31032 = ADVANCED_FACE ( 'NONE', ( #1591 ), #3790, .T. ) ;
#31033 = ORIENTED_EDGE ( 'NONE', *, *, #22228, .F. ) ;
#31034 = ORIENTED_EDGE ( 'NONE', *, *, #21179, .T. ) ;
#31035 = EDGE_CURVE ( 'NONE', #20682, #5307, #18244, .T. ) ;
#31036 = CARTESIAN_POINT ( 'NONE',  ( 18.13765659361598281, 10.46359668135569976, -4.336808689942018722E-16 ) ) ;
#31037 = CARTESIAN_POINT ( 'NONE',  ( -3.665401116828205463, 4.874126016103034864, -19.63064294430000345 ) ) ;
#31038 = EDGE_LOOP ( 'NONE', ( #15399, #1026, #15669, #25420 ) ) ;
#31039 = EDGE_CURVE ( 'NONE', #26791, #12957, #3944, .T. ) ;
#31040 = CARTESIAN_POINT ( 'NONE',  ( 25.08428924680000094, -13.52916357279999993, 225.7601281139999969 ) ) ;
#31041 = CARTESIAN_POINT ( 'NONE',  ( 24.06750537026301018, 15.26514225575822081, 4.098700193000015091 ) ) ;
#31042 = VERTEX_POINT ( 'NONE', #1279 ) ;
#31043 = EDGE_LOOP ( 'NONE', ( #28782, #19966, #21519, #29172, #850, #29251, #16016, #7390 ) ) ;
#31044 = ORIENTED_EDGE ( 'NONE', *, *, #21221, .F. ) ;
#31045 = SHAPE_REPRESENTATION_RELATIONSHIP ( 'NONE' , 'NONE' ,  #27424, #17428 ) ;
#31046 = EDGE_LOOP ( 'NONE', ( #26738, #22180, #12719, #379 ) ) ;
#31047 = CARTESIAN_POINT ( 'NONE',  ( -17.49999999969999820, -25.48537695659676672, -31.01919234699705186 ) ) ;
#31048 = CARTESIAN_POINT ( 'NONE',  ( 28.35455043824866550, 0.5159221438580617880, 0.2374258030000131470 ) ) ;
#31049 = CARTESIAN_POINT ( 'NONE',  ( -0.4334975989126229612, 2.694277338339795769, -67.89769279494433363 ) ) ;
#31050 = ORIENTED_EDGE ( 'NONE', *, *, #1416, .F. ) ;
#31051 = CARTESIAN_POINT ( 'NONE',  ( -10.69999999999999929, -27.00000000000000000, -28.40000000000000213 ) ) ;
#31052 = TOROIDAL_SURFACE ( 'NONE', #30561, 24.50000000000000000, 4.000000000000000000 ) ;
#31053 = AXIS2_PLACEMENT_3D ( 'NONE', #7955, #3390, #15362 ) ;
#31054 = LINE ( 'NONE', #23672, #19695 ) ;
#31055 = AXIS2_PLACEMENT_3D ( 'NONE', #8387, #3520, #25248 ) ;
#31056 = CARTESIAN_POINT ( 'NONE',  ( 28.46656763489999875, -1.746773142929999967, 222.0000000000000000 ) ) ;
#31057 = DIRECTION ( 'NONE',  ( 0.000000000000000000, 1.000000000000000000, 0.000000000000000000 ) ) ;
#31058 = ORIENTED_EDGE ( 'NONE', *, *, #21840, .T. ) ;
#31059 = LINE ( 'NONE', #6825, #14008 ) ;
#31060 = CARTESIAN_POINT ( 'NONE',  ( -4.180754675048084401, 1.217138862148065659, -15.80443125760000456 ) ) ;
#31061 = FACE_OUTER_BOUND ( 'NONE', #29135, .T. ) ;
#31062 = CARTESIAN_POINT ( 'NONE',  ( 0.6483608293613253304, -27.49254329982320399, 5.909562041028879165 ) ) ;
#31063 = EDGE_LOOP ( 'NONE', ( #20908, #1705, #18177, #28103, #203 ) ) ;
#31064 = CARTESIAN_POINT ( 'NONE',  ( 8.000000000742927497, -28.90964379103893123, -30.74680062208867071 ) ) ;
#31065 = CARTESIAN_POINT ( 'NONE',  ( 8.999999999770000869, 21.70000000000000284, -45.10000000000000142 ) ) ;
#31066 = CARTESIAN_POINT ( 'NONE',  ( 23.16094352345281138, -13.48406906521379334, 6.099999999996507327 ) ) ;
#31067 = AXIS2_PLACEMENT_3D ( 'NONE', #15551, #3916, #18060 ) ;
#31068 = FACE_OUTER_BOUND ( 'NONE', #748, .T. ) ;
#31069 = CARTESIAN_POINT ( 'NONE',  ( -3.807105672873282831, -5.136256491778199873, -65.13409070562501313 ) ) ;
#31070 = CARTESIAN_POINT ( 'NONE',  ( 0.000000000000000000, 0.000000000000000000, 190.0000000000000000 ) ) ;
#31071 = CARTESIAN_POINT ( 'NONE',  ( -17.04621913067799710, -32.00000000000000000, -31.28675134614999820 ) ) ;
#31072 = EDGE_LOOP ( 'NONE', ( #23189, #12535, #9068, #27533 ) ) ;
#31073 = CARTESIAN_POINT ( 'NONE',  ( 18.13191322229999969, -9.527368092500001495, -0.7999999992999995424 ) ) ;
#31074 = DIRECTION ( 'NONE',  ( 0.000000000000000000, 0.3420201433259318358, -0.9396926207858125046 ) ) ;
#31075 = CIRCLE ( 'NONE', #17494, 3.000000000000001332 ) ;
#31076 = ADVANCED_FACE ( 'NONE', ( #8333 ), #23148, .T. ) ;
#31077 = DIRECTION ( 'NONE',  ( -1.000000000000000000, 1.224606353819999829E-16, 0.000000000000000000 ) ) ;
#31078 = AXIS2_PLACEMENT_3D ( 'NONE', #9690, #9069, #9215 ) ;
#31079 = EDGE_CURVE ( 'NONE', #22666, #11888, #28168, .T. ) ;
#31080 = ORIENTED_EDGE ( 'NONE', *, *, #21569, .F. ) ;
#31081 = DIRECTION ( 'NONE',  ( -0.000000000000000000, -0.000000000000000000, -1.000000000000000000 ) ) ;
#31082 = PRODUCT_DEFINITION_SHAPE ( 'NONE', 'NONE',  #31133 ) ;
#31083 = ORIENTED_EDGE ( 'NONE', *, *, #30622, .T. ) ;
#31084 = DIRECTION ( 'NONE',  ( 0.000000000000000000, 0.000000000000000000, 1.000000000000000000 ) ) ;
#31085 = CARTESIAN_POINT ( 'NONE',  ( 23.80092420482279891, 14.36517094565843777, 6.099998581000020792 ) ) ;
#31086 = VERTEX_POINT ( 'NONE', #13380 ) ;
#31087 = CARTESIAN_POINT ( 'NONE',  ( -20.80531994253358974, 17.08514196121145545, 0.000000000000000000 ) ) ;
#31088 = AXIS2_PLACEMENT_3D ( 'NONE', #1133, #13079, #8351 ) ;
#31089 = CARTESIAN_POINT ( 'NONE',  ( -3.112296099710462727, 3.758517760630103233, -62.99933298492499034 ) ) ;
#31090 = CARTESIAN_POINT ( 'NONE',  ( -18.95046173579999760, -18.95046173579999760, 143.2171415880000040 ) ) ;
#31091 = VECTOR ( 'NONE', #22257, 1000.000000000000000 ) ;
#31092 = CARTESIAN_POINT ( 'NONE',  ( 11.20000000009999930, -22.00000000000000000, -28.39999999955988841 ) ) ;
#31093 = CARTESIAN_POINT ( 'NONE',  ( -10.69999999999999929, -25.00000000000000000, -26.16393202249999916 ) ) ;
#31094 = CARTESIAN_POINT ( 'NONE',  ( 3.145769537974499208, 1.551367331320289145, 230.8336439985931179 ) ) ;
#31095 = VECTOR ( 'NONE', #469, 999.9999999999998863 ) ;
#31096 = CARTESIAN_POINT ( 'NONE',  ( 3.748453146079709697, -2.489798990173139437, -35.69999999999999574 ) ) ;
#31097 = CARTESIAN_POINT ( 'NONE',  ( 9.500000000000000000, 21.70000000000000284, -60.10000000019999788 ) ) ;
#31098 = ORIENTED_EDGE ( 'NONE', *, *, #23903, .T. ) ;
#31099 = DIRECTION ( 'NONE',  ( -1.000000000000000000, 5.665498452320000818E-16, 0.000000000000000000 ) ) ;
#31100 = CARTESIAN_POINT ( 'NONE',  ( 10.69999999996243290, -28.46594883620507588, -25.75514764082761587 ) ) ;
#31101 = EDGE_CURVE ( 'NONE', #4546, #28608, #193, .T. ) ;
#31102 = CARTESIAN_POINT ( 'NONE',  ( 18.92330595649999836, 19.72869720889999812, 229.8506619570000282 ) ) ;
#31103 = CARTESIAN_POINT ( 'NONE',  ( -25.27355175290000133, 12.75978488059999805, 222.0000000000000000 ) ) ;
#31104 = CARTESIAN_POINT ( 'NONE',  ( 22.03727920249266248, 17.02869341850189855, 6.333333333333394322 ) ) ;
#31105 = CARTESIAN_POINT ( 'NONE',  ( -0.1058797546490000130, -28.50006311429999784, 226.0959516479999820 ) ) ;
#31106 = CARTESIAN_POINT ( 'NONE',  ( 16.20123158649999695, 11.52736809289999620, -1.399999999999998579 ) ) ;
#31107 = FACE_OUTER_BOUND ( 'NONE', #9199, .T. ) ;
#31108 = CARTESIAN_POINT ( 'NONE',  ( 24.00345430277922887, -14.02483715947875176, 226.1000014189999661 ) ) ;
#31109 = VECTOR ( 'NONE', #7368, 1000.000000000000000 ) ;
#31110 = B_SPLINE_SURFACE_WITH_KNOTS ( 'NONE', 5, 1, ( 
 ( #4607, #9487 ),
 ( #23817, #2414 ),
 ( #21610, #24124 ),
 ( #2563, #2265 ),
 ( #21761, #209 ),
 ( #9800, #28988 ),
 ( #17031, #22537 ),
 ( #14988, #29451 ),
 ( #5224, #5381 ) ),
 .UNSPECIFIED., .F., .F., .F.,
 ( 6, 3, 6 ),
 ( 2, 2 ),
 ( 0.000000000000000000, 55.31395511720000258, 94.75474465359999954 ),
 ( -3.500000000000000000, 3.500000000000000000 ),
 .UNSPECIFIED. ) ;
#31111 = CARTESIAN_POINT ( 'NONE',  ( 1.087346358790000053E-15, 2.000000000000000000, 227.6412452699999847 ) ) ;
#31112 = CARTESIAN_POINT ( 'NONE',  ( -26.80000000000000071, -7.283063041539999493E-14, 230.0000000000000000 ) ) ;
#31113 = CARTESIAN_POINT ( 'NONE',  ( -4.000000000000000000, -29.96004123392021157, -79.78289277550334191 ) ) ;
#31114 = ORIENTED_EDGE ( 'NONE', *, *, #2366, .T. ) ;
#31115 = DIRECTION ( 'NONE',  ( -0.8090169943751909232, 0.5877852522921378498, 0.000000000000000000 ) ) ;
#31116 = ORIENTED_EDGE ( 'NONE', *, *, #14521, .T. ) ;
#31117 = CARTESIAN_POINT ( 'NONE',  ( -8.699999999668209583, -9.149979920083866958, -35.02638174926116221 ) ) ;
#31118 = CLOSED_SHELL ( 'NONE', ( #1187, #26980, #30594, #5448, #13109, #30687, #27289, #21987, #29456, #27132, #30922, #2485, #30314, #14467, #13671, #17206, #11000, #18625, #28715, #12903, #23373, #23705, #558, #21059, #17554, #9826, #12664, #30818 ) ) ;
#31119 = NEXT_ASSEMBLY_USAGE_OCCURRENCE ( 'NAUO1', ' ', ' ', #30228, #3296, $ ) ;
#31120 = NEXT_ASSEMBLY_USAGE_OCCURRENCE ( 'NAUO2', ' ', ' ', #30228, #4619, $ ) ;
#31121 = NEXT_ASSEMBLY_USAGE_OCCURRENCE ( 'NAUO3', ' ', ' ', #30228, #2325, $ ) ;
#31122 = NEXT_ASSEMBLY_USAGE_OCCURRENCE ( 'NAUO4', ' ', ' ', #30228, #8875, $ ) ;
#31123 = NEXT_ASSEMBLY_USAGE_OCCURRENCE ( 'NAUO5', ' ', ' ', #30228, #54, $ ) ;
#31124 = NEXT_ASSEMBLY_USAGE_OCCURRENCE ( 'NAUO6', ' ', ' ', #30228, #21398, $ ) ;
#31125 = NEXT_ASSEMBLY_USAGE_OCCURRENCE ( 'NAUO7', ' ', ' ', #30228, #7911, $ ) ;
#31126 = NEXT_ASSEMBLY_USAGE_OCCURRENCE ( 'NAUO8', ' ', ' ', #30228, #5604, $ ) ;
#31127 = NEXT_ASSEMBLY_USAGE_OCCURRENCE ( 'NAUO9', ' ', ' ', #30228, #18101, $ ) ;
#31128 = NEXT_ASSEMBLY_USAGE_OCCURRENCE ( 'NAUO10', ' ', ' ', #30228, #26933, $ ) ;
#31129 = NEXT_ASSEMBLY_USAGE_OCCURRENCE ( 'NAUO11', ' ', ' ', #30228, #17, $ ) ;
#31130 = NEXT_ASSEMBLY_USAGE_OCCURRENCE ( 'NAUO12', ' ', ' ', #30228, #15813, $ ) ;
#31131 = NEXT_ASSEMBLY_USAGE_OCCURRENCE ( 'NAUO13', ' ', ' ', #30228, #22352, $ ) ;
#31132 = NEXT_ASSEMBLY_USAGE_OCCURRENCE ( 'NAUO14', ' ', ' ', #30228, #4652, $ ) ;
#31133 = NEXT_ASSEMBLY_USAGE_OCCURRENCE ( 'NAUO15', ' ', ' ', #30228, #24622, $ ) ;
#31134 = NEXT_ASSEMBLY_USAGE_OCCURRENCE ( 'NAUO16', ' ', ' ', #30228, #2358, $ ) ;
#31135 = NEXT_ASSEMBLY_USAGE_OCCURRENCE ( 'NAUO17', ' ', ' ', #30228, #15768, $ ) ;
#31136 = NEXT_ASSEMBLY_USAGE_OCCURRENCE ( 'NAUO18', ' ', ' ', #30228, #22352, $ ) ;
#31137 = NEXT_ASSEMBLY_USAGE_OCCURRENCE ( 'NAUO19', ' ', ' ', #30228, #22352, $ ) ;
#31138 = NEXT_ASSEMBLY_USAGE_OCCURRENCE ( 'NAUO20', ' ', ' ', #30228, #22352, $ ) ;
#31139 = NEXT_ASSEMBLY_USAGE_OCCURRENCE ( 'NAUO21', ' ', ' ', #30228, #22352, $ ) ;
#31140 = NEXT_ASSEMBLY_USAGE_OCCURRENCE ( 'NAUO22', ' ', ' ', #30228, #22352, $ ) ;
#31141 = NEXT_ASSEMBLY_USAGE_OCCURRENCE ( 'NAUO23', ' ', ' ', #30228, #22352, $ ) ;
#31142 = NEXT_ASSEMBLY_USAGE_OCCURRENCE ( 'NAUO24', ' ', ' ', #30228, #22352, $ ) ;
#31143 = NEXT_ASSEMBLY_USAGE_OCCURRENCE ( 'NAUO25', ' ', ' ', #30228, #22352, $ ) ;
#31144 = NEXT_ASSEMBLY_USAGE_OCCURRENCE ( 'NAUO26', ' ', ' ', #30228, #22352, $ ) ;
ENDSEC;
END-ISO-10303-21;
